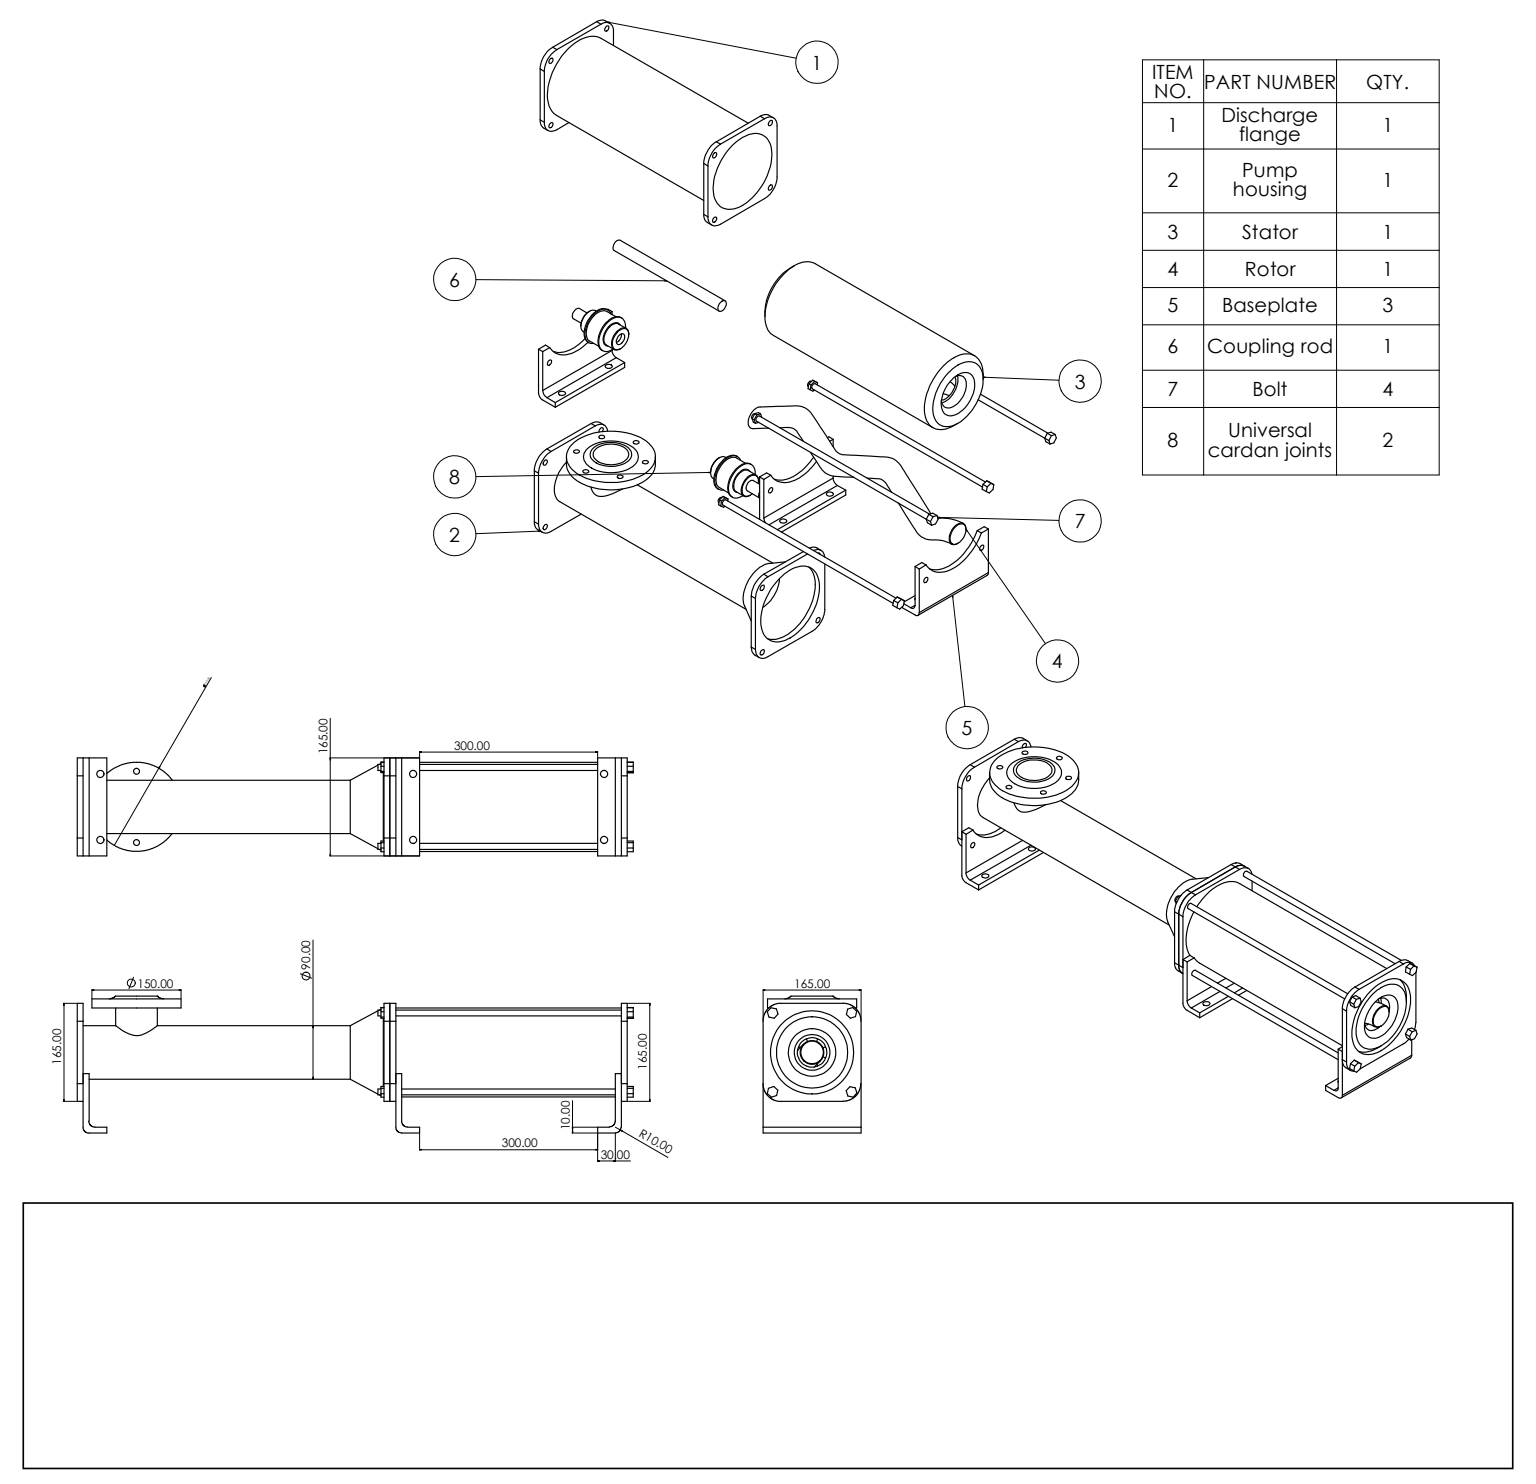
ISO-10303-21;
HEADER;
FILE_DESCRIPTION (('STEP AP214'),
    '1' );
FILE_NAME ('MAS-348',
    '2026-10-27T19:20:31',
    ( '' ),
    ( '' ),
    'SwSTEP 2.0',
    'SolidWorks 2025',
    '' );
FILE_SCHEMA (( 'AUTOMOTIVE_DESIGN' ));
ENDSEC;

DATA;
#1 = CARTESIAN_POINT ( 'NONE',  ( 14.38125909742182529, -39.99999999999944578, -55.17850393971050238 ) ) ;
#2 = CARTESIAN_POINT ( 'NONE',  ( -198.0356074513804572, -9.007331120208026888E-14, 15.37879056873070560 ) ) ;
#3 = CARTESIAN_POINT ( 'NONE',  ( 4.995406935893293543, -15.24977328854832592, 0.000000000000000000 ) ) ;
#4 = CARTESIAN_POINT ( 'NONE',  ( 163.1118516004056573, -9.006482792069636645, 9.006482792069567367 ) ) ;
#5 = CARTESIAN_POINT ( 'NONE',  ( -259.2033419157646676, 9.517827891722584255, -0.000000000000000000 ) ) ;
#6 = CARTESIAN_POINT ( 'NONE',  ( 0.2972598230770027716, -38.42060263243656237, -18.14793986248737667 ) ) ;
#7 = DIRECTION ( 'NONE',  ( 0.000000000000000000, 0.000000000000000000, -1.000000000000000000 ) ) ;
#8 =( GEOMETRIC_REPRESENTATION_CONTEXT ( 3 ) GLOBAL_UNCERTAINTY_ASSIGNED_CONTEXT ( ( #20296 ) ) GLOBAL_UNIT_ASSIGNED_CONTEXT ( ( #22388, #16248, #14122 ) ) REPRESENTATION_CONTEXT ( 'NONE', 'WORKASPACE' ) );
#9 = CARTESIAN_POINT ( 'NONE',  ( -200.0000000000000000, -52.49999999999992895, -52.49999999999999289 ) ) ;
#10 = CARTESIAN_POINT ( 'NONE',  ( 0.2972598230769957217, 1.502051041545559470E-13, -14.33493731733933352 ) ) ;
#11 = CARTESIAN_POINT ( 'NONE',  ( 130.8568914410475372, 8.154165912415230659E-16, 5.949712681206690945 ) ) ;
#12 = CARTESIAN_POINT ( 'NONE',  ( 184.8905102610680444, 13.49065550809807945, 13.49065550809809544 ) ) ;
#13 = CARTESIAN_POINT ( 'NONE',  ( 146.6084372240433709, -3.800685668859084210, 52.76785682606516303 ) ) ;
#14 = CARTESIAN_POINT ( 'NONE',  ( -190.0144721488653943, -13.91469502169275962, -47.57279682962041534 ) ) ;
#15 = CARTESIAN_POINT ( 'NONE',  ( -198.0356074513804572, -39.15871834505905724, -17.40982414986491733 ) ) ;
#16 = ORIENTED_EDGE ( 'NONE', *, *, #6629, .F. ) ;
#17 = CARTESIAN_POINT ( 'NONE',  ( 146.6084372240433993, -24.48358557860353457, 24.48358557860296258 ) ) ;
#18 = LINE ( 'NONE', #3258, #24208 ) ;
#19 = CARTESIAN_POINT ( 'NONE',  ( -192.9588430854689989, -14.46834944099973086, 0.000000000000000000 ) ) ;
#20 = CARTESIAN_POINT ( 'NONE',  ( -678.9461782662772293, 90.00000000000000000, 30.00000000000158096 ) ) ;
#21 = CARTESIAN_POINT ( 'NONE',  ( -100.7734535825088500, -44.31723036834885932, -12.25131212657538171 ) ) ;
#22 = DIRECTION ( 'NONE',  ( 0.000000000000000000, 0.000000000000000000, 1.000000000000000000 ) ) ;
#23 = CARTESIAN_POINT ( 'NONE',  ( -82.23866954411506924, 1.261533135296079022, 20.16514221458300682 ) ) ;
#24 = ORIENTED_EDGE ( 'NONE', *, *, #545, .T. ) ;
#25 = CARTESIAN_POINT ( 'NONE',  ( 199.9999999999999432, 19.00168160052138333, -0.2996653188340382967 ) ) ;
#26 = CARTESIAN_POINT ( 'NONE',  ( 22.89172254855152389, -23.44749030158411074, 43.00256445985486664 ) ) ;
#27 = CARTESIAN_POINT ( 'NONE',  ( -4.004886986946876171, 13.82996668233325721, 47.00296421444863171 ) ) ;
#28 = ORIENTED_EDGE ( 'NONE', *, *, #15718, .T. ) ;
#29 = ORIENTED_EDGE ( 'NONE', *, *, #2591, .T. ) ;
#30 = CARTESIAN_POINT ( 'NONE',  ( -208.1127848780265026, 15.00245453012665564, 0.000000000000000000 ) ) ;
#31 = CARTESIAN_POINT ( 'NONE',  ( 199.0062801237116332, 7.031410157601610145, -18.72090521856086198 ) ) ;
#32 = CARTESIAN_POINT ( 'NONE',  ( -190.0000000000000000, 52.50000000000007816, 52.49999999999999289 ) ) ;
#33 = CARTESIAN_POINT ( 'NONE',  ( -30.26275506840324070, 1.198031551616013601, 1.198031551616023371 ) ) ;
#34 = DIRECTION ( 'NONE',  ( 0.000000000000000000, 0.000000000000000000, 1.000000000000000000 ) ) ;
#35 = CARTESIAN_POINT ( 'NONE',  ( 199.9999999999999432, -1.727494763561684666E-13, 20.00000000000010303 ) ) ;
#36 = CARTESIAN_POINT ( 'NONE',  ( 200.0000000000002274, -16.15590588650048787, 10.03807108387658786 ) ) ;
#37 = CARTESIAN_POINT ( 'NONE',  ( 170.0000000000000000, 1.183443619805854272E-13, -24.95097643317000546 ) ) ;
#38 = DIRECTION ( 'NONE',  ( -1.836970198721030427E-16, 1.000000000000000000, -1.682156097916904327E-16 ) ) ;
#39 = CARTESIAN_POINT ( 'NONE',  ( 199.0246859915949642, -4.071254240408448410, 19.58630271169732140 ) ) ;
#40 = DIRECTION ( 'NONE',  ( 0.000000000000000000, -0.000000000000000000, 1.000000000000000000 ) ) ;
#41 = CARTESIAN_POINT ( 'NONE',  ( 12.96694272553733107, -24.77464205076947223, -44.79869582454342236 ) ) ;
#42 = CARTESIAN_POINT ( 'NONE',  ( -213.1075012329536946, -37.98287015391210275, -37.98287015391272092 ) ) ;
#43 = EDGE_CURVE ( 'NONE', #19077, #10069, #15238, .T. ) ;
#44 = CARTESIAN_POINT ( 'NONE',  ( -200.0000000000000000, 18.14877749763656212, 46.38610861938588670 ) ) ;
#45 = CARTESIAN_POINT ( 'NONE',  ( 146.6084372240433709, -32.08495691632041513, -24.48358557860343154 ) ) ;
#46 = CARTESIAN_POINT ( 'NONE',  ( -77.61444910505676376, 3.470426107442325048, 21.81614215779332966 ) ) ;
#47 = CARTESIAN_POINT ( 'NONE',  ( -213.1075012329537230, -9.698598906450422774, -9.698598906450550672 ) ) ;
#48 = CARTESIAN_POINT ( 'NONE',  ( -208.1127848780264742, -55.00245453012676222, -2.449293598294708485E-15 ) ) ;
#49 = EDGE_CURVE ( 'NONE', #17928, #4130, #15424, .T. ) ;
#50 = FACE_OUTER_BOUND ( 'NONE', #10007, .T. ) ;
#51 = CIRCLE ( 'NONE', #14477, 30.00000000000003908 ) ;
#52 = CARTESIAN_POINT ( 'NONE',  ( -192.9588430854689705, -54.46834944099975928, -2.449293598294708485E-15 ) ) ;
#53 = AXIS2_PLACEMENT_3D ( 'NONE', #25264, #21266, #19008 ) ;
#54 = CARTESIAN_POINT ( 'NONE',  ( -114.6180193230984372, 19.15387080987368762, 10.88873798880637622 ) ) ;
#55 = CARTESIAN_POINT ( 'NONE',  ( -30.26275506840325136, 40.00000000000003553, -1.694272468445841007 ) ) ;
#56 = EDGE_CURVE ( 'NONE', #12829, #11587, #7928, .T. ) ;
#57 = CARTESIAN_POINT ( 'NONE',  ( -30.26275506840325136, 29.48230279907798135, -27.08623969584585112 ) ) ;
#58 = EDGE_CURVE ( 'NONE', #18547, #5841, #11121, .T. ) ;
#59 = CARTESIAN_POINT ( 'NONE',  ( -198.0356074513804572, 15.37879056873066830, -40.00000000000002132 ) ) ;
#60 = VERTEX_POINT ( 'NONE', #18074 ) ;
#61 = VERTEX_POINT ( 'NONE', #13950 ) ;
#62 = CARTESIAN_POINT ( 'NONE',  ( 146.6084372240433709, -34.62501878078303008, 40.00000000000002132 ) ) ;
#63 = CARTESIAN_POINT ( 'NONE',  ( -86.86493150571118349, -7.943527260495776510, -19.77569912839190280 ) ) ;
#64 = CARTESIAN_POINT ( 'NONE',  ( -259.2033419157646676, -40.00000000000017764, 30.48217210827725054 ) ) ;
#65 = CIRCLE ( 'NONE', #6032, 14.99999999999999822 ) ;
#66 = CARTESIAN_POINT ( 'NONE',  ( -259.2033419157646676, 21.55415060305860209, -21.55415060305812602 ) ) ;
#67 = CARTESIAN_POINT ( 'NONE',  ( -280.0000000000000568, -20.00000000000006750, 40.00000000000002132 ) ) ;
#68 = CARTESIAN_POINT ( 'NONE',  ( -210.0000000000000284, -52.49999999999991473, 82.49999999999998579 ) ) ;
#69 = DIRECTION ( 'NONE',  ( 1.018913292508929218E-14, 1.000000000000000000, 8.144542348679703993E-15 ) ) ;
#70 = CARTESIAN_POINT ( 'NONE',  ( 200.0000000000001421, 16.62132632430557777, -9.210632111445709924 ) ) ;
#71 = CARTESIAN_POINT ( 'NONE',  ( 199.9999999999999432, -18.84870794256249482, 2.485603278128234450 ) ) ;
#72 = CARTESIAN_POINT ( 'NONE',  ( 91.82158438592158234, 44.40256751092319121, 12.16597498400105515 ) ) ;
#73 = CARTESIAN_POINT ( 'NONE',  ( -91.56559293963836410, -12.25131212657524138, 44.31723036834888774 ) ) ;
#74 = DIRECTION ( 'NONE',  ( -1.000000000000000000, 0.000000000000000000, 0.000000000000000000 ) ) ;
#75 = CARTESIAN_POINT ( 'NONE',  ( 14.38125909742181108, 1.616281842095393922E-13, -15.17850393972633682 ) ) ;
#76 = CARTESIAN_POINT ( 'NONE',  ( -198.0356074513804572, -67.44298959253333692, -10.87444709761016348 ) ) ;
#77 = CARTESIAN_POINT ( 'NONE',  ( -87.08883615166502068, 12.58652615577663170, -17.39726528837345398 ) ) ;
#78 = CARTESIAN_POINT ( 'NONE',  ( -213.1075012329537230, -18.58567234101155208, 37.98287015391234434 ) ) ;
#79 = CARTESIAN_POINT ( 'NONE',  ( -100.7734535825088500, -12.25131212657462498, -44.31723036834905827 ) ) ;
#80 = CARTESIAN_POINT ( 'NONE',  ( 199.0199757207951734, 7.646550829590152532, 18.48267855362066214 ) ) ;
#82 = CARTESIAN_POINT ( 'NONE',  ( -208.1127848780265026, -2.327190355601776466E-13, 55.00245453012672670 ) ) ;
#81 = CARTESIAN_POINT ( 'NONE',  ( -100.7734535825088358, 12.25131212657497848, -12.25131212657469604 ) ) ;
#83 = CARTESIAN_POINT ( 'NONE',  ( 19.06497207195980792, 66.60410523465830579, -10.03556273973354251 ) ) ;
#84 = AXIS2_PLACEMENT_3D ( 'NONE', #861, #18677, #15078 ) ;
#85 = CARTESIAN_POINT ( 'NONE',  ( 23.42154907652883011, 42.84253412640345715, -23.32998349128526883 ) ) ;
#86 = CARTESIAN_POINT ( 'NONE',  ( 192.4448373802100889, 19.99999999996064304, 2.449293598294708485E-15 ) ) ;
#87 = VERTEX_POINT ( 'NONE', #1727 ) ;
#88 = CARTESIAN_POINT ( 'NONE',  ( 192.4448373802100889, -14.14213562375876698, -14.14213562375885047 ) ) ;
#89 = CARTESIAN_POINT ( 'NONE',  ( -62.79433447042063676, -25.93934121795946268, 9.335111860881914581 ) ) ;
#90 = CARTESIAN_POINT ( 'NONE',  ( -280.0000000000000568, 19.99999999999995737, 40.00000000000002132 ) ) ;
#91 = ORIENTED_EDGE ( 'NONE', *, *, #1926, .F. ) ;
#92 = CARTESIAN_POINT ( 'NONE',  ( 12.01361959687201519, 24.84115733209565136, -44.88892880200794622 ) ) ;
#93 = CARTESIAN_POINT ( 'NONE',  ( 199.9999999999998863, -17.04947422730185025, -8.406841951002201441 ) ) ;
#94 = CARTESIAN_POINT ( 'NONE',  ( 20.91285618074969221, -23.84652503050088512, 43.54130497316993598 ) ) ;
#95 = CARTESIAN_POINT ( 'NONE',  ( -2.164901439630326330, 23.84421257770968339, -43.53794903252429549 ) ) ;
#96 = CARTESIAN_POINT ( 'NONE',  ( 199.0132273568269170, -10.00203194272371476, -17.32088655864767190 ) ) ;
#97 = VECTOR ( 'NONE', #21456, 1000.000000000000000 ) ;
#98 = CARTESIAN_POINT ( 'NONE',  ( 151.7948205124836250, -3.202120068677277203E-13, 33.23291073765553705 ) ) ;
#99 = CARTESIAN_POINT ( 'NONE',  ( 154.0339099654741801, -28.18615453125293513, 11.67508747798861002 ) ) ;
#100 = CARTESIAN_POINT ( 'NONE',  ( -166.3490736466491740, -19.13702016930768579, 36.43932733844285821 ) ) ;
#101 = CARTESIAN_POINT ( 'NONE',  ( 163.1118516004056573, 9.006482792069759213, -9.006482792069505194 ) ) ;
#102 = DIRECTION ( 'NONE',  ( -1.000000000000000000, -1.836970198721030181E-16, 0.000000000000000000 ) ) ;
#104 = CARTESIAN_POINT ( 'NONE',  ( 91.82158438592158234, -12.16597498397778843, 12.16597498397750954 ) ) ;
#103 = CARTESIAN_POINT ( 'NONE',  ( -188.4265466358324090, 13.83489705870430519, -47.03621809928684172 ) ) ;
#105 = CARTESIAN_POINT ( 'NONE',  ( -56.48582580120559271, -6.472252184284276844, 6.472252184284108978 ) ) ;
#106 = CARTESIAN_POINT ( 'NONE',  ( 91.82158438592159655, -22.79471317813468545, -40.00000000000002132 ) ) ;
#107 = CARTESIAN_POINT ( 'NONE',  ( -208.1127848780264742, 55.00245453010919050, -40.00000000000002132 ) ) ;
#108 = CARTESIAN_POINT ( 'NONE',  ( -105.3755690713226585, -40.00000000000027711, 21.75974354311608749 ) ) ;
#109 = CARTESIAN_POINT ( 'NONE',  ( 0.2972598230770011618, 10.13633138497462305, 66.70487387989858519 ) ) ;
#110 = CARTESIAN_POINT ( 'NONE',  ( -96.94475454975007267, 20.58449551010169998, -9.001119816636389714 ) ) ;
#111 = CARTESIAN_POINT ( 'NONE',  ( 130.8568914410475372, -4.207082182992785135, -4.207082182992884611 ) ) ;
#112 = ORIENTED_EDGE ( 'NONE', *, *, #21174, .F. ) ;
#113 = CARTESIAN_POINT ( 'NONE',  ( 0.2972598230769938343, 10.13633138497472252, 10.13633138497475628 ) ) ;
#114 = CARTESIAN_POINT ( 'NONE',  ( -97.73806390046776471, 8.581719943994480460, 20.71810467721184423 ) ) ;
#115 = CONTEXT_DEPENDENT_SHAPE_REPRESENTATION ( #703, #24194 ) ;
#116 = ORIENTED_EDGE ( 'NONE', *, *, #25089, .T. ) ;
#117 = EDGE_CURVE ( 'NONE', #6149, #16510, #26225, .T. ) ;
#118 = ORIENTED_EDGE ( 'NONE', *, *, #8682, .F. ) ;
#119 = B_SPLINE_CURVE_WITH_KNOTS ( 'NONE', 3,
 ( #4293, #2821, #10524, #19041, #16643, #4682, #8526, #24772, #8927, #6525, #20776, #20510, #2282, #14636, #22773, #8662, #10391, #6395, #24904, #14511, #14774, #22904, #12785, #20912, #2691, #18907, #15039, #23170, #13054, #25298, #21172, #4948, #17164, #2945 ),
 .UNSPECIFIED., .F., .F.,
 ( 4, 2, 2, 2, 2, 2, 2, 2, 2, 2, 2, 2, 2, 2, 2, 2, 4 ),
 ( -5.298243351204090312E-05, 0.01887868273877536807, 0.02834451532491907844, 0.03071097347145498174, 0.03307743161799089199, 0.03544388976452679529, 0.03781034791106269860, 0.04254326420413442889, 0.04727618049720615223, 0.04964263864374202084, 0.05200909679027788945, 0.05674201308334969607, 0.05910847122988561325, 0.06029170030315351980, 0.06147492937642144023, 0.06620784566949308725, 0.07567367825563638128 ),
 .UNSPECIFIED. ) ;
#120 = CARTESIAN_POINT ( 'NONE',  ( 57.59792236341147031, -26.56190807104670171, -30.00663442387710234 ) ) ;
#121 = CARTESIAN_POINT ( 'NONE',  ( 22.75882399337409367, -43.17886244245828919, -17.88527043150862283 ) ) ;
#122 = VERTEX_POINT ( 'NONE', #3583 ) ;
#123 = CARTESIAN_POINT ( 'NONE',  ( 151.7948205124836250, -33.23291073765550863, 0.000000000000000000 ) ) ;
#124 = CARTESIAN_POINT ( 'NONE',  ( -77.90255099906771363, -8.644468104261237684, -20.04994828523970440 ) ) ;
#125 = ORIENTED_EDGE ( 'NONE', *, *, #9291, .T. ) ;
#126 = SHAPE_REPRESENTATION ( 'Rotor', ( #21058 ), #20184 ) ;
#127 = CARTESIAN_POINT ( 'NONE',  ( 199.9999999999999432, 17.49244587396685091, 7.427265670988617785 ) ) ;
#128 = CARTESIAN_POINT ( 'NONE',  ( -83.21262154144230294, -33.12752917117752105, 13.72187187063023472 ) ) ;
#129 = CARTESIAN_POINT ( 'NONE',  ( -86.96347745069644475, 12.89780903124410472, -43.67073346367977393 ) ) ;
#130 = CARTESIAN_POINT ( 'NONE',  ( -187.8779108535587739, -43.02987313851080131, -17.82355704116172745 ) ) ;
#131 = CARTESIAN_POINT ( 'NONE',  ( 0.2972598230770030492, -40.00000000000007816, 14.33493731733919496 ) ) ;
#132 = CARTESIAN_POINT ( 'NONE',  ( 4.995406935893288214, 15.24977328854832770, 0.000000000000000000 ) ) ;
#133 = CARTESIAN_POINT ( 'NONE',  ( -259.2033419157646676, 21.55415060305860209, -21.55415060305812602 ) ) ;
#134 = CARTESIAN_POINT ( 'NONE',  ( 199.0221265002223845, 3.088699012602908578, 19.76381171561452632 ) ) ;
#135 = CARTESIAN_POINT ( 'NONE',  ( 200.0000000000000000, -39.99999999999991473, -20.00000000000024514 ) ) ;
#136 = CARTESIAN_POINT ( 'NONE',  ( 192.4448373802100889, -3.692737725850373501E-14, 19.99999999996060751 ) ) ;
#137 = CARTESIAN_POINT ( 'NONE',  ( -100.7734535825088500, 40.00000000000008527, -22.67402823373177512 ) ) ;
#138 = CARTESIAN_POINT ( 'NONE',  ( -30.26275506840324425, -1.694272468446265334, -40.00000000000002132 ) ) ;
#139 = CARTESIAN_POINT ( 'NONE',  ( 200.0000000000000000, -42.42640687119269671, -14.14213562373124766 ) ) ;
#140 = CARTESIAN_POINT ( 'NONE',  ( 192.4448373802100889, 20.00000000003945644, 0.000000000000000000 ) ) ;
#141 = ADVANCED_FACE ( 'NONE', ( #24347 ), #25952, .T. ) ;
#142 = CARTESIAN_POINT ( 'NONE',  ( -56.48582580120558561, -21.81201906317785699, 21.81201906317761896 ) ) ;
#143 = DIRECTION ( 'NONE',  ( 0.000000000000000000, 1.000000000000000000, 0.000000000000000000 ) ) ;
#144 = DIRECTION ( 'NONE',  ( 0.000000000000000000, 0.000000000000000000, 1.000000000000000000 ) ) ;
#145 = CARTESIAN_POINT ( 'NONE',  ( 57.59792236341147031, 40.00000000000042633, -37.56421063658144277 ) ) ;
#146 = CARTESIAN_POINT ( 'NONE',  ( 184.8905102610680444, -40.00000000000005684, 19.07866798485543569 ) ) ;
#147 = CARTESIAN_POINT ( 'NONE',  ( -259.2033419157646676, 21.55415060305839958, -35.01439189186541512 ) ) ;
#148 = CARTESIAN_POINT ( 'NONE',  ( -114.7173660547197045, 17.99555204289530863, 12.80183536318784299 ) ) ;
#149 = CARTESIAN_POINT ( 'NONE',  ( -193.3669098795559194, -18.32287322058442314, -44.23532903077867218 ) ) ;
#150 = CARTESIAN_POINT ( 'NONE',  ( 91.82158438592159655, -44.40256751092324095, -12.16597498400075139 ) ) ;
#151 = VERTEX_POINT ( 'NONE', #13812 ) ;
#152 = CARTESIAN_POINT ( 'NONE',  ( -192.9588430854690273, -18.05360324515400094, -38.51493924976961836 ) ) ;
#153 = DIRECTION ( 'NONE',  ( 1.000000000000000000, -0.000000000000000000, -0.000000000000000000 ) ) ;
#154 = CARTESIAN_POINT ( 'NONE',  ( -30.26275506840324425, -1.694272468446265334, -40.00000000000002132 ) ) ;
#155 = CARTESIAN_POINT ( 'NONE',  ( 190.0000000000000000, -66.50000000000001421, -66.50000000000005684 ) ) ;
#156 = CARTESIAN_POINT ( 'NONE',  ( -259.2033419157646676, -6.730120644403663199, 6.730120644403451813 ) ) ;
#157 = ORIENTED_EDGE ( 'NONE', *, *, #1849, .F. ) ;
#158 = ORIENTED_EDGE ( 'NONE', *, *, #24110, .F. ) ;
#159 = CARTESIAN_POINT ( 'NONE',  ( 199.9999999999999716, 8.674762155946922348, 16.91470172953081885 ) ) ;
#160 = LINE ( 'NONE', #12392, #2622 ) ;
#161 = CARTESIAN_POINT ( 'NONE',  ( -7.769366557097702852, 22.72119856430158791, 41.90323276218021675 ) ) ;
#162 = VERTEX_POINT ( 'NONE', #11961 ) ;
#163 = ORIENTED_EDGE ( 'NONE', *, *, #20627, .T. ) ;
#164 = CARTESIAN_POINT ( 'NONE',  ( -198.0356074513804572, 10.87444709759714989, 10.87444709759722450 ) ) ;
#165 = CARTESIAN_POINT ( 'NONE',  ( 199.0071786209885261, 3.739031945787267386, -19.64359944086908527 ) ) ;
#166 = CARTESIAN_POINT ( 'NONE',  ( -77.58504658647395047, -13.57342497464155429, -17.50304285594473086 ) ) ;
#167 = CARTESIAN_POINT ( 'NONE',  ( 14.38125909742180752, 10.73282306404720465, 10.73282306404724018 ) ) ;
#168 = CARTESIAN_POINT ( 'NONE',  ( 0.2972598230770030492, 5.716321584140269555E-13, -54.33493731733936016 ) ) ;
#169 = DIRECTION ( 'NONE',  ( 0.000000000000000000, -1.000000000000000000, 0.000000000000000000 ) ) ;
#170 = CARTESIAN_POINT ( 'NONE',  ( -654.9559990268497813, 38.50095308322672594, 10.88967829900012418 ) ) ;
#171 = CARTESIAN_POINT ( 'NONE',  ( -200.0000000000000000, -66.50000000000001421, -66.50000000000005684 ) ) ;
#172 = CARTESIAN_POINT ( 'NONE',  ( 199.0185982156405089, 10.13449990482401297, 17.24443922940779927 ) ) ;
#173 = CARTESIAN_POINT ( 'NONE',  ( -183.6284948306234810, 17.34366805700532410, 41.87131864452296526 ) ) ;
#174 = CARTESIAN_POINT ( 'NONE',  ( 23.37583784646126617, -23.33923448557677105, -42.85659535397680031 ) ) ;
#175 = CARTESIAN_POINT ( 'NONE',  ( 57.59792236341148453, -26.56190807104663421, -26.56190807104710672 ) ) ;
#176 = CARTESIAN_POINT ( 'NONE',  ( -94.58366989427224780, 20.58370269626824012, -9.000605044545586964 ) ) ;
#177 = CARTESIAN_POINT ( 'NONE',  ( -280.0000000000000000, -14.14213562373108779, 14.14213562373088529 ) ) ;
#178 = CYLINDRICAL_SURFACE ( 'NONE', #9570, 69.99999999999998579 ) ;
#179 = CARTESIAN_POINT ( 'NONE',  ( 19.06497207195982924, -54.19242893257843008, -2.449293598294708485E-15 ) ) ;
#180 = FACE_OUTER_BOUND ( 'NONE', #16206, .T. ) ;
#181 = CARTESIAN_POINT ( 'NONE',  ( -208.1127848780264742, -55.00245453012676222, -2.449293598294708485E-15 ) ) ;
#182 = CARTESIAN_POINT ( 'NONE',  ( -114.6133217222730991, 10.93740326486608083, 19.07173553325018389 ) ) ;
#183 = CARTESIAN_POINT ( 'NONE',  ( -105.3755690713226585, 40.00000000000019185, -18.24025645688310249 ) ) ;
#184 = CARTESIAN_POINT ( 'NONE',  ( -259.2033419157646676, -6.730120644403570829, -6.730120644403545960 ) ) ;
#185 = CARTESIAN_POINT ( 'NONE',  ( -91.56559293963834989, -22.67402823373193499, -40.00000000000002132 ) ) ;
#186 = ORIENTED_EDGE ( 'NONE', *, *, #13817, .T. ) ;
#187 = EDGE_LOOP ( 'NONE', ( #24603, #23674, #1863, #22741 ) ) ;
#188 = ORIENTED_EDGE ( 'NONE', *, *, #14494, .T. ) ;
#189 = CARTESIAN_POINT ( 'NONE',  ( -280.0000000000000568, 19.99999999999995737, 40.00000000000002132 ) ) ;
#190 = EDGE_CURVE ( 'NONE', #22454, #4199, #20086, .T. ) ;
#191 = CARTESIAN_POINT ( 'NONE',  ( -56.48582580120559982, 50.09629031063956717, 6.472252184284792875 ) ) ;
#192 = CARTESIAN_POINT ( 'NONE',  ( -110.0685463886591293, -19.46857821975389058, -5.325649136242457615 ) ) ;
#193 = ADVANCED_FACE ( 'NONE', ( #5707 ), #22219, .T. ) ;
#194 = DIRECTION ( 'NONE',  ( 0.000000000000000000, -0.9767746502210199466, 0.2142691827715878239 ) ) ;
#195 = PRODUCT ( 'Universal cardan joints', 'Universal cardan joints', '', ( #26348 ) ) ;
#196 = CARTESIAN_POINT ( 'NONE',  ( 210.0000000000000284, 61.50000000000009948, -66.50000000000005684 ) ) ;
#197 = CARTESIAN_POINT ( 'NONE',  ( 200.0000000000001705, 18.83917254958691601, 2.502331228272203223 ) ) ;
#198 = ADVANCED_FACE ( 'NONE', ( #23801 ), #14342, .T. ) ;
#199 = ADVANCED_FACE ( 'NONE', ( #14088 ), #12427, .T. ) ;
#200 = CARTESIAN_POINT ( 'NONE',  ( 199.9999999999999716, -19.00887936793599664, -0.3109487220520843476 ) ) ;
#201 = CARTESIAN_POINT ( 'NONE',  ( 136.1360204305621551, 31.79587985999232558, 24.77266263493161702 ) ) ;
#202 = CARTESIAN_POINT ( 'NONE',  ( 184.8905102610680444, -41.77492675556007384, 14.79361573936348684 ) ) ;
#203 = DIRECTION ( 'NONE',  ( -0.2259624730582342200, 0.000000000000000000, -0.9741360073261878805 ) ) ;
#204 = CARTESIAN_POINT ( 'NONE',  ( 19.06497207195979726, 40.00000000000017053, -14.19242893257798599 ) ) ;
#205 = CARTESIAN_POINT ( 'NONE',  ( 146.6084372240433993, -3.800685668858596156, -3.800685668858692967 ) ) ;
#206 = CARTESIAN_POINT ( 'NONE',  ( 163.1118516004056573, -19.27778845538787422, 19.27778845538743724 ) ) ;
#207 = CARTESIAN_POINT ( 'NONE',  ( -198.0356074513804572, -17.40982414986482141, 39.15871834505909987 ) ) ;
#208 = CARTESIAN_POINT ( 'NONE',  ( 163.1118516004056573, -9.006482792073960297, -47.56205970284963769 ) ) ;
#209 = CARTESIAN_POINT ( 'NONE',  ( 199.0242990326260042, -2.747623036511753991, 19.85784534697798875 ) ) ;
#211 = CARTESIAN_POINT ( 'NONE',  ( -100.7734535825088500, 39.99999999999994316, 17.32597176626825686 ) ) ;
#210 = CARTESIAN_POINT ( 'NONE',  ( 0.2972598230769959993, 38.42060263243713081, -38.42060263243619289 ) ) ;
#212 = CARTESIAN_POINT ( 'NONE',  ( 146.6084372240433709, 3.800685668858042821, 52.76785682606522698 ) ) ;
#213 = CARTESIAN_POINT ( 'NONE',  ( 19.94008347562116512, 43.76810615267693549, -24.01421467034480273 ) ) ;
#214 = CARTESIAN_POINT ( 'NONE',  ( -135.8532207217289738, -9.153146818113595984, -40.00000000000002132 ) ) ;
#215 = CARTESIAN_POINT ( 'NONE',  ( 8.517493242715996615, -24.85395068094629067, -44.90626920808422540 ) ) ;
#216 = CARTESIAN_POINT ( 'NONE',  ( -4.082462733454099713, -46.97557262069199879, 13.82507958736570153 ) ) ;
#217 = CARTESIAN_POINT ( 'NONE',  ( 130.8568914410475088, 5.949712681206712261, 40.00000000000002132 ) ) ;
#218 = VERTEX_POINT ( 'NONE', #16347 ) ;
#219 = CARTESIAN_POINT ( 'NONE',  ( 7.307793593482434957, 24.85783611765758039, -44.91153572052478893 ) ) ;
#220 = CARTESIAN_POINT ( 'NONE',  ( -259.2033419157646676, -35.01439189186554302, 21.55415060305832498 ) ) ;
#221 = CARTESIAN_POINT ( 'NONE',  ( -16.87994666136603072, -20.93785811888612258, 39.19724034055838757 ) ) ;
#222 =( GEOMETRIC_REPRESENTATION_CONTEXT ( 3 ) GLOBAL_UNCERTAINTY_ASSIGNED_CONTEXT ( ( #25788 ) ) GLOBAL_UNIT_ASSIGNED_CONTEXT ( ( #19170, #953, #19420 ) ) REPRESENTATION_CONTEXT ( 'NONE', 'WORKASPACE' ) );
#223 = CARTESIAN_POINT ( 'NONE',  ( -3.696864809820620934, 13.84627154338459931, -47.11278487914880486 ) ) ;
#224 = CARTESIAN_POINT ( 'NONE',  ( 199.0143331921596257, -11.79252763263196613, -16.15335214697885391 ) ) ;
#225 = EDGE_CURVE ( 'NONE', #2033, #22654, #7079, .T. ) ;
#226 = CARTESIAN_POINT ( 'NONE',  ( -56.48582580120559271, -1.062504017861011783E-13, 9.153146818113587102 ) ) ;
#227 = CARTESIAN_POINT ( 'NONE',  ( 167.0466155511621480, -23.44215416552593467, 9.710058186601612462 ) ) ;
#228 = CARTESIAN_POINT ( 'NONE',  ( -188.6890294954723117, -13.84869711777589885, 47.12920239600079242 ) ) ;
#229 = CARTESIAN_POINT ( 'NONE',  ( 14.38125909742181463, 10.73282306403652875, -67.30136555895941797 ) ) ;
#230 = CARTESIAN_POINT ( 'NONE',  ( -100.7734535825088500, 22.67402823373189591, -0.000000000000000000 ) ) ;
#231 = AXIS2_PLACEMENT_3D ( 'NONE', #20688, #10567, #468 ) ;
#232 = CIRCLE ( 'NONE', #10863, 5.000000000000004441 ) ;
#234 = CARTESIAN_POINT ( 'NONE',  ( -135.8532207217289738, -6.472252184284280396, 6.472252184284099208 ) ) ;
#233 = CARTESIAN_POINT ( 'NONE',  ( -194.7884774423580154, 18.40784251727735565, -44.44046305924767637 ) ) ;
#235 = CARTESIAN_POINT ( 'NONE',  ( -135.8532207217289738, 50.09629031063956006, 6.472252184284782217 ) ) ;
#236 = CARTESIAN_POINT ( 'NONE',  ( -100.7734535825088500, -17.32597176626813251, 40.00000000000002132 ) ) ;
#237 = CARTESIAN_POINT ( 'NONE',  ( 146.6084372240433993, 5.374981219216999229, 2.449293598294708485E-15 ) ) ;
#238 = CARTESIAN_POINT ( 'NONE',  ( 4.995406935893290878, 1.606505379428369110E-13, -15.24977328854832592 ) ) ;
#239 = CARTESIAN_POINT ( 'NONE',  ( 136.1360204305621551, -24.77266263493126885, 31.79587985999256006 ) ) ;
#240 = CARTESIAN_POINT ( 'NONE',  ( -94.58414068580489698, 20.73981583682122576, -8.590713000717968839 ) ) ;
#241 = CARTESIAN_POINT ( 'NONE',  ( 184.8905102610680444, 43.07788698682591644, -13.49065550809769221 ) ) ;
#242 = CARTESIAN_POINT ( 'NONE',  ( -213.1075012329537230, -9.698598906450557777, 9.698598906450415669 ) ) ;
#243 = ORIENTED_EDGE ( 'NONE', *, *, #21209, .F. ) ;
#244 = AXIS2_PLACEMENT_3D ( 'NONE', #3180, #21532, #25538 ) ;
#245 = CARTESIAN_POINT ( 'NONE',  ( 151.7948205124836534, -51.78348778862535795, 4.785054706298367044 ) ) ;
#246 = AXIS2_PLACEMENT_3D ( 'NONE', #22417, #6170, #12157 ) ;
#247 = AXIS2_PLACEMENT_3D ( 'NONE', #22404, #17983, #169 ) ;
#248 = CARTESIAN_POINT ( 'NONE',  ( -200.0000000000001421, -14.17215463606902404, -49.28189405767602693 ) ) ;
#249 = CARTESIAN_POINT ( 'NONE',  ( -91.56559293963834989, 6.234561990864368500E-14, -22.67402823373191723 ) ) ;
#250 = CARTESIAN_POINT ( 'NONE',  ( 91.82158438592159655, 12.16597498400028776, 44.40256751092339016 ) ) ;
#251 = CARTESIAN_POINT ( 'NONE',  ( -3.379936260374155399, -43.32059152999958940, -17.94397654175126888 ) ) ;
#252 = EDGE_LOOP ( 'NONE', ( #14876, #22901, #13781, #8671 ) ) ;
#253 = DIRECTION ( 'NONE',  ( 0.000000000000000000, 1.000000000000000000, 0.000000000000000000 ) ) ;
#254 = DIRECTION ( 'NONE',  ( 0.000000000000000000, 0.000000000000000000, 1.000000000000000000 ) ) ;
#255 = ORIENTED_EDGE ( 'NONE', *, *, #15646, .F. ) ;
#256 = CARTESIAN_POINT ( 'NONE',  ( 199.9999999999998295, 18.60987205011830881, -3.837998380785754726 ) ) ;
#257 = CIRCLE ( 'NONE', #21922, 30.00000000000000355 ) ;
#258 = PLANE ( 'NONE',  #2201 ) ;
#259 = CARTESIAN_POINT ( 'NONE',  ( 184.8905102610680444, -14.79361573936379415, -14.79361573936387941 ) ) ;
#260 = CARTESIAN_POINT ( 'NONE',  ( -188.3066136396997479, -46.99300418776440580, -13.82848859481202553 ) ) ;
#261 = CARTESIAN_POINT ( 'NONE',  ( -208.1127848780265026, -2.327190355601776466E-13, 55.00245453012672670 ) ) ;
#262 = CARTESIAN_POINT ( 'NONE',  ( 163.1118516004056573, 12.73709011382477918, 40.00000000000002132 ) ) ;
#263 = CARTESIAN_POINT ( 'NONE',  ( -208.1127848780265026, 10.60833733269551615, -10.60833733269529766 ) ) ;
#264 = CARTESIAN_POINT ( 'NONE',  ( 199.0256575778758474, -7.963596585350240176, 18.35421432800287533 ) ) ;
#265 = CIRCLE ( 'NONE', #15136, 44.99999999999997158 ) ;
#266 = CARTESIAN_POINT ( 'NONE',  ( -192.9588430854690273, -40.00000000000024158, 54.46834944101708231 ) ) ;
#267 = CARTESIAN_POINT ( 'NONE',  ( 170.2234770963711128, 40.00000000000000000, 15.44714144992830462 ) ) ;
#268 = CARTESIAN_POINT ( 'NONE',  ( -208.1127848780265026, -9.061048840815752106E-14, 15.00245453012669472 ) ) ;
#269 = DIRECTION ( 'NONE',  ( 0.000000000000000000, -1.000000000000000000, 0.000000000000000000 ) ) ;
#270 = CARTESIAN_POINT ( 'NONE',  ( 14.38125909742182884, -55.17850393972636169, -2.449293598294708485E-15 ) ) ;
#271 = CARTESIAN_POINT ( 'NONE',  ( -238.4067589809705794, -0.6820004458488042598, 57.25054294077229855 ) ) ;
#272 = CARTESIAN_POINT ( 'NONE',  ( -280.0000000000000000, -2.609240458947769655E-13, 20.00000000000001421 ) ) ;
#273 = CARTESIAN_POINT ( 'NONE',  ( 1.564252679174732208, -48.56509332159251358, 14.06374044400967271 ) ) ;
#274 = CARTESIAN_POINT ( 'NONE',  ( 136.1360204305621266, 7.947488714877270288E-14, -4.966164525587064560 ) ) ;
#275 = CARTESIAN_POINT ( 'NONE',  ( -100.7734535825088500, -40.00000000000009948, 17.32597176626796909 ) ) ;
#276 = CARTESIAN_POINT ( 'NONE',  ( -259.2033419157646676, -6.730120644403570829, -6.730120644403545960 ) ) ;
#277 = AXIS2_PLACEMENT_3D ( 'NONE', #11873, #9385, #1278 ) ;
#278 = CARTESIAN_POINT ( 'NONE',  ( -188.2995950289364941, -46.99046209955426434, -13.82811170417247126 ) ) ;
#279 = CARTESIAN_POINT ( 'NONE',  ( -97.72675010090328840, -8.987772175319422630, -20.56394680065913505 ) ) ;
#280 = CARTESIAN_POINT ( 'NONE',  ( 200.0000000000000000, -42.42640687119269671, -14.14213562373124766 ) ) ;
#281 = ORIENTED_EDGE ( 'NONE', *, *, #13368, .T. ) ;
#282 = CARTESIAN_POINT ( 'NONE',  ( 151.7948205124836534, -23.49921654115981084, -33.06932595376387951 ) ) ;
#283 = CARTESIAN_POINT ( 'NONE',  ( -200.0000000000000000, 52.49999999999987210, -82.49999999999998579 ) ) ;
#284 = CARTESIAN_POINT ( 'NONE',  ( -91.56559293963834989, -17.32597176626812185, -40.00000000000002132 ) ) ;
#285 = CARTESIAN_POINT ( 'NONE',  ( -114.4364955367336449, 20.04994829326807348, -8.644468109231272734 ) ) ;
#286 = CARTESIAN_POINT ( 'NONE',  ( -259.2033419157646676, -9.517827891722680178, 0.000000000000000000 ) ) ;
#287 = VERTEX_POINT ( 'NONE', #6242 ) ;
#288 = ORIENTED_EDGE ( 'NONE', *, *, #2639, .F. ) ;
#289 = CARTESIAN_POINT ( 'NONE',  ( 199.9999999999999716, 17.03617407744741641, 8.421988063785285306 ) ) ;
#290 = CARTESIAN_POINT ( 'NONE',  ( -97.73860346102746632, 8.987542150733535351, -20.56359266934956764 ) ) ;
#291 = ADVANCED_FACE ( 'NONE', ( #12485 ), #392, .F. ) ;
#292 = CARTESIAN_POINT ( 'NONE',  ( 23.36462152322931374, 23.34178792078241216, 42.86003749000698804 ) ) ;
#293 = ORIENTED_EDGE ( 'NONE', *, *, #21671, .T. ) ;
#294 = AXIS2_PLACEMENT_3D ( 'NONE', #8252, #14768, #20771 ) ;
#295 = CIRCLE ( 'NONE', #24520, 34.99999999999999289 ) ;
#296 = ORIENTED_EDGE ( 'NONE', *, *, #19861, .T. ) ;
#297 = CARTESIAN_POINT ( 'NONE',  ( -91.56559293963834989, -16.03295912088706388, -16.03295912088710651 ) ) ;
#298 = CARTESIAN_POINT ( 'NONE',  ( 199.0116000645839449, -7.055149577161559549, -18.71482085160166875 ) ) ;
#299 = DIRECTION ( 'NONE',  ( -1.000000000000000000, -0.000000000000000000, -0.000000000000000000 ) ) ;
#300 = ADVANCED_FACE ( 'NONE', ( #8363, #8229, #20751, #2125, #20481, #18473 ), #22483, .F. ) ;
#301 = CARTESIAN_POINT ( 'NONE',  ( 35.93702930694564657, 42.26928858314015258, -12.87541766278293665 ) ) ;
#302 = CARTESIAN_POINT ( 'NONE',  ( -280.0000000000000568, 14.14213562373097943, -42.42640687119285303 ) ) ;
#303 = CARTESIAN_POINT ( 'NONE',  ( 190.0000000000000000, 2.476104986517924766E-14, 4.683861624749757595E-30 ) ) ;
#304 = ADVANCED_FACE ( 'NONE', ( #10498 ), #8499, .T. ) ;
#305 = CARTESIAN_POINT ( 'NONE',  ( -94.58414068588150769, -8.590713000723692261, -20.73981583676798124 ) ) ;
#306 = EDGE_CURVE ( 'NONE', #14634, #3360, #8864, .T. ) ;
#307 = CARTESIAN_POINT ( 'NONE',  ( -280.0000000000000568, 40.00000000000017764, -19.99999999999959144 ) ) ;
#308 = CARTESIAN_POINT ( 'NONE',  ( 4.995406935893283773, 40.00000000000017764, -15.24977328854790848 ) ) ;
#309 = CARTESIAN_POINT ( 'NONE',  ( -655.7547062770219100, 39.08587256449166603, 8.516853268417087008 ) ) ;
#310 = DIRECTION ( 'NONE',  ( 0.000000000000000000, -0.6739498806388346530, -0.7387770694782699321 ) ) ;
#311 = CARTESIAN_POINT ( 'NONE',  ( 199.0082178062215803, 19.99654772287713911, -0.6402344634765599896 ) ) ;
#312 = CARTESIAN_POINT ( 'NONE',  ( -188.2652133075334291, 23.44262061655307505, 42.99509596150254964 ) ) ;
#313 = CARTESIAN_POINT ( 'NONE',  ( 163.1118516004056573, -9.006482792074626431, 47.56205970284951690 ) ) ;
#314 = CIRCLE ( 'NONE', #24034, 5.000000000000011546 ) ;
#315 = CARTESIAN_POINT ( 'NONE',  ( -199.9999999999998579, 24.82633483071252201, 44.86878812508700776 ) ) ;
#316 = CARTESIAN_POINT ( 'NONE',  ( 19.06497207195980792, 18.24870850772737185, 38.31983398719634692 ) ) ;
#317 = DIRECTION ( 'NONE',  ( 1.000000000000000000, -1.836970198721030181E-16, -0.000000000000000000 ) ) ;
#318 = CARTESIAN_POINT ( 'NONE',  ( -86.96347745069643054, 15.38646221621821297, -41.18208027870583265 ) ) ;
#319 = CARTESIAN_POINT ( 'NONE',  ( -661.6513161486427634, 44.74118846189777088, 4.856359999860261567 ) ) ;
#320 = CARTESIAN_POINT ( 'NONE',  ( 57.59792236341147031, 2.435789363418170872, 40.00000000000002132 ) ) ;
#321 = CARTESIAN_POINT ( 'NONE',  ( 151.7948205124836250, 23.49921654116361225, -23.49921654116333514 ) ) ;
#322 = CIRCLE ( 'NONE', #24542, 5.000000000000004441 ) ;
#323 = CARTESIAN_POINT ( 'NONE',  ( 163.1118516004056573, 27.26290988616876021, 40.00000000000002132 ) ) ;
#324 = DIRECTION ( 'NONE',  ( 1.000000000000000000, 1.836970198721030181E-16, 0.000000000000000000 ) ) ;
#325 = CARTESIAN_POINT ( 'NONE',  ( -86.96347745069645896, 39.99999999999977973, 21.75974354311691883 ) ) ;
#326 = CARTESIAN_POINT ( 'NONE',  ( 19.06497207195980792, 10.03556273973433299, 10.03556273973436319 ) ) ;
#327 = CARTESIAN_POINT ( 'NONE',  ( 146.5090579137181237, -12.40347562390472191, 29.94463907179402185 ) ) ;
#328 = EDGE_LOOP ( 'NONE', ( #16904, #25782, #2991, #623 ) ) ;
#329 = ORIENTED_EDGE ( 'NONE', *, *, #13669, .T. ) ;
#330 = CARTESIAN_POINT ( 'NONE',  ( 136.1360204305621551, -35.03383547441293899, 40.00000000000002132 ) ) ;
#331 = SURFACE_SIDE_STYLE ('',( #4065 ) ) ;
#332 = CARTESIAN_POINT ( 'NONE',  ( -105.3755690713226585, 41.18208027870575449, 15.38646221621837107 ) ) ;
#333 = CARTESIAN_POINT ( 'NONE',  ( 83.01683444495014896, 24.01517293246239859, -9.947410331382577908 ) ) ;
#334 = B_SPLINE_CURVE_WITH_KNOTS ( 'NONE', 3,
 ( #4512, #20114, #6492, #14604, #8355, #6621, #19974, #12614, #1625, #16476, #1755, #1891, #10626, #24601 ),
 .UNSPECIFIED., .F., .F.,
 ( 4, 2, 2, 2, 2, 2, 4 ),
 ( 0.0003132551814620533593, 0.004485169056169878432, 0.006571125993523792459, 0.008657082930877708221, 0.01282899680558553628, 0.01491495374293945290, 0.01700091068029336780 ),
 .UNSPECIFIED. ) ;
#335 = CARTESIAN_POINT ( 'NONE',  ( -175.9234121933940003, -12.95566993500714581, -42.70618342224702957 ) ) ;
#336 = CARTESIAN_POINT ( 'NONE',  ( -175.9235632145383477, 21.03681926525754164, 39.35891845724489002 ) ) ;
#337 = CARTESIAN_POINT ( 'NONE',  ( 199.9999999999997442, 8.817246258963736594, -16.83121203733840332 ) ) ;
#338 = CARTESIAN_POINT ( 'NONE',  ( 200.0000000000000284, -8.412522034014145333, -17.05141207210294851 ) ) ;
#339 = CARTESIAN_POINT ( 'NONE',  ( -192.9588430854690273, 10.23066800229588758, -66.79921049721882298 ) ) ;
#340 = CARTESIAN_POINT ( 'NONE',  ( 57.59792236341147031, -26.56190807104712448, 30.00663442387673285 ) ) ;
#341 = CARTESIAN_POINT ( 'NONE',  ( 180.0000000000000000, -61.50000000000001421, 66.50000000000005684 ) ) ;
#342 = CARTESIAN_POINT ( 'NONE',  ( -213.1075012329537230, 40.00000000000055422, -53.71589010953623244 ) ) ;
#343 = CARTESIAN_POINT ( 'NONE',  ( 130.8568914410475088, -32.49135343045495006, 24.07718906446878648 ) ) ;
#344 = CARTESIAN_POINT ( 'NONE',  ( 130.8568914410475372, 34.05028731879791337, 0.000000000000000000 ) ) ;
#345 = CARTESIAN_POINT ( 'NONE',  ( -77.90255099907052738, 8.064892378688679031, 20.29001641119211641 ) ) ;
#346 = CARTESIAN_POINT ( 'NONE',  ( -198.0356074513804572, -67.44298959250878056, 10.87444709758448447 ) ) ;
#347 = CARTESIAN_POINT ( 'NONE',  ( -198.0356074513804572, -15.37879056873074290, 0.000000000000000000 ) ) ;
#348 = EDGE_CURVE ( 'NONE', #21839, #25714, #6340, .T. ) ;
#350 = CARTESIAN_POINT ( 'NONE',  ( -259.2033419157646676, 39.99999999999987210, 30.48217210827754542 ) ) ;
#349 = CARTESIAN_POINT ( 'NONE',  ( 184.8905102610680444, 41.77492675555983936, 14.79361573936436081 ) ) ;
#351 = CARTESIAN_POINT ( 'NONE',  ( 0.2972598230769886718, 38.42060263243643448, 18.14793986248763957 ) ) ;
#352 = CARTESIAN_POINT ( 'NONE',  ( 27.00968939604439711, 41.97305875715863976, -17.38581019152421447 ) ) ;
#353 = CARTESIAN_POINT ( 'NONE',  ( 146.6084372240433709, 5.374981219217002781, -40.00000000000002132 ) ) ;
#354 = CARTESIAN_POINT ( 'NONE',  ( -162.0762913951020892, 1.198031840385716418, 1.198031840385750169 ) ) ;
#355 = CARTESIAN_POINT ( 'NONE',  ( -100.7734535825088358, -22.67402823373193499, 0.000000000000000000 ) ) ;
#356 = ADVANCED_FACE ( 'NONE', ( #16743 ), #4299, .T. ) ;
#357 = CARTESIAN_POINT ( 'NONE',  ( -77.90255099906768521, -20.04994828523980743, 8.644468104261049390 ) ) ;
#358 = CARTESIAN_POINT ( 'NONE',  ( -30.26275506840324070, 41.69427246844628598, 2.449293598294708485E-15 ) ) ;
#359 = ADVANCED_FACE ( 'NONE', ( #19844 ), #15148, .T. ) ;
#360 = ORIENTED_EDGE ( 'NONE', *, *, #13600, .F. ) ;
#361 = DIRECTION ( 'NONE',  ( 0.000000000000000000, 0.000000000000000000, 1.000000000000000000 ) ) ;
#362 = CARTESIAN_POINT ( 'NONE',  ( -77.80451652700847376, 19.69389078277757577, 9.718324738897942794 ) ) ;
#363 = CARTESIAN_POINT ( 'NONE',  ( -4.660840668353244176, -23.32816686155642572, 42.82207049670917343 ) ) ;
#364 = CARTESIAN_POINT ( 'NONE',  ( -3.786831587087438500, 23.50387725152274143, -43.07879808621805040 ) ) ;
#365 = CARTESIAN_POINT ( 'NONE',  ( 199.0262399469797572, -16.26902294624164469, 11.64593733880351500 ) ) ;
#366 = CARTESIAN_POINT ( 'NONE',  ( -188.2995950289364089, 46.99046209955525200, -13.82811170417133617 ) ) ;
#367 = CARTESIAN_POINT ( 'NONE',  ( -53.37686176745582145, -27.95807077219591008, -13.65870576116551405 ) ) ;
#369 = CARTESIAN_POINT ( 'NONE',  ( -197.6433718613984638, -18.53520099271227650, 44.74793361791267188 ) ) ;
#368 = CIRCLE ( 'NONE', #25453, 69.99999999999994316 ) ;
#370 = CARTESIAN_POINT ( 'NONE',  ( 0.2972598230769990524, -18.14793986248671231, -38.42060263243687501 ) ) ;
#371 = CARTESIAN_POINT ( 'NONE',  ( -105.3755690713226869, 21.75974354311648540, -0.000000000000000000 ) ) ;
#373 = CARTESIAN_POINT ( 'NONE',  ( -198.0356074513804572, 10.87444709759730088, -10.87444709759707173 ) ) ;
#372 = CARTESIAN_POINT ( 'NONE',  ( -188.3509229510973171, 17.87648076835260724, -43.15764231845668775 ) ) ;
#374 = CARTESIAN_POINT ( 'NONE',  ( 163.1118516004056573, -19.27778845538787422, 19.27778845538743724 ) ) ;
#375 = CARTESIAN_POINT ( 'NONE',  ( 146.6084372240433993, -5.374981219216945938, -2.449293598294708485E-15 ) ) ;
#376 = CARTESIAN_POINT ( 'NONE',  ( 136.1360204305621266, 4.966164525587089429, 2.449293598294708485E-15 ) ) ;
#377 = CARTESIAN_POINT ( 'NONE',  ( -91.56559293963834989, -2.543181659092656077E-13, 22.67402823373191723 ) ) ;
#378 = CARTESIAN_POINT ( 'NONE',  ( 4.995406935893290878, 39.06748935135185263, 39.06748935135198764 ) ) ;
#379 = EDGE_CURVE ( 'NONE', #9180, #11184, #24378, .T. ) ;
#380 = CARTESIAN_POINT ( 'NONE',  ( -88.38011430142853442, 20.03522014474807733, -8.298859908977320288 ) ) ;
#381 = CARTESIAN_POINT ( 'NONE',  ( -30.26275506840322649, -29.48230279907769358, -29.48230279907820162 ) ) ;
#382 = CARTESIAN_POINT ( 'NONE',  ( 151.7948205124836250, 23.49921654116361225, -23.49921654116333514 ) ) ;
#383 = ORIENTED_EDGE ( 'NONE', *, *, #7506, .F. ) ;
#384 = CARTESIAN_POINT ( 'NONE',  ( 136.1360204305621551, -53.05693388239313890, 3.511608612530593199 ) ) ;
#385 = CARTESIAN_POINT ( 'NONE',  ( -102.4294859495257981, 8.407280617713011495, 20.29697089052800862 ) ) ;
#386 = CARTESIAN_POINT ( 'NONE',  ( 19.06497207195981858, -10.03556273973469715, 66.60410523465813526 ) ) ;
#387 = CARTESIAN_POINT ( 'NONE',  ( 6.984886629841083661, -44.84679502273381502, -24.81009932001601825 ) ) ;
#388 = EDGE_CURVE ( 'NONE', #22654, #12121, #26200, .T. ) ;
#389 = EDGE_CURVE ( 'NONE', #22079, #14258, #2389, .T. ) ;
#390 = ORIENTED_EDGE ( 'NONE', *, *, #13074, .F. ) ;
#391 = CARTESIAN_POINT ( 'NONE',  ( 0.4226707250630000745, -48.37218667320258447, -14.03458789212649016 ) ) ;
#392 = CYLINDRICAL_SURFACE ( 'NONE', #8339, 5.000000000000007994 ) ;
#393 = VECTOR ( 'NONE', #2972, 1000.000000000000000 ) ;
#394 = ORIENTED_EDGE ( 'NONE', *, *, #6967, .F. ) ;
#395 = B_SPLINE_CURVE_WITH_KNOTS ( 'NONE', 3,
 ( #13531, #13284, #23906, #9540, #17397, #9292 ),
 .UNSPECIFIED., .F., .F.,
 ( 4, 2, 4 ),
 ( 0.0003134720024621259586, 0.004478974658733396105, 0.008644477315004665818 ),
 .UNSPECIFIED. ) ;
#396 = CARTESIAN_POINT ( 'NONE',  ( 199.9999999999997726, 10.29466221862743680, -15.97248499526360987 ) ) ;
#397 = CARTESIAN_POINT ( 'NONE',  ( -114.4364955367323091, -20.29001642039124675, -8.064892380834873364 ) ) ;
#398 = AXIS2_PLACEMENT_3D ( 'NONE', #8466, #22714, #5020 ) ;
#399 = CARTESIAN_POINT ( 'NONE',  ( -189.1288815661592650, -43.24061771116329567, -23.62384257861769754 ) ) ;
#400 = CARTESIAN_POINT ( 'NONE',  ( -192.9588430854689989, -2.280704836619014309E-13, 54.46834944099972375 ) ) ;
#401 = B_SPLINE_CURVE_WITH_KNOTS ( 'NONE', 3,
 ( #4947, #19166, #10663, #18773, #12921, #12650, #4553, #6791, #22903, #10796, #25038, #22772 ),
 .UNSPECIFIED., .F., .F.,
 ( 4, 2, 2, 2, 2, 4 ),
 ( 5.605063087764202676E-17, 0.005971652981263785541, 0.008957479471895606754, 0.01045039271721155509, 0.01119684933986949023, 0.01194330596252742363 ),
 .UNSPECIFIED. ) ;
#402 = CARTESIAN_POINT ( 'NONE',  ( -238.4067589809705794, 40.96449427998256709, 2.449293598294708485E-15 ) ) ;
#403 = CARTESIAN_POINT ( 'NONE',  ( 136.1360204305621551, -53.05693388239309627, -3.511608612531332163 ) ) ;
#404 = DIRECTION ( 'NONE',  ( 0.000000000000000000, 1.000000000000000000, 0.000000000000000000 ) ) ;
#405 = CARTESIAN_POINT ( 'NONE',  ( -105.3755690713226585, -40.00000000000010658, 18.24025645688337249 ) ) ;
#406 = CARTESIAN_POINT ( 'NONE',  ( 19.06497207195979726, 39.99999999999997158, 14.19242893257854554 ) ) ;
#407 = DIRECTION ( 'NONE',  ( 0.000000000000000000, 0.000000000000000000, 1.000000000000000000 ) ) ;
#408 = LINE ( 'NONE', #4009, #2409 ) ;
#409 = CARTESIAN_POINT ( 'NONE',  ( -100.7734535825088500, -17.32597176626812185, -40.00000000000002132 ) ) ;
#410 = CARTESIAN_POINT ( 'NONE',  ( 184.8905102610680444, -13.49065550809810965, 13.49065550809799596 ) ) ;
#411 = CARTESIAN_POINT ( 'NONE',  ( 19.06497207195981147, 1.521599808664285085E-13, -14.19242893257840521 ) ) ;
#412 = CARTESIAN_POINT ( 'NONE',  ( -114.4364955367327070, -8.644468109209471507, 20.04994829327649342 ) ) ;
#413 = CARTESIAN_POINT ( 'NONE',  ( 170.2234770963711128, 40.00000000000021316, -15.44714144992773797 ) ) ;
#414 = CARTESIAN_POINT ( 'NONE',  ( -162.0762913951020892, 39.99999999999985079, 41.69427287692695216 ) ) ;
#415 = FACE_OUTER_BOUND ( 'NONE', #9966, .T. ) ;
#416 = CARTESIAN_POINT ( 'NONE',  ( -114.7826396787322665, 2.171560191748074081E-13, -22.13135001986799111 ) ) ;
#417 = CARTESIAN_POINT ( 'NONE',  ( -93.02511667906946968, -8.946512270084925333, -20.50052124204830761 ) ) ;
#418 = CARTESIAN_POINT ( 'NONE',  ( 146.6084372240433709, -32.08495691632041513, -24.48358557860343154 ) ) ;
#419 = ORIENTED_EDGE ( 'NONE', *, *, #4206, .T. ) ;
#420 = CARTESIAN_POINT ( 'NONE',  ( -726.9846540392142060, -66.50000000000001421, -66.50000000000005684 ) ) ;
#421 = CARTESIAN_POINT ( 'NONE',  ( -370.0000000000001137, -4.857225732735059864E-14, 0.000000000000000000 ) ) ;
#422 = CARTESIAN_POINT ( 'NONE',  ( -162.0762913951020607, -41.69427287682838568, -2.449293598294708485E-15 ) ) ;
#423 = AXIS2_PLACEMENT_3D ( 'NONE', #16508, #2685, #22769 ) ;
#424 = CARTESIAN_POINT ( 'NONE',  ( -138.9613198122422375, -27.95779845120239671, 13.65853124629192017 ) ) ;
#425 = FACE_OUTER_BOUND ( 'NONE', #10801, .T. ) ;
#426 =( NAMED_UNIT ( * ) SI_UNIT ( $, .STERADIAN. ) SOLID_ANGLE_UNIT ( ) );
#427 = ORIENTED_EDGE ( 'NONE', *, *, #15865, .F. ) ;
#428 = EDGE_LOOP ( 'NONE', ( #390, #21002 ) ) ;
#429 = SPHERICAL_SURFACE ( 'NONE', #21501, 15.00000000000000000 ) ;
#430 = CARTESIAN_POINT ( 'NONE',  ( -97.73806390048314086, 8.581719943918708182, -20.71810467719452120 ) ) ;
#431 = CARTESIAN_POINT ( 'NONE',  ( 19.94008347562546390, 13.96811062196290010, 47.92933869853475670 ) ) ;
#432 = EDGE_LOOP ( 'NONE', ( #11863, #1832, #6303, #14953 ) ) ;
#433 = VERTEX_POINT ( 'NONE', #24106 ) ;
#434 = CARTESIAN_POINT ( 'NONE',  ( -135.8532207217289738, -6.472252184284287502, 50.09629031063965243 ) ) ;
#435 = CARTESIAN_POINT ( 'NONE',  ( 199.0205186365099905, -18.88915341724846542, -6.581556047429298673 ) ) ;
#436 = CARTESIAN_POINT ( 'NONE',  ( -110.0947178155009141, 2.529241932053376551, 20.04333087343293940 ) ) ;
#437 = CARTESIAN_POINT ( 'NONE',  ( -109.1264249741459338, -33.12752917269534692, -13.72187187123280161 ) ) ;
#438 = CARTESIAN_POINT ( 'NONE',  ( 91.82158438592158234, -12.16597498397761967, -12.16597498397768007 ) ) ;
#439 = CIRCLE ( 'NONE', #14817, 44.99999999999997158 ) ;
#440 = CARTESIAN_POINT ( 'NONE',  ( -295.0000000000000568, -4.857225732735059864E-14, 0.000000000000000000 ) ) ;
#441 = FACE_BOUND ( 'NONE', #16176, .T. ) ;
#442=STYLED_ITEM('',(#26409),#26080);
#443 = CARTESIAN_POINT ( 'NONE',  ( 200.0000000000000000, 40.00000000000026290, -19.99999999999950617 ) ) ;
#444 = CARTESIAN_POINT ( 'NONE',  ( 163.1118516004056573, -2.556006622855449647E-13, 27.26290988616872824 ) ) ;
#445 = CARTESIAN_POINT ( 'NONE',  ( -650.6286843459992042, 35.47998694306583189, 18.48952057123083037 ) ) ;
#446 = DIRECTION ( 'NONE',  ( 0.000000000000000000, 0.000000000000000000, -1.000000000000000000 ) ) ;
#447 = CARTESIAN_POINT ( 'NONE',  ( 199.0122446118616892, 18.20979473430505280, 8.267810710173087330 ) ) ;
#448 = CARTESIAN_POINT ( 'NONE',  ( -188.3610564113327825, 23.46269903113395827, 43.02325945309083011 ) ) ;
#449 = CARTESIAN_POINT ( 'NONE',  ( -105.3755690713226585, -12.89780903124444578, 43.67073346367968156 ) ) ;
#450 =( BOUNDED_CURVE ( )  B_SPLINE_CURVE ( 3, ( #3461, #19679, #15943, #11828 ),
 .UNSPECIFIED., .F., .F. ) 
 B_SPLINE_CURVE_WITH_KNOTS ( ( 4, 4 ),
 ( 0.004183487405659383311, 0.01388163287021833628 ),
 .UNSPECIFIED. ) 
 CURVE ( )  GEOMETRIC_REPRESENTATION_ITEM ( )  RATIONAL_B_SPLINE_CURVE ( ( 0.6809743333591558034, 0.7608653435686151267, 0.8672072324488965256, 1.000000000000000000 ) ) 
 REPRESENTATION_ITEM ( '' )  );
#451 = DIRECTION ( 'NONE',  ( 0.000000000000000000, 0.000000000000000000, -1.000000000000000000 ) ) ;
#452 = CARTESIAN_POINT ( 'NONE',  ( 14.38125909742182529, -39.01709431150933938, 39.01709431150894147 ) ) ;
#453 = CARTESIAN_POINT ( 'NONE',  ( 150.0000000000000284, -135.7889608577475258, -82.49999999999998579 ) ) ;
#454 = CARTESIAN_POINT ( 'NONE',  ( 192.4448373802101173, 14.14213562375922884, -42.42640687116488607 ) ) ;
#455 = CARTESIAN_POINT ( 'NONE',  ( -649.9764076924376468, 36.43131350046466821, 26.47907437413556053 ) ) ;
#456 = CARTESIAN_POINT ( 'NONE',  ( 163.1118516004056573, 27.26290988616875310, 0.000000000000000000 ) ) ;
#457 = CARTESIAN_POINT ( 'NONE',  ( -192.9588430854690273, 66.79921049724377724, -10.23066800231904239 ) ) ;
#458 = CARTESIAN_POINT ( 'NONE',  ( -100.7734535825088500, 22.67402823373189591, -0.000000000000000000 ) ) ;
#459 = LINE ( 'NONE', #6827, #7636 ) ;
#460 = CARTESIAN_POINT ( 'NONE',  ( -91.56559293963834989, -39.99999999999985789, -17.32597176626853042 ) ) ;
#461 = CARTESIAN_POINT ( 'NONE',  ( 199.0150639398586634, -12.88796719789325707, -15.29887847299889003 ) ) ;
#462 = DIRECTION ( 'NONE',  ( -1.000000000000000000, 0.000000000000000000, 0.000000000000000000 ) ) ;
#463 = ORIENTED_EDGE ( 'NONE', *, *, #25346, .F. ) ;
#464 = AXIS2_PLACEMENT_3D ( 'NONE', #3688, #20320, #23901 ) ;
#466 = ORIENTED_EDGE ( 'NONE', *, *, #16953, .T. ) ;
#465 = EDGE_CURVE ( 'NONE', #21399, #16736, #13986, .T. ) ;
#467 = CARTESIAN_POINT ( 'NONE',  ( -86.96347745069644475, -21.75974354311651737, 0.000000000000000000 ) ) ;
#468 = DIRECTION ( 'NONE',  ( 0.000000000000000000, 0.000000000000000000, 1.000000000000000000 ) ) ;
#469 = CARTESIAN_POINT ( 'NONE',  ( 0.2972598230769907257, 66.70487387989869887, -10.13633138497392494 ) ) ;
#470 = CARTESIAN_POINT ( 'NONE',  ( -114.4364955367305896, -20.29001642037712827, 8.064892380866057309 ) ) ;
#471 = CARTESIAN_POINT ( 'NONE',  ( -215.0000000000000284, 69.29737539576900929, -75.30386416458597409 ) ) ;
#472 = DIRECTION ( 'NONE',  ( 0.000000000000000000, 0.000000000000000000, 1.000000000000000000 ) ) ;
#473 = CARTESIAN_POINT ( 'NONE',  ( 199.9999999999999147, 7.974356211459238786, -17.24664066343551028 ) ) ;
#474 = CARTESIAN_POINT ( 'NONE',  ( 170.0000000000000000, -6.285860131565354614, 24.25569233607177111 ) ) ;
#475 = CIRCLE ( 'NONE', #21717, 14.99999999999999822 ) ;
#476 = CARTESIAN_POINT ( 'NONE',  ( 136.1360204305621551, -53.05693388239309627, -3.511608612531332163 ) ) ;
#477 = CARTESIAN_POINT ( 'NONE',  ( -56.48582580120559271, 6.472252184284121412, 6.472252184284244869 ) ) ;
#478 = DIRECTION ( 'NONE',  ( 0.000000000000000000, 0.000000000000000000, -1.000000000000000000 ) ) ;
#479 = CARTESIAN_POINT ( 'NONE',  ( 151.7948205124836534, 40.00000000000012079, -6.767089262348609857 ) ) ;
#480 = CARTESIAN_POINT ( 'NONE',  ( 184.8905102610680444, -13.49065550809840630, 43.07788698682565354 ) ) ;
#481 = CARTESIAN_POINT ( 'NONE',  ( -83.21262154144251610, -13.72187187061536484, 33.12752917118401541 ) ) ;
#482 = CARTESIAN_POINT ( 'NONE',  ( -30.26275506840324070, 1.198031551616013601, 1.198031551616023371 ) ) ;
#483 = CARTESIAN_POINT ( 'NONE',  ( -213.1075012329537230, -9.698598906438496314, 66.26714140136188291 ) ) ;
#484 = DIRECTION ( 'NONE',  ( -1.000000000000000000, -1.836970198721030181E-16, -0.000000000000000000 ) ) ;
#486 = CARTESIAN_POINT ( 'NONE',  ( 184.8905102610680444, -40.00000000000005684, 19.07866798485543569 ) ) ;
#485 = CARTESIAN_POINT ( 'NONE',  ( 14.38125909742181463, 10.73282306403652875, -67.30136555895941797 ) ) ;
#487 = CARTESIAN_POINT ( 'NONE',  ( 91.82158438592158234, 16.11829626348378142, 40.45024623143977749 ) ) ;
#488 = CARTESIAN_POINT ( 'NONE',  ( 23.38399212876566580, 42.85408588822684806, -23.33762193384624695 ) ) ;
#489 = CARTESIAN_POINT ( 'NONE',  ( -91.56559293963834989, 17.32597176626809699, -40.00000000000002132 ) ) ;
#490 = CARTESIAN_POINT ( 'NONE',  ( -280.0000000000000568, -42.42640687119295251, 14.14213562373088351 ) ) ;
#491 = CARTESIAN_POINT ( 'NONE',  ( -56.48582580120559982, 30.84685318188643421, 40.00000000000002132 ) ) ;
#492 = CARTESIAN_POINT ( 'NONE',  ( -5.787027468455986146, -42.67020100828555940, 17.67457596681778043 ) ) ;
#493 = AXIS2_PLACEMENT_3D ( 'NONE', #19176, #9563, #1212 ) ;
#494 = CARTESIAN_POINT ( 'NONE',  ( -238.4067589809705794, 40.96449427990177128, 40.00000000000002132 ) ) ;
#495 = VERTEX_POINT ( 'NONE', #11725 ) ;
#496 = CARTESIAN_POINT ( 'NONE',  ( -198.0012279766650067, -49.19397028317939657, -14.15883993157146215 ) ) ;
#497 = AXIS2_PLACEMENT_3D ( 'NONE', #8550, #23068, #15061 ) ;
#498 = CARTESIAN_POINT ( 'NONE',  ( -77.55640685876515761, 16.67541351910017866, 14.62304181636398148 ) ) ;
#499 = CARTESIAN_POINT ( 'NONE',  ( -4.076660308449182146, -23.44206949513782945, 42.99426297939349695 ) ) ;
#500 = CARTESIAN_POINT ( 'NONE',  ( -4.660840668352557614, 13.78427145221092154, -46.77528141313259624 ) ) ;
#501 = CARTESIAN_POINT ( 'NONE',  ( 200.0000000000000853, -10.31015863810315025, 15.97237410830284254 ) ) ;
#502 = CARTESIAN_POINT ( 'NONE',  ( -238.4067589809705794, 28.96627169325285678, 27.60227080167094726 ) ) ;
#503 = CARTESIAN_POINT ( 'NONE',  ( -82.30220482034343377, -18.74474319042090542, 7.441767004327110691 ) ) ;
#504 = CARTESIAN_POINT ( 'NONE',  ( -726.9846540392142060, 52.49999999999986500, 82.49999999999998579 ) ) ;
#505 = CARTESIAN_POINT ( 'NONE',  ( -188.4702232936788278, -23.48628015402999836, 43.05505437950382941 ) ) ;
#506 = CARTESIAN_POINT ( 'NONE',  ( 192.4448373802100889, 14.14213562375873678, 14.14213562375894817 ) ) ;
#507 = CARTESIAN_POINT ( 'NONE',  ( -100.7734535825088500, -44.31723036834885932, -12.25131212657538171 ) ) ;
#508 = CARTESIAN_POINT ( 'NONE',  ( -198.0356074513804572, -10.87444709759714634, -10.87444709759729911 ) ) ;
#509 = VECTOR ( 'NONE', #21184, 1000.000000000000000 ) ;
#511 = CARTESIAN_POINT ( 'NONE',  ( 4.995406935893290878, 39.06748935135239265, -39.06748935135144762 ) ) ;
#510 = CARTESIAN_POINT ( 'NONE',  ( 19.06497207195981147, -10.03556273973425483, -10.03556273973443247 ) ) ;
#512 = CARTESIAN_POINT ( 'NONE',  ( -86.96347745069644475, 12.89780903124349898, 43.67073346367994446 ) ) ;
#513 = CARTESIAN_POINT ( 'NONE',  ( -100.7734535825088358, -17.32597176626813251, -2.449293598294708485E-15 ) ) ;
#514 = CARTESIAN_POINT ( 'NONE',  ( 91.82158438592158234, 22.79471317813471742, 40.00000000000002132 ) ) ;
#515 = CARTESIAN_POINT ( 'NONE',  ( -56.48582580120558561, -40.00000000000012790, 9.153146818113166105 ) ) ;
#516 = CARTESIAN_POINT ( 'NONE',  ( -91.56559293963834989, 12.25131212657490209, -44.31723036834897300 ) ) ;
#517 = DIRECTION ( 'NONE',  ( 0.000000000000000000, 0.000000000000000000, 1.000000000000000000 ) ) ;
#518 = CARTESIAN_POINT ( 'NONE',  ( 14.38125909742181996, -10.73282306405815234, -67.30136555898266693 ) ) ;
#519 = CARTESIAN_POINT ( 'NONE',  ( -56.48582580120559271, 6.472252184284211118, -6.472252184284153387 ) ) ;
#520 = ORIENTED_EDGE ( 'NONE', *, *, #25095, .F. ) ;
#521 = CARTESIAN_POINT ( 'NONE',  ( 192.4448373802101173, -14.14213562375886291, 42.42640687116498555 ) ) ;
#522 = CARTESIAN_POINT ( 'NONE',  ( 169.9999999999999432, 22.62041470344884075, 9.369682556672378482 ) ) ;
#523 = CARTESIAN_POINT ( 'NONE',  ( -100.7734535825088500, 16.03295912088683295, 40.53558337403684675 ) ) ;
#524 = CARTESIAN_POINT ( 'NONE',  ( 7.112934525950139530, -44.84100494512853885, -18.57375239871706185 ) ) ;
#525 = VERTEX_POINT ( 'NONE', #9736 ) ;
#526 = DIRECTION ( 'NONE',  ( 0.000000000000000000, 0.000000000000000000, 1.000000000000000000 ) ) ;
#527 = CARTESIAN_POINT ( 'NONE',  ( -90.07798792367799479, -15.74993999324178162, -15.74993999324182248 ) ) ;
#528 = ORIENTED_EDGE ( 'NONE', *, *, #7839, .T. ) ;
#529 = CARTESIAN_POINT ( 'NONE',  ( 199.9999999999997442, 17.78964944107278967, -6.681507572083275726 ) ) ;
#530 = CIRCLE ( 'NONE', #25177, 14.99999999999999822 ) ;
#531 = DIRECTION ( 'NONE',  ( 1.000000000000000000, 1.836970198721030181E-16, -0.000000000000000000 ) ) ;
#532 = EDGE_CURVE ( 'NONE', #15801, #13855, #7476, .T. ) ;
#533 = CARTESIAN_POINT ( 'NONE',  ( 192.4448373802101173, 19.99999999996063949, 40.00000000000002132 ) ) ;
#534 = CARTESIAN_POINT ( 'NONE',  ( -162.0762913951021176, -27.08623940707584055, -29.48230308784799547 ) ) ;
#535 = CARTESIAN_POINT ( 'NONE',  ( 199.0191753821509622, 9.128090787448098098, 17.79799345705162139 ) ) ;
#536 = EDGE_CURVE ( 'NONE', #22653, #12962, #21308, .T. ) ;
#537 = CARTESIAN_POINT ( 'NONE',  ( -162.0762913951020607, -57.76657433537922515, -1.198031840455874963 ) ) ;
#538 = CARTESIAN_POINT ( 'NONE',  ( 184.8905102610680444, -40.00000000000005684, 19.07866798485543569 ) ) ;
#539 = CARTESIAN_POINT ( 'NONE',  ( 0.2972598230769883387, 39.99999999999997158, 14.33493731733947563 ) ) ;
#540 = CARTESIAN_POINT ( 'NONE',  ( -215.0000000000000284, 61.50000000000001421, -66.50000000000005684 ) ) ;
#541 = CARTESIAN_POINT ( 'NONE',  ( 14.38125909742181285, -15.17850393972633505, 0.000000000000000000 ) ) ;
#542 = CARTESIAN_POINT ( 'NONE',  ( -597.4202930725263059, 39.67406997103029198, 5.193980993137010671 ) ) ;
#543 = EDGE_CURVE ( 'NONE', #14909, #16811, #17780, .T. ) ;
#544 = CARTESIAN_POINT ( 'NONE',  ( -100.7734535825088358, -17.32597176626813251, -2.449293598294708485E-15 ) ) ;
#545 = EDGE_CURVE ( 'NONE', #9566, #22711, #18550, .T. ) ;
#546 = CARTESIAN_POINT ( 'NONE',  ( -208.1127848780264742, -38.89260858015758515, 38.89260858015713751 ) ) ;
#547 = CARTESIAN_POINT ( 'NONE',  ( -114.4364955367327354, 8.064892380842190178, 20.29001642038852182 ) ) ;
#548 = CARTESIAN_POINT ( 'NONE',  ( -105.2109270643250909, 16.13380223203129304, -14.21138704485549731 ) ) ;
#549 = CARTESIAN_POINT ( 'NONE',  ( -56.48582580120558561, 3.151766524733697544E-13, -30.84685318188644132 ) ) ;
#550 = CARTESIAN_POINT ( 'NONE',  ( 192.4448373802100889, -3.692737725850373501E-14, 19.99999999996060751 ) ) ;
#551 = CARTESIAN_POINT ( 'NONE',  ( 200.0000000000000000, 14.14213562373100608, -42.42640687119291698 ) ) ;
#552 = CARTESIAN_POINT ( 'NONE',  ( -362.0709805440841365, 9.999999999999960920, 0.000000000000000000 ) ) ;
#553 = CARTESIAN_POINT ( 'NONE',  ( -210.0000000000000284, 72.72568232011437317, -59.67546976104961942 ) ) ;
#554 = CARTESIAN_POINT ( 'NONE',  ( 91.82158438592156813, -16.11829626348402655, -40.45024623143966380 ) ) ;
#555 = VERTEX_POINT ( 'NONE', #21999 ) ;
#556 = DIRECTION ( 'NONE',  ( -1.000000000000000000, -1.836970198721030427E-16, 0.000000000000000000 ) ) ;
#557 = DIRECTION ( 'NONE',  ( 0.000000000000000000, 0.000000000000000000, 1.000000000000000000 ) ) ;
#558 = CARTESIAN_POINT ( 'NONE',  ( 136.1360204305621551, -4.966164525587036138, -40.00000000000002132 ) ) ;
#559 = CARTESIAN_POINT ( 'NONE',  ( -87.11144460191506766, -21.34775735502242000, -2.726834743463422583 ) ) ;
#560 = CARTESIAN_POINT ( 'NONE',  ( -192.9588430854689989, 10.23066800230756712, -10.23066800230735396 ) ) ;
#561 = ORIENTED_EDGE ( 'NONE', *, *, #7645, .F. ) ;
#562 =( BOUNDED_SURFACE ( )  B_SPLINE_SURFACE ( 3, 3, ( 
 ( #2606, #10719, #25098, #14964, #10577, #12567, #4870, #12974, #18828, #18692, #24826, #608, #21097, #477, #6579, #2877, #10985, #19095, #25223, #21357, #5129, #15468, #11229, #7110, #25867, #3126, #9623, #19347, #17216, #13603 ),
 ( #19602, #9489, #1388, #7611, #11353, #15726, #21861, #23597, #25355, #13235, #11607, #5376, #7356, #11742, #23851, #17347, #19730, #17470, #25612, #9360, #23476, #13480, #9106, #21602, #9240, #3375, #1256, #11474, #17593, #3637 ),
 ( #15221, #21732, #1136, #23352, #25733, #5248, #3508, #7484, #15596, #19862, #5502, #23721, #1517, #17726, #5629, #25483, #13735, #7232, #15352, #13352, #21474, #3249, #19469, #20137, #9888, #2051, #13871, #14143, #16407, #3918 ),
 ( #6164, #5899, #24128, #42, #8018, #22275, #18261, #16001, #10290, #7880, #1915, #5763, #6291, #12409, #4049, #17856, #6037, #12150, #12281, #175, #22004, #24535, #4319, #20272, #8155, #26137, #14008, #26279, #10158, #3775 ),
 ( #1784, #16269, #14409, #24398, #17990, #22410, #14274, #11878, #10020, #26007, #4186, #19998, #16133, #20408, #12017, #2182, #22539, #23984, #1647, #18398, #24264, #15855, #8281, #9755, #18129, #7743, #22137, #4712, #19064, #22802 ),
 ( #25199, #12816, #18663, #6422, #10822, #2305, #20806, #23194, #24800, #449, #10414, #8956, #16799, #14800, #8821, #20939, #8553, #4579, #2717, #24936, #2577, #18935, #847, #18532, #17065, #313, #25067, #24665, #8415, #717 ),
 ( #18803, #16932, #6946, #6818, #6686, #22932, #12948, #23071, #10551, #14935, #2439, #583, #15064, #16537, #14540, #22670, #12676, #16669, #4842, #4442, #21064, #4975, #10691, #20534, #6552, #12536, #2850, #14662, #20670, #10958 ) ),
 .UNSPECIFIED., .T., .F., .F. ) 
 B_SPLINE_SURFACE_WITH_KNOTS ( ( 4, 3, 4 ),
 ( 4, 2, 2, 2, 2, 2, 2, 2, 2, 2, 2, 2, 2, 2, 4 ),
 ( 0.000000000000000000, 0.5000000000000000000, 1.000000000000000000 ),
 ( 0.000000000000000000, 0.1357259735107005372, 0.1651108541090157700, 0.1944957347073310028, 0.3598804999793158710, 0.3867117631979620773, 0.4135430264166082281, 0.5789277916885930964, 0.6062785021374117456, 0.6336292125862302838, 0.8508620842112317728, 0.8814014469398914198, 0.9119408096685510667, 0.9559704048342755334, 1.000000000000000000 ),
 .UNSPECIFIED. ) 
 GEOMETRIC_REPRESENTATION_ITEM ( )  RATIONAL_B_SPLINE_SURFACE ( (
 ( 1.000000000000000000, 1.000000000000000000, 1.000000000000000000, 1.000000000000000000, 1.000000000000000000, 1.000000000000000000, 1.000000000000000000, 1.000000000000000000, 1.000000000000000000, 1.000000000000000000, 1.000000000000000000, 1.000000000000000000, 1.000000000000000000, 1.000000000000000000, 1.000000000000000000, 1.000000000000000000, 1.000000000000000000, 1.000000000000000000, 1.000000000000000000, 1.000000000000000000, 1.000000000000000000, 1.000000000000000000, 1.000000000000000000, 1.000000000000000000, 1.000000000000000000, 1.000000000000000000, 1.000000000000000000, 1.000000000000000000, 1.000000000000000000, 1.000000000000000000),
 ( 0.3333333333333333703, 0.3333333333333333703, 0.3333333333333333703, 0.3333333333333333703, 0.3333333333333333703, 0.3333333333333333703, 0.3333333333333333703, 0.3333333333333333703, 0.3333333333333333703, 0.3333333333333333703, 0.3333333333333333703, 0.3333333333333333703, 0.3333333333333333703, 0.3333333333333333703, 0.3333333333333333703, 0.3333333333333333703, 0.3333333333333333703, 0.3333333333333333703, 0.3333333333333333703, 0.3333333333333333703, 0.3333333333333333703, 0.3333333333333333703, 0.3333333333333333703, 0.3333333333333333703, 0.3333333333333333703, 0.3333333333333333703, 0.3333333333333333703, 0.3333333333333333703, 0.3333333333333333703, 0.3333333333333333703),
 ( 0.3333333333333333703, 0.3333333333333333703, 0.3333333333333333703, 0.3333333333333333703, 0.3333333333333333703, 0.3333333333333333703, 0.3333333333333333703, 0.3333333333333333703, 0.3333333333333333703, 0.3333333333333333703, 0.3333333333333333703, 0.3333333333333333703, 0.3333333333333333703, 0.3333333333333333703, 0.3333333333333333703, 0.3333333333333333703, 0.3333333333333333703, 0.3333333333333333703, 0.3333333333333333703, 0.3333333333333333703, 0.3333333333333333703, 0.3333333333333333703, 0.3333333333333333703, 0.3333333333333333703, 0.3333333333333333703, 0.3333333333333333703, 0.3333333333333333703, 0.3333333333333333703, 0.3333333333333333703, 0.3333333333333333703),
 ( 1.000000000000000000, 1.000000000000000000, 1.000000000000000000, 1.000000000000000000, 1.000000000000000000, 1.000000000000000000, 1.000000000000000000, 1.000000000000000000, 1.000000000000000000, 1.000000000000000000, 1.000000000000000000, 1.000000000000000000, 1.000000000000000000, 1.000000000000000000, 1.000000000000000000, 1.000000000000000000, 1.000000000000000000, 1.000000000000000000, 1.000000000000000000, 1.000000000000000000, 1.000000000000000000, 1.000000000000000000, 1.000000000000000000, 1.000000000000000000, 1.000000000000000000, 1.000000000000000000, 1.000000000000000000, 1.000000000000000000, 1.000000000000000000, 1.000000000000000000),
 ( 0.3333333333333333703, 0.3333333333333333703, 0.3333333333333333703, 0.3333333333333333703, 0.3333333333333333703, 0.3333333333333333703, 0.3333333333333333703, 0.3333333333333333703, 0.3333333333333333703, 0.3333333333333333703, 0.3333333333333333703, 0.3333333333333333703, 0.3333333333333333703, 0.3333333333333333703, 0.3333333333333333703, 0.3333333333333333703, 0.3333333333333333703, 0.3333333333333333703, 0.3333333333333333703, 0.3333333333333333703, 0.3333333333333333703, 0.3333333333333333703, 0.3333333333333333703, 0.3333333333333333703, 0.3333333333333333703, 0.3333333333333333703, 0.3333333333333333703, 0.3333333333333333703, 0.3333333333333333703, 0.3333333333333333703),
 ( 0.3333333333333333703, 0.3333333333333333703, 0.3333333333333333703, 0.3333333333333333703, 0.3333333333333333703, 0.3333333333333333703, 0.3333333333333333703, 0.3333333333333333703, 0.3333333333333333703, 0.3333333333333333703, 0.3333333333333333703, 0.3333333333333333703, 0.3333333333333333703, 0.3333333333333333703, 0.3333333333333333703, 0.3333333333333333703, 0.3333333333333333703, 0.3333333333333333703, 0.3333333333333333703, 0.3333333333333333703, 0.3333333333333333703, 0.3333333333333333703, 0.3333333333333333703, 0.3333333333333333703, 0.3333333333333333703, 0.3333333333333333703, 0.3333333333333333703, 0.3333333333333333703, 0.3333333333333333703, 0.3333333333333333703),
 ( 1.000000000000000000, 1.000000000000000000, 1.000000000000000000, 1.000000000000000000, 1.000000000000000000, 1.000000000000000000, 1.000000000000000000, 1.000000000000000000, 1.000000000000000000, 1.000000000000000000, 1.000000000000000000, 1.000000000000000000, 1.000000000000000000, 1.000000000000000000, 1.000000000000000000, 1.000000000000000000, 1.000000000000000000, 1.000000000000000000, 1.000000000000000000, 1.000000000000000000, 1.000000000000000000, 1.000000000000000000, 1.000000000000000000, 1.000000000000000000, 1.000000000000000000, 1.000000000000000000, 1.000000000000000000, 1.000000000000000000, 1.000000000000000000, 1.000000000000000000) ) ) 
 REPRESENTATION_ITEM ( '' )  SURFACE ( )  );
#563 = ORIENTED_EDGE ( 'NONE', *, *, #7909, .T. ) ;
#564 = CARTESIAN_POINT ( 'NONE',  ( 199.9999999999999147, -2.490047575889294595, 18.88689753006142880 ) ) ;
#565 = CARTESIAN_POINT ( 'NONE',  ( -103.9663809733945499, 8.026122151960143114, -20.15238534321454367 ) ) ;
#566 = CARTESIAN_POINT ( 'NONE',  ( 23.26364522859735828, 23.36474233297307990, 42.89098160628132916 ) ) ;
#567 = VERTEX_POINT ( 'NONE', #26132 ) ;
#568 = ORIENTED_EDGE ( 'NONE', *, *, #18157, .T. ) ;
#569 = CARTESIAN_POINT ( 'NONE',  ( 136.1360204305621551, -53.05693388239313890, 3.511608612530593199 ) ) ;
#570 = CARTESIAN_POINT ( 'NONE',  ( 199.0236444319429268, -19.98745889671670284, 0.8241971460415670192 ) ) ;
#571 = CARTESIAN_POINT ( 'NONE',  ( -110.1018001840315321, 0.6219992248577108640, 20.19553435165690658 ) ) ;
#572 = CARTESIAN_POINT ( 'NONE',  ( 192.4448373802100889, -14.14213562375876698, -14.14213562375885047 ) ) ;
#573 = DIRECTION ( 'NONE',  ( -1.000000000000000000, 0.000000000000000000, -0.000000000000000000 ) ) ;
#574 = CARTESIAN_POINT ( 'NONE',  ( -208.1127848780264742, 39.99999999999992895, 15.00245453012683683 ) ) ;
#575 = PLANE ( 'NONE',  #7887 ) ;
#576 = FACE_OUTER_BOUND ( 'NONE', #10089, .T. ) ;
#577 = CARTESIAN_POINT ( 'NONE',  ( -198.0356074513804572, 40.00000000000056843, -55.37879056871282302 ) ) ;
#578 = CARTESIAN_POINT ( 'NONE',  ( -259.2033419157646676, 39.99999999999987921, 9.517827891723049660 ) ) ;
#579 = CARTESIAN_POINT ( 'NONE',  ( -656.5498746188114865, 39.67471111131991535, -5.189028119869940170 ) ) ;
#580 = LINE ( 'NONE', #4839, #17878 ) ;
#581 = CARTESIAN_POINT ( 'NONE',  ( 199.0103760074104002, 19.48024492545154018, 4.564568505664855280 ) ) ;
#582 = CARTESIAN_POINT ( 'NONE',  ( -188.9266304146001971, 17.94050393342739014, 43.31220791188948738 ) ) ;
#583 = CARTESIAN_POINT ( 'NONE',  ( -91.56559293963836410, 16.03295912088692177, 16.03295912088721664 ) ) ;
#584 = CARTESIAN_POINT ( 'NONE',  ( -265.6482238768269326, 0.000000000000000000, 0.000000000000000000 ) ) ;
#585 = CARTESIAN_POINT ( 'NONE',  ( -56.48582580120558561, 6.472252184283903809, 50.09629031063968796 ) ) ;
#586 = DIRECTION ( 'NONE',  ( 1.000000000000000000, 1.836970198721030427E-16, 0.000000000000000000 ) ) ;
#587 = CARTESIAN_POINT ( 'NONE',  ( -105.3755690713226727, -12.89780903124395550, -12.89780903124416511 ) ) ;
#588 = CARTESIAN_POINT ( 'NONE',  ( -199.9999999999998010, 49.28189405767604114, -14.17215463606931181 ) ) ;
#589 = CARTESIAN_POINT ( 'NONE',  ( 91.82158438592158234, 17.20528682183301683, 0.000000000000000000 ) ) ;
#590 = CARTESIAN_POINT ( 'NONE',  ( 136.1360204305621266, -24.77266263493151044, 24.77266263493093135 ) ) ;
#591 = CARTESIAN_POINT ( 'NONE',  ( -259.2033419157646676, 9.517827891722584255, -0.000000000000000000 ) ) ;
#592 = CARTESIAN_POINT ( 'NONE',  ( -611.2898122108906591, 32.33625437144371517, -31.30306668446011642 ) ) ;
#593 = ORIENTED_EDGE ( 'NONE', *, *, #11245, .T. ) ;
#594 = CARTESIAN_POINT ( 'NONE',  ( -162.0762913951020892, -39.99999999999961631, -41.69427287692722928 ) ) ;
#595 = CARTESIAN_POINT ( 'NONE',  ( 199.0058896134214024, 8.852588301136247395, -17.93157114668636964 ) ) ;
#596 = CARTESIAN_POINT ( 'NONE',  ( 137.0939645874030361, -12.56330697291285681, 30.33050608226178468 ) ) ;
#597 = ORIENTED_EDGE ( 'NONE', *, *, #20606, .T. ) ;
#598 = ORIENTED_EDGE ( 'NONE', *, *, #21416, .F. ) ;
#599 = CARTESIAN_POINT ( 'NONE',  ( -280.0000000000000000, 19.99999999999996092, 2.449293598294708485E-15 ) ) ;
#600 = CARTESIAN_POINT ( 'NONE',  ( -190.0000000000000000, -66.50000000000001421, -66.50000000000005684 ) ) ;
#601 = CARTESIAN_POINT ( 'NONE',  ( -114.7824662269243561, -22.13040512707748064, -1.403530270405573210 ) ) ;
#602 = CARTESIAN_POINT ( 'NONE',  ( 107.5473083967388277, -16.96446921415041587, -16.96446921415049403 ) ) ;
#603 =( BOUNDED_CURVE ( )  B_SPLINE_CURVE ( 3, ( #11156, #15517, #13403, #11526 ),
 .UNSPECIFIED., .F., .F. ) 
 B_SPLINE_CURVE_WITH_KNOTS ( ( 4, 4 ),
 ( 0.01577215542394082640, 0.02369175774463767523 ),
 .UNSPECIFIED. ) 
 CURVE ( )  GEOMETRIC_REPRESENTATION_ITEM ( )  RATIONAL_B_SPLINE_CURVE ( ( 0.5197830649482693133, 0.5065943549827455206, 0.4999999999999891198, 0.5000000000000001110 ) ) 
 REPRESENTATION_ITEM ( '' )  );
#604 = LINE ( 'NONE', #14430, #23210 ) ;
#605 = CARTESIAN_POINT ( 'NONE',  ( 200.0000000000000000, 15.45062812681867825, -11.05917137904152625 ) ) ;
#606 = CARTESIAN_POINT ( 'NONE',  ( -105.4741150117382062, 7.943527260750565588, -19.77569912955109288 ) ) ;
#607 = CARTESIAN_POINT ( 'NONE',  ( -105.3755690713226585, -43.67073346367964604, -12.89780903124457545 ) ) ;
#608 = CARTESIAN_POINT ( 'NONE',  ( -91.56559293963836410, 16.03295912088692177, 16.03295912088721664 ) ) ;
#609 = DIRECTION ( 'NONE',  ( 0.000000000000000000, 0.000000000000000000, -1.000000000000000000 ) ) ;
#610 = CARTESIAN_POINT ( 'NONE',  ( -192.9588430854690273, 40.00000000000055422, -54.46834944101679810 ) ) ;
#611 = CARTESIAN_POINT ( 'NONE',  ( -88.39148973765144035, -8.027153355909462107, 20.15708830332390988 ) ) ;
#612 = ADVANCED_FACE ( 'NONE', ( #6031 ), #23234, .T. ) ;
#613 = CARTESIAN_POINT ( 'NONE',  ( -238.4067589809705794, -0.9644942799826262680, 0.000000000000000000 ) ) ;
#614 = CARTESIAN_POINT ( 'NONE',  ( 163.1118516004056573, -19.27778845538761132, -19.27778845538770724 ) ) ;
#615 = CARTESIAN_POINT ( 'NONE',  ( 146.6084372240433709, -32.08495691632041513, -24.48358557860343154 ) ) ;
#616 = CARTESIAN_POINT ( 'NONE',  ( 199.0138869583062728, 16.66122972709626637, 11.08110611611319740 ) ) ;
#618 = CARTESIAN_POINT ( 'NONE',  ( -208.1127848780265026, -9.061048840815752106E-14, 15.00245453012669472 ) ) ;
#617 = CARTESIAN_POINT ( 'NONE',  ( -280.0000000000000568, -42.42640687119276066, -14.14213562373147148 ) ) ;
#619 = CARTESIAN_POINT ( 'NONE',  ( 36.66494225463969059, 39.17447069122760439, -16.22659705898878002 ) ) ;
#620 = CARTESIAN_POINT ( 'NONE',  ( 91.82158438592158234, -17.20528682183298486, -40.00000000000002132 ) ) ;
#621 = CARTESIAN_POINT ( 'NONE',  ( 192.4448373802101173, -42.42640687122073473, 14.14213562370301780 ) ) ;
#622 = CARTESIAN_POINT ( 'NONE',  ( 130.8568914410475372, -34.05028731879786363, 0.000000000000000000 ) ) ;
#623 = ORIENTED_EDGE ( 'NONE', *, *, #25019, .T. ) ;
#624 = CARTESIAN_POINT ( 'NONE',  ( 6.615221834168117709, -44.82734842560460464, 24.79576599681886151 ) ) ;
#625 = CARTESIAN_POINT ( 'NONE',  ( -30.26275506840324425, 41.69427246844627177, 40.00000000000002132 ) ) ;
#626 = EDGE_CURVE ( 'NONE', #8935, #25083, #18123, .T. ) ;
#627 = ORIENTED_EDGE ( 'NONE', *, *, #1350, .F. ) ;
#628 = CARTESIAN_POINT ( 'NONE',  ( -199.9999999999998579, 24.82633483071252201, 44.86878812508700776 ) ) ;
#629 = CARTESIAN_POINT ( 'NONE',  ( 199.9999999999999432, -14.14213562373096345, -14.14213562373104871 ) ) ;
#630 = CARTESIAN_POINT ( 'NONE',  ( -39.81953879995582213, -16.38089232936994222, 32.18669035977284665 ) ) ;
#631 = EDGE_CURVE ( 'NONE', #993, #19515, #17493, .T. ) ;
#632 = CARTESIAN_POINT ( 'NONE',  ( -4.151555265633182223, 23.42746911247800057, -42.97219445042047425 ) ) ;
#633 = CARTESIAN_POINT ( 'NONE',  ( 199.0262887415137527, -15.87643591937917442, 12.17243215972436055 ) ) ;
#634 = CARTESIAN_POINT ( 'NONE',  ( -259.2033419157646676, 21.55415060305790931, 35.01439189186571355 ) ) ;
#635 = CARTESIAN_POINT ( 'NONE',  ( -77.59415595804631494, -21.92621357339736221, 2.768978254285019425 ) ) ;
#636 = SURFACE_SIDE_STYLE ('',( #25248 ) ) ;
#637 = CARTESIAN_POINT ( 'NONE',  ( -190.7346372394937077, -13.94676542150760312, 47.78727444208784192 ) ) ;
#638 = CARTESIAN_POINT ( 'NONE',  ( -280.0000000000000000, 14.14213562373078581, 14.14213562373108424 ) ) ;
#639 = ADVANCED_FACE ( 'NONE', ( #7380 ), #10777, .T. ) ;
#640 = CARTESIAN_POINT ( 'NONE',  ( 4.995406935893287326, 17.50105314357170627, 39.06748935135200895 ) ) ;
#641 = CARTESIAN_POINT ( 'NONE',  ( -280.0000000000000000, -14.14213562373118549, 14.14213562373078936 ) ) ;
#642 = CARTESIAN_POINT ( 'NONE',  ( -91.56559293963836410, 16.03295912088692177, 16.03295912088721664 ) ) ;
#644 = CARTESIAN_POINT ( 'NONE',  ( -100.7734535825088358, 12.25131212657497848, -12.25131212657469604 ) ) ;
#643 = CARTESIAN_POINT ( 'NONE',  ( -238.4067589809705794, 27.60227080167080160, -28.96627169325299533 ) ) ;
#645 = CARTESIAN_POINT ( 'NONE',  ( -259.2033419157646676, 49.83842185052017015, 6.730120644404137487 ) ) ;
#646 = CARTESIAN_POINT ( 'NONE',  ( 136.1360204305621266, 35.03383547441298163, 40.00000000000002132 ) ) ;
#647 = CARTESIAN_POINT ( 'NONE',  ( -213.1075012329537230, 13.71589010951907817, -40.00000000000002132 ) ) ;
#648 = CARTESIAN_POINT ( 'NONE',  ( -238.4067589809705794, 28.96627169325324758, -27.60227080167054581 ) ) ;
#649 = CARTESIAN_POINT ( 'NONE',  ( -102.4294859495854411, 20.29697089060380222, -8.407280617849153259 ) ) ;
#650 = CARTESIAN_POINT ( 'NONE',  ( -213.1075012329536946, -37.98287015391210275, -37.98287015391272092 ) ) ;
#651 = CARTESIAN_POINT ( 'NONE',  ( -151.7004365444681468, 32.50163950438717109, -13.46261988206755333 ) ) ;
#652 = ORIENTED_EDGE ( 'NONE', *, *, #9331, .F. ) ;
#653 = CARTESIAN_POINT ( 'NONE',  ( -213.1075012329537230, 66.26714140136188291, 9.698598906438215650 ) ) ;
#654 = CARTESIAN_POINT ( 'NONE',  ( -86.86493150570990451, 7.943527260495432785, 19.77569912839167898 ) ) ;
#655 = CARTESIAN_POINT ( 'NONE',  ( -135.8532207217289738, -21.81201906317788186, 21.81201906317762962 ) ) ;
#656 = CARTESIAN_POINT ( 'NONE',  ( 16.03312633933773768, -44.50221493480259483, -18.43342098165166121 ) ) ;
#657 = ORIENTED_EDGE ( 'NONE', *, *, #3627, .F. ) ;
#658 = CARTESIAN_POINT ( 'NONE',  ( -678.9461782662772293, 75.00000000000000000, 35.00000000000159162 ) ) ;
#659 = CARTESIAN_POINT ( 'NONE',  ( 190.0000000000000000, 52.50000000000007816, -52.49999999999999289 ) ) ;
#660 = CARTESIAN_POINT ( 'NONE',  ( 199.9999999999999432, 6.681520191215184035, -17.78964488229654251 ) ) ;
#661 = CARTESIAN_POINT ( 'NONE',  ( -114.5523123854244716, -20.89198064830845425, 6.807555700458482129 ) ) ;
#662 = CARTESIAN_POINT ( 'NONE',  ( 91.82158438592158234, 22.79471317813472098, 2.449293598294708485E-15 ) ) ;
#663 = CARTESIAN_POINT ( 'NONE',  ( -105.4894168351564048, 19.67999904371083275, 8.151722511394638104 ) ) ;
#664 = CARTESIAN_POINT ( 'NONE',  ( 199.0161420530203600, 13.89456085230456850, 14.38651294782529888 ) ) ;
#665 = PRESENTATION_LAYER_ASSIGNMENT (  '', '', ( #24456 ) ) ;
#666 = CARTESIAN_POINT ( 'NONE',  ( 130.8568914410475088, -4.207082182990058428, 52.36146031193416661 ) ) ;
#667 = CARTESIAN_POINT ( 'NONE',  ( 91.82158438592158234, -6.516925787240506436E-14, 22.79471317813470321 ) ) ;
#668 = CARTESIAN_POINT ( 'NONE',  ( 57.59792236341146321, 40.00000000000004263, -2.435789363418021214 ) ) ;
#669 = CARTESIAN_POINT ( 'NONE',  ( -362.0709805440841365, -10.00000000000005684, 1.224646799147354440E-15 ) ) ;
#670 = CARTESIAN_POINT ( 'NONE',  ( -30.26275506840322649, -41.69427246844630019, -2.449293598294708485E-15 ) ) ;
#672 = CARTESIAN_POINT ( 'NONE',  ( 19.06497207195981147, -10.03556273973439517, 10.03556273973429214 ) ) ;
#671 = CARTESIAN_POINT ( 'NONE',  ( 23.42154907652910012, -13.79745687233715046, -46.79103593565392316 ) ) ;
#673 = CARTESIAN_POINT ( 'NONE',  ( 200.0000000000000000, -19.99999999999988631, -40.00000000000002132 ) ) ;
#674 = CARTESIAN_POINT ( 'NONE',  ( 163.1118516004056573, 19.27778845539212327, 37.29075403953164169 ) ) ;
#675 = CARTESIAN_POINT ( 'NONE',  ( 156.1979191798867248, -11.34289806466571271, -27.38417834433185760 ) ) ;
#676 = CARTESIAN_POINT ( 'NONE',  ( -716.9846540392142060, 66.50000000000009948, 61.50000000000005684 ) ) ;
#677 = CARTESIAN_POINT ( 'NONE',  ( -91.56559293963834989, 1.671088883502053755E-13, -17.32597176626811120 ) ) ;
#678 = CARTESIAN_POINT ( 'NONE',  ( 14.38125909742180930, 39.99999999999982947, 55.17850393971022527 ) ) ;
#679 = CARTESIAN_POINT ( 'NONE',  ( 130.8568914410475088, 4.207082182989741348, -52.36146031193420924 ) ) ;
#680 = PLANE ( 'NONE',  #24960 ) ;
#681 = CARTESIAN_POINT ( 'NONE',  ( -86.86493150571116928, -8.366608963953867217, -19.60045294882765887 ) ) ;
#682 = CARTESIAN_POINT ( 'NONE',  ( 14.38125909742182529, -39.01709431150933938, 39.01709431150894147 ) ) ;
#683 = ORIENTED_EDGE ( 'NONE', *, *, #9481, .F. ) ;
#684 = CARTESIAN_POINT ( 'NONE',  ( -192.9588430854689989, -10.23066800230742501, -10.23066800230756712 ) ) ;
#685 = FACE_OUTER_BOUND ( 'NONE', #11342, .T. ) ;
#686 = CARTESIAN_POINT ( 'NONE',  ( 163.1118516004056573, -12.73709011382471878, -40.00000000000002132 ) ) ;
#687 = EDGE_CURVE ( 'NONE', #14320, #23489, #997, .T. ) ;
#688 = CARTESIAN_POINT ( 'NONE',  ( -114.6679276626366430, 11.81543316366880525, -18.60595090114481920 ) ) ;
#689 = CARTESIAN_POINT ( 'NONE',  ( 151.7948205124836250, -23.49921654116371883, 23.49921654116317526 ) ) ;
#690 =( NAMED_UNIT ( * ) SI_UNIT ( $, .STERADIAN. ) SOLID_ANGLE_UNIT ( ) );
#691 = ORIENTED_EDGE ( 'NONE', *, *, #23589, .F. ) ;
#692 = AXIS2_PLACEMENT_3D ( 'NONE', #22776, #2285, #14907 ) ;
#693 = EDGE_LOOP ( 'NONE', ( #13184, #9222, #23705, #13464 ) ) ;
#694 = AXIS2_PLACEMENT_3D ( 'NONE', #21020, #25155, #15023 ) ;
#695 = CARTESIAN_POINT ( 'NONE',  ( 199.9999999999999147, 3.087032903897462432, 18.75855398088509318 ) ) ;
#696 = DIRECTION ( 'NONE',  ( 1.000000000000000000, 0.000000000000000000, 0.000000000000000000 ) ) ;
#697 = EDGE_CURVE ( 'NONE', #5841, #23332, #14292, .T. ) ;
#698 = ORIENTED_EDGE ( 'NONE', *, *, #18324, .T. ) ;
#699 = ORIENTED_EDGE ( 'NONE', *, *, #4311, .T. ) ;
#700 = CARTESIAN_POINT ( 'NONE',  ( -280.0000000000000568, -42.42640687119295251, 14.14213562373088351 ) ) ;
#701 = CARTESIAN_POINT ( 'NONE',  ( 199.0171635947087907, -15.67013318013508716, -12.42972081464992407 ) ) ;
#702 = LINE ( 'NONE', #834, #8135 ) ;
#703 =( REPRESENTATION_RELATIONSHIP ('NONE','NONE', #23888, #9131 ) REPRESENTATION_RELATIONSHIP_WITH_TRANSFORMATION ( #1591 )SHAPE_REPRESENTATION_RELATIONSHIP( ) );
#704 = EDGE_CURVE ( 'NONE', #13948, #1209, #14934, .T. ) ;
#705 = AXIS2_PLACEMENT_3D ( 'NONE', #5212, #19434, #1220 ) ;
#706 = CARTESIAN_POINT ( 'NONE',  ( -105.3755690713226585, -15.38646221621796251, 41.18208027870593924 ) ) ;
#707 = CARTESIAN_POINT ( 'NONE',  ( 14.38125909742180752, 10.73282306404720465, 10.73282306404724018 ) ) ;
#708 = CARTESIAN_POINT ( 'NONE',  ( 146.6084372240433709, 40.00000000000017053, -34.62501878078291639 ) ) ;
#709 = CARTESIAN_POINT ( 'NONE',  ( -114.4364955367328491, -20.29001642038857156, 8.064892380842218600 ) ) ;
#710 = DIRECTION ( 'NONE',  ( 0.000000000000000000, 0.000000000000000000, -1.000000000000000000 ) ) ;
#711 = CARTESIAN_POINT ( 'NONE',  ( 14.38125909742181818, 5.830552384690105017E-13, -55.17850393972636880 ) ) ;
#712 = CARTESIAN_POINT ( 'NONE',  ( 0.2972598230769957217, 1.502051041545559470E-13, -14.33493731733933352 ) ) ;
#713 = DIRECTION ( 'NONE',  ( 0.000000000000000000, 0.000000000000000000, 1.000000000000000000 ) ) ;
#714 = CARTESIAN_POINT ( 'NONE',  ( -87.13361725327075646, -16.16779225783700724, -14.22820416757983253 ) ) ;
#715 = CARTESIAN_POINT ( 'NONE',  ( 199.0068072339493597, 19.36029496603142874, -5.002335373038918398 ) ) ;
#716 = CARTESIAN_POINT ( 'NONE',  ( -190.0144222803280627, 13.91469272132741963, 47.57278142030602908 ) ) ;
#717 = CARTESIAN_POINT ( 'NONE',  ( 200.0000000000000000, -14.14213562373122457, 42.42640687119282461 ) ) ;
#718 = CARTESIAN_POINT ( 'NONE',  ( -93.02511667907126025, 8.946512270084744145, 20.50052124204852078 ) ) ;
#719 = CARTESIAN_POINT ( 'NONE',  ( 200.0000000000000000, 14.14213562373083022, 42.42640687119289566 ) ) ;
#720 = CARTESIAN_POINT ( 'NONE',  ( -77.55743582226475041, 22.12574471220127137, 0.8414656003864237066 ) ) ;
#721 = CARTESIAN_POINT ( 'NONE',  ( 163.1118516004056573, 19.27778845539265618, -37.29075403953135037 ) ) ;
#722 = CARTESIAN_POINT ( 'NONE',  ( -661.7419054499291633, 44.81143869219462772, -4.158744080377950070 ) ) ;
#723 = CARTESIAN_POINT ( 'NONE',  ( -135.8532207217289738, 9.153146818113546246, -0.000000000000000000 ) ) ;
#724 = VECTOR ( 'NONE', #14723, 1000.000000000000000 ) ;
#725 = CARTESIAN_POINT ( 'NONE',  ( -100.7734535825088500, 12.25131212657428748, 44.31723036834913643 ) ) ;
#726 = CARTESIAN_POINT ( 'NONE',  ( 57.59792236341147031, 2.435789363418170872, 40.00000000000002132 ) ) ;
#727 = VECTOR ( 'NONE', #18095, 1000.000000000000000 ) ;
#728 = CARTESIAN_POINT ( 'NONE',  ( -592.0657137250348114, 44.93697794005576185, -2.456499637838828853 ) ) ;
#729 = ORIENTED_EDGE ( 'NONE', *, *, #3071, .F. ) ;
#730 = CARTESIAN_POINT ( 'NONE',  ( 0.2972598230770103767, -39.99999999999945288, -54.33493731733979359 ) ) ;
#731 = CARTESIAN_POINT ( 'NONE',  ( 199.0058341074146142, 9.150281110520873895, -17.78147227136547670 ) ) ;
#732 = DIRECTION ( 'NONE',  ( 1.000000000000000000, 1.836970198721030181E-16, 0.000000000000000000 ) ) ;
#733 = ORIENTED_EDGE ( 'NONE', *, *, #5255, .F. ) ;
#734 = ORIENTED_EDGE ( 'NONE', *, *, #20024, .F. ) ;
#735 = ORIENTED_EDGE ( 'NONE', *, *, #6535, .T. ) ;
#736 = CARTESIAN_POINT ( 'NONE',  ( 130.8568914410475088, 5.949712681206712261, 40.00000000000002132 ) ) ;
#737 = EDGE_CURVE ( 'NONE', #992, #2989, #22534, .T. ) ;
#738 = CARTESIAN_POINT ( 'NONE',  ( -100.0968563617347797, -20.72609133250457703, -8.149320301440017289 ) ) ;
#739 = CARTESIAN_POINT ( 'NONE',  ( -105.4741150117382489, -19.77569912955116749, -7.943527260750408381 ) ) ;
#740 = CIRCLE ( 'NONE', #4985, 5.000000000000095035 ) ;
#741 = CARTESIAN_POINT ( 'NONE',  ( 146.6084372240433993, -24.48358557860319706, -24.48358557860330720 ) ) ;
#742 = CARTESIAN_POINT ( 'NONE',  ( -30.26275506840324070, -1.147469862568086380E-14, 1.694272468446259783 ) ) ;
#743 = CARTESIAN_POINT ( 'NONE',  ( 199.9999999999999432, 6.681520191215184035, -17.78964488229654251 ) ) ;
#744 = CARTESIAN_POINT ( 'NONE',  ( 199.9999999999999147, -5.229706238425958276, -18.27161031230872368 ) ) ;
#745 = CARTESIAN_POINT ( 'NONE',  ( 0.2972598230770011618, 10.13633138497555919, -66.70487387989845729 ) ) ;
#746 = CARTESIAN_POINT ( 'NONE',  ( 146.6084372240433709, -3.800685668859084210, 52.76785682606516303 ) ) ;
#747 = DIRECTION ( 'NONE',  ( 1.000000000000000000, 1.836970198721030181E-16, 0.000000000000000000 ) ) ;
#748 = CARTESIAN_POINT ( 'NONE',  ( -162.0762913951021176, 40.00000000000001421, -1.694272876827905394 ) ) ;
#749 = DIRECTION ( 'NONE',  ( -1.000000000000000000, -1.836970198721030181E-16, 0.000000000000000000 ) ) ;
#750 = CARTESIAN_POINT ( 'NONE',  ( -135.8532207217289738, 9.153146818113546246, -0.000000000000000000 ) ) ;
#751 = CARTESIAN_POINT ( 'NONE',  ( -280.0000000000000568, 14.14213562373067745, 42.42640687119295251 ) ) ;
#752 = CARTESIAN_POINT ( 'NONE',  ( 199.0072939989582324, 19.72179417679889823, -3.362695692811099590 ) ) ;
#754 = CARTESIAN_POINT ( 'NONE',  ( -87.13361725327074225, -15.19799821270821560, -15.19799821270861884 ) ) ;
#753 = CARTESIAN_POINT ( 'NONE',  ( -56.48582580120559271, -6.472252184284276844, 6.472252184284108978 ) ) ;
#755 = CARTESIAN_POINT ( 'NONE',  ( -192.9588430854689989, 14.46834944099965981, 0.000000000000000000 ) ) ;
#756 = CARTESIAN_POINT ( 'NONE',  ( 151.7948205124836250, -23.49921654116339553, -23.49921654116350211 ) ) ;
#757 = CARTESIAN_POINT ( 'NONE',  ( 163.1118516004056573, -27.26290988616869626, 0.000000000000000000 ) ) ;
#758 = ORIENTED_EDGE ( 'NONE', *, *, #3424, .F. ) ;
#759 = CARTESIAN_POINT ( 'NONE',  ( 17.65190074001006693, -48.50354960737486465, 14.05440436229930867 ) ) ;
#760 = CARTESIAN_POINT ( 'NONE',  ( -192.9588430854690273, 14.46834944099966336, -40.00000000000002132 ) ) ;
#761 = ORIENTED_EDGE ( 'NONE', *, *, #11193, .T. ) ;
#762 = CARTESIAN_POINT ( 'NONE',  ( -105.2334157265390502, 16.99665894158216872, -13.14152336620543338 ) ) ;
#763 = CARTESIAN_POINT ( 'NONE',  ( -56.48582580120559982, -34.75652343174615311, 21.81201906317766870 ) ) ;
#764 = CARTESIAN_POINT ( 'NONE',  ( -70.30307074955213409, -8.711708290686113187, 23.14841683089695934 ) ) ;
#765 = CARTESIAN_POINT ( 'NONE',  ( -82.26600655510863191, 19.56860215688234561, -4.953608811515387345 ) ) ;
#766 = CARTESIAN_POINT ( 'NONE',  ( -5.859158571312478081, 23.09435402965887363, -42.46836465824239326 ) ) ;
#767 = CARTESIAN_POINT ( 'NONE',  ( 199.0263606093525652, -14.93202714917829965, 13.31409215216611663 ) ) ;
#768 = CARTESIAN_POINT ( 'NONE',  ( 130.8568914410475088, 4.207082182989012153, 52.36146031193425188 ) ) ;
#769 = CARTESIAN_POINT ( 'NONE',  ( -87.13361725327075646, -21.49321519333432207, -1.155557966632341512E-30 ) ) ;
#770 = DIRECTION ( 'NONE',  ( 0.000000000000000000, 1.000000000000000000, 0.000000000000000000 ) ) ;
#771 = CARTESIAN_POINT ( 'NONE',  ( -188.4265466358341428, -13.83489705870445263, 47.03621809928723252 ) ) ;
#772 = CARTESIAN_POINT ( 'NONE',  ( 184.8905102610680444, 14.79361573936375507, 14.79361573936398067 ) ) ;
#773 = CARTESIAN_POINT ( 'NONE',  ( -105.3755690713226727, 15.38646221621793231, -15.38646221621779020 ) ) ;
#774 = CARTESIAN_POINT ( 'NONE',  ( -280.0000000000000568, -42.42640687119276066, -14.14213562373147148 ) ) ;
#775 = CARTESIAN_POINT ( 'NONE',  ( -86.86493150571114086, -7.943527260496002107, 19.77569912839178912 ) ) ;
#777 = CARTESIAN_POINT ( 'NONE',  ( 146.6084372240433709, 32.08495691632030145, 24.48358557860365181 ) ) ;
#776 = LINE ( 'NONE', #12604, #24053 ) ;
#778 = CARTESIAN_POINT ( 'NONE',  ( 130.8568914410475372, 4.207082182992923691, -4.207082182992794017 ) ) ;
#779 = CARTESIAN_POINT ( 'NONE',  ( 170.2234770963711128, 24.55285855007190676, 40.00000000000002132 ) ) ;
#780 = CARTESIAN_POINT ( 'NONE',  ( 192.4448373802101173, 19.99999999996065014, -40.00000000000002132 ) ) ;
#781 = CARTESIAN_POINT ( 'NONE',  ( 91.82158438592158234, 16.11829626348434630, -40.45024623143955012 ) ) ;
#782 = PRODUCT_RELATED_PRODUCT_CATEGORY ( 'part', '', ( #10401 ) ) ;
#783 = CARTESIAN_POINT ( 'NONE',  ( -314.0000000000000568, -4.857225732735059864E-14, 0.000000000000000000 ) ) ;
#784 = CARTESIAN_POINT ( 'NONE',  ( 0.2972598230770027716, -38.42060263243681817, 18.14793986248684377 ) ) ;
#785 = CARTESIAN_POINT ( 'NONE',  ( -184.9729924864344355, 42.02333070177955676, -22.80024897327513500 ) ) ;
#786 = ORIENTED_EDGE ( 'NONE', *, *, #16697, .F. ) ;
#787 = CARTESIAN_POINT ( 'NONE',  ( 19.06497207195981858, 10.03556273973424062, 66.60410523465820631 ) ) ;
#788 = CARTESIAN_POINT ( 'NONE',  ( -86.95457011089800403, -19.12034330075778854, -9.640471311020448297 ) ) ;
#789 = ITEM_DEFINED_TRANSFORMATION ( 'NONE', 'NONE', #7845,  #21058 ) ;
#790 = CARTESIAN_POINT ( 'NONE',  ( 199.9999999999999432, -14.14213562373093680, 14.14213562373082311 ) ) ;
#791 = CARTESIAN_POINT ( 'NONE',  ( 9.345847406375622057, -49.32890504404500831, -14.17927947630055741 ) ) ;
#792 = EDGE_LOOP ( 'NONE', ( #18200, #12963, #12220, #17200 ) ) ;
#793 = DIRECTION ( 'NONE',  ( -0.01051738777840850216, -0.9307051272558640731, 0.3656191333258757004 ) ) ;
#794 = CARTESIAN_POINT ( 'NONE',  ( -110.0738206587849390, -10.29063887146194034, -17.41030175792333168 ) ) ;
#795 = EDGE_CURVE ( 'NONE', #24980, #854, #10474, .T. ) ;
#796 = CARTESIAN_POINT ( 'NONE',  ( 200.0000000000003126, 10.03286793820859835, -16.13825081434616493 ) ) ;
#797 = CARTESIAN_POINT ( 'NONE',  ( -114.6679276626352788, -21.51116696530653627, -4.801621139945174477 ) ) ;
#798 = CARTESIAN_POINT ( 'NONE',  ( -86.96347745069644475, 18.24025645688350750, -40.00000000000002132 ) ) ;
#799 = CARTESIAN_POINT ( 'NONE',  ( 146.6084372240433709, -52.76785682606510619, -3.800685668859292043 ) ) ;
#800 = CARTESIAN_POINT ( 'NONE',  ( 199.0185982156405089, 10.13449990482401297, 17.24443922940779927 ) ) ;
#801 = CARTESIAN_POINT ( 'NONE',  ( 57.59792236341147031, -26.56190807104712448, 30.00663442387673285 ) ) ;
#802 = CARTESIAN_POINT ( 'NONE',  ( -208.1127848780265026, -2.327190355601776466E-13, 55.00245453012672670 ) ) ;
#803 = CARTESIAN_POINT ( 'NONE',  ( -30.26275506840324425, 39.99999999999987210, 41.69427246844643520 ) ) ;
#804 = CARTESIAN_POINT ( 'NONE',  ( 184.8905102610680444, 1.070102760522089011E-13, -20.92133201514444352 ) ) ;
#805 = CARTESIAN_POINT ( 'NONE',  ( -280.0000000000000568, -20.00000000000006395, -40.00000000000002132 ) ) ;
#807 = CARTESIAN_POINT ( 'NONE',  ( -617.0807177054949761, 28.23630110923742365, 28.33531756806318214 ) ) ;
#806 = CARTESIAN_POINT ( 'NONE',  ( 25.62979979008735043, -22.88075396656093830, -42.16299361905900867 ) ) ;
#808 = CARTESIAN_POINT ( 'NONE',  ( -213.1075012329537230, -53.71589010953668719, -40.00000000000002132 ) ) ;
#809 = CARTESIAN_POINT ( 'NONE',  ( 14.38125909742180752, 17.55144818341448953, 39.01709431150923280 ) ) ;
#810 = CARTESIAN_POINT ( 'NONE',  ( 167.0466155511619490, -9.710058186601607133, -23.44215416552599152 ) ) ;
#811 = LINE ( 'NONE', #8516, #13626 ) ;
#812 = CARTESIAN_POINT ( 'NONE',  ( 4.995406935893306866, -39.99999999999944578, -55.24977328856505920 ) ) ;
#813 = FACE_OUTER_BOUND ( 'NONE', #11620, .T. ) ;
#814 = CARTESIAN_POINT ( 'NONE',  ( 155.1202959361052365, -27.79909075771130844, -11.51476041348459667 ) ) ;
#815 = CARTESIAN_POINT ( 'NONE',  ( -280.0000000000000000, -14.14213562373118549, 14.14213562373078936 ) ) ;
#816 = CARTESIAN_POINT ( 'NONE',  ( -86.96347745069643054, 15.38646221621763210, 41.18208027870604582 ) ) ;
#817 = VERTEX_POINT ( 'NONE', #14658 ) ;
#819 = CARTESIAN_POINT ( 'NONE',  ( -7.769366557093614567, 45.69637362129925862, -13.56374645825293257 ) ) ;
#818 = CARTESIAN_POINT ( 'NONE',  ( -77.79405973474302982, -6.791823288762519617, -20.85724814835166896 ) ) ;
#820 = FACE_OUTER_BOUND ( 'NONE', #17080, .T. ) ;
#821 = CARTESIAN_POINT ( 'NONE',  ( 130.8568914410475088, -5.949712681206671405, 40.00000000000002132 ) ) ;
#822 = AXIS2_PLACEMENT_3D ( 'NONE', #9624, #3638, #5764 ) ;
#823 = CARTESIAN_POINT ( 'NONE',  ( -678.9461782662789346, 90.00000000000000000, -24.99999999999826628 ) ) ;
#824 = CARTESIAN_POINT ( 'NONE',  ( -188.3392535381696007, 47.00481007172025727, -13.83023904993444120 ) ) ;
#825 =( NAMED_UNIT ( * ) SI_UNIT ( $, .STERADIAN. ) SOLID_ANGLE_UNIT ( ) );
#826 = ORIENTED_EDGE ( 'NONE', *, *, #944, .T. ) ;
#827 = ORIENTED_EDGE ( 'NONE', *, *, #8764, .F. ) ;
#828 = CARTESIAN_POINT ( 'NONE',  ( 85.88525995973293448, -8.769880560541459147, 23.37195345519199563 ) ) ;
#829 = CARTESIAN_POINT ( 'NONE',  ( 98.29820294267858571, 2.581272653895909208, 20.00000000000376588 ) ) ;
#830 = EDGE_LOOP ( 'NONE', ( #20781, #4653, #520, #427 ) ) ;
#831 = EDGE_LOOP ( 'NONE', ( #23466, #9560, #14259, #11065 ) ) ;
#832 = CARTESIAN_POINT ( 'NONE',  ( 146.6084372240433993, -24.48358557860319706, -24.48358557860330720 ) ) ;
#833 = CARTESIAN_POINT ( 'NONE',  ( 199.0220583073800640, -19.74674823417053915, -3.257374120286249397 ) ) ;
#834 = CARTESIAN_POINT ( 'NONE',  ( -678.9461782662772293, 75.00000000000000000, 25.00000000000157385 ) ) ;
#835 = CARTESIAN_POINT ( 'NONE',  ( 91.82158438592158234, -40.45024623143958564, 16.11829626348418998 ) ) ;
#836 = CARTESIAN_POINT ( 'NONE',  ( -135.8532207217289738, -6.472252184284190690, -6.472252184284188914 ) ) ;
#837 = CARTESIAN_POINT ( 'NONE',  ( 91.82158438592156813, 39.99999999999995737, 22.79471317813484887 ) ) ;
#838 = CARTESIAN_POINT ( 'NONE',  ( -199.9999999999999716, -22.84381638316559204, 44.98788141756676140 ) ) ;
#839 = CARTESIAN_POINT ( 'NONE',  ( -199.9999999999999432, 10.02640517461945890, 53.44529986889378392 ) ) ;
#840 = CARTESIAN_POINT ( 'NONE',  ( -30.26275506840324070, -40.00000000000001421, -1.694272468446678559 ) ) ;
#841 = CARTESIAN_POINT ( 'NONE',  ( -30.26275506840323359, 4.336144384597734078E-13, -41.69427246844629309 ) ) ;
#842 = CARTESIAN_POINT ( 'NONE',  ( -110.0368417077420560, -18.51665893310633848, 7.992411109433169791 ) ) ;
#843 = CARTESIAN_POINT ( 'NONE',  ( -87.13361725327075646, 15.19799821270843765, 15.19799821270837015 ) ) ;
#844 = CARTESIAN_POINT ( 'NONE',  ( 199.0053210531128229, 14.60061869579413063, -13.67646033072836786 ) ) ;
#845 = VECTOR ( 'NONE', #18191, 1000.000000000000000 ) ;
#846 = CARTESIAN_POINT ( 'NONE',  ( -86.96347745069644475, 15.38646221621793586, -15.38646221621778842 ) ) ;
#847 = CARTESIAN_POINT ( 'NONE',  ( 136.1360204305621266, -3.511608612531119000, 53.05693388239312469 ) ) ;
#848 = LINE ( 'NONE', #8957, #8452 ) ;
#849 = CARTESIAN_POINT ( 'NONE',  ( 146.6084372240433993, -3.800685668858652999, 3.800685668858636568 ) ) ;
#850 = CARTESIAN_POINT ( 'NONE',  ( -280.0000000000000568, 14.14213562373127431, -42.42640687119274645 ) ) ;
#851 = CARTESIAN_POINT ( 'NONE',  ( -642.7070543445415751, 32.34947999245193273, 31.28956669078001340 ) ) ;
#852 = CARTESIAN_POINT ( 'NONE',  ( -198.0356074513804572, -15.37879056873074290, 40.00000000000002132 ) ) ;
#853 = B_SPLINE_CURVE_WITH_KNOTS ( 'NONE', 3,
 ( #22849, #4624, #12724, #20848, #2626, #10738 ),
 .UNSPECIFIED., .F., .F.,
 ( 4, 2, 4 ),
 ( -0.0001050551439129801008, 0.04006586859759233427, 0.08023679233909764008 ),
 .UNSPECIFIED. ) ;
#854 = VERTEX_POINT ( 'NONE', #22798 ) ;
#855 = CARTESIAN_POINT ( 'NONE',  ( -56.48582580120559982, 50.09629031063956717, 6.472252184284792875 ) ) ;
#856 = CARTESIAN_POINT ( 'NONE',  ( 151.7948205124835681, 33.23291073765556547, 40.00000000000002132 ) ) ;
#857 = CARTESIAN_POINT ( 'NONE',  ( -592.4919920315402351, 44.60627086681392228, -6.055351194787411906 ) ) ;
#858 = VERTEX_POINT ( 'NONE', #4575 ) ;
#859 = CARTESIAN_POINT ( 'NONE',  ( 19.06497207195981858, 5.735870351258996432E-13, -54.19242893257843008 ) ) ;
#860 = CARTESIAN_POINT ( 'NONE',  ( 199.0089017020823121, -1.168865339877916965, -19.99575268797839911 ) ) ;
#861 = CARTESIAN_POINT ( 'NONE',  ( 200.0000000000000000, 66.50000000000009948, -66.50000000000005684 ) ) ;
#862 = VERTEX_POINT ( 'NONE', #20801 ) ;
#863 = ORIENTED_EDGE ( 'NONE', *, *, #704, .T. ) ;
#864 = ORIENTED_EDGE ( 'NONE', *, *, #26060, .T. ) ;
#865 = CARTESIAN_POINT ( 'NONE',  ( -213.1075012329537230, 53.71589010953660193, 40.00000000000002132 ) ) ;
#866 = CARTESIAN_POINT ( 'NONE',  ( -105.4732637872227770, -19.68494377761401992, -8.153770687239941140 ) ) ;
#867 = AXIS2_PLACEMENT_3D ( 'NONE', #5163, #9025, #21137 ) ;
#868 = DIRECTION ( 'NONE',  ( 0.000000000000000000, 0.7071067811865434649, 0.7071067811865516806 ) ) ;
#869 = EDGE_CURVE ( 'NONE', #20514, #9693, #9078, .T. ) ;
#870 = CARTESIAN_POINT ( 'NONE',  ( -114.4364955367327070, -8.644468109209471507, 20.04994829327649342 ) ) ;
#871 = CARTESIAN_POINT ( 'NONE',  ( -56.48582580120559271, 2.158176344243877536E-14, -9.153146818113587102 ) ) ;
#872 = CARTESIAN_POINT ( 'NONE',  ( 199.9999999999996021, 9.500464834803043601, -16.45734938164063621 ) ) ;
#873 = CARTESIAN_POINT ( 'NONE',  ( 199.9999999999999432, 2.163685940895884841, -18.88015187541845918 ) ) ;
#874 = CARTESIAN_POINT ( 'NONE',  ( -56.48582580120559982, -34.75652343174584047, -21.81201906317815187 ) ) ;
#875 = CARTESIAN_POINT ( 'NONE',  ( -280.0000000000000000, 14.14213562373078581, 14.14213562373108424 ) ) ;
#876 = LINE ( 'NONE', #6848, #22484 ) ;
#877 = CARTESIAN_POINT ( 'NONE',  ( 4.995406935893298872, 5.820775922023080204E-13, -55.24977328854835434 ) ) ;
#878 = CARTESIAN_POINT ( 'NONE',  ( 160.9163046357249129, -135.7889608577475542, -55.61140153332245006 ) ) ;
#879 = CARTESIAN_POINT ( 'NONE',  ( 210.0000000000000284, 69.29737539576909455, -75.30386416458597409 ) ) ;
#880 = EDGE_CURVE ( 'NONE', #12353, #2322, #17250, .T. ) ;
#881 = ADVANCED_FACE ( 'NONE', ( #17061 ), #19573, .T. ) ;
#882 = CARTESIAN_POINT ( 'NONE',  ( 4.995406935893310418, -67.35176059880237176, 10.78321810387813429 ) ) ;
#883 = CARTESIAN_POINT ( 'NONE',  ( 199.0119004238765967, 18.48644426806060181, 7.626980851762527713 ) ) ;
#884 = COLOUR_RGB ( '',0.7921568627450980005, 0.8196078431372548767, 0.9333333333333333481 ) ;
#886 = CARTESIAN_POINT ( 'NONE',  ( 130.8568914410475088, 40.00000000000015632, -34.05028731879774284 ) ) ;
#885 = CARTESIAN_POINT ( 'NONE',  ( -91.56559293963834989, -16.03295912088728414, 16.03295912088688269 ) ) ;
#887 = CARTESIAN_POINT ( 'NONE',  ( -56.48582580120559982, -9.153146818113595984, -40.00000000000002132 ) ) ;
#888 = CARTESIAN_POINT ( 'NONE',  ( -259.2033419157646676, -6.730120644403667640, 49.83842185052029805 ) ) ;
#889 = CARTESIAN_POINT ( 'NONE',  ( 192.4448373802100889, -20.00000000003938538, 0.000000000000000000 ) ) ;
#890 = ORIENTED_EDGE ( 'NONE', *, *, #2098, .F. ) ;
#891 = CARTESIAN_POINT ( 'NONE',  ( -1.087763065927232153, -43.78960619332504223, 24.03018639662561640 ) ) ;
#892 = CARTESIAN_POINT ( 'NONE',  ( 192.4448373802101173, 19.99999999996065014, -40.00000000000002132 ) ) ;
#893 = DIRECTION ( 'NONE',  ( -1.000000000000000000, -1.836970198721030181E-16, 0.000000000000000000 ) ) ;
#894 = CARTESIAN_POINT ( 'NONE',  ( -238.4067589809705794, 28.96627169325315165, 28.96627169325329731 ) ) ;
#895 = CARTESIAN_POINT ( 'NONE',  ( -213.1075012329537230, -40.00000000000011369, 13.71589010951897691 ) ) ;
#896 = CARTESIAN_POINT ( 'NONE',  ( -86.86493150571119770, 19.77569912839179622, -7.943527260495995002 ) ) ;
#897 = CARTESIAN_POINT ( 'NONE',  ( -1.818469002956039970, -13.93708913181221298, -47.72215409237463035 ) ) ;
#898 = CARTESIAN_POINT ( 'NONE',  ( 200.0000000000000000, -12.54535540268124372, 14.29661512548269187 ) ) ;
#899 = CARTESIAN_POINT ( 'NONE',  ( -238.4067589809705794, 57.25054294065799354, -0.6820004457334954973 ) ) ;
#900 = CARTESIAN_POINT ( 'NONE',  ( -82.23726319249652761, -20.19517362732918642, -9.977985540125272163E-16 ) ) ;
#901 = DIRECTION ( 'NONE',  ( 1.000000000000000000, -1.836970198721030181E-16, -0.000000000000000000 ) ) ;
#902 = CARTESIAN_POINT ( 'NONE',  ( 210.0000000000000284, 72.72568232011447265, -59.67546976104962653 ) ) ;
#903 = CARTESIAN_POINT ( 'NONE',  ( 136.1360204305621266, 24.77266263493104148, 24.77266263493145004 ) ) ;
#904 = CARTESIAN_POINT ( 'NONE',  ( 136.1360204305621551, 24.77266263493108411, 31.79587985999273769 ) ) ;
#905 = CARTESIAN_POINT ( 'NONE',  ( -82.30220482034344798, 7.992411108777224271, -18.51665893431685461 ) ) ;
#906 = CARTESIAN_POINT ( 'NONE',  ( -208.1127848780265026, -10.60833733269537227, -10.60833733269551793 ) ) ;
#908 = CARTESIAN_POINT ( 'NONE',  ( -100.7734535825088500, 40.53558337403654832, 16.03295912088756481 ) ) ;
#907 = CARTESIAN_POINT ( 'NONE',  ( -91.56559293963836410, 44.31723036834908669, -12.25131212657445801 ) ) ;
#909 = CARTESIAN_POINT ( 'NONE',  ( -208.1127848780265026, 38.89260858015777700, -38.89260858015687461 ) ) ;
#910 = CARTESIAN_POINT ( 'NONE',  ( 19.06497207195980792, 54.19242893257844429, -40.00000000000002132 ) ) ;
#911 = CARTESIAN_POINT ( 'NONE',  ( -105.3755690713226727, -15.38646221621786481, -15.38646221621789856 ) ) ;
#912 = CARTESIAN_POINT ( 'NONE',  ( -210.0000000000000284, 63.70262460423102624, -57.69613583541415380 ) ) ;
#913 = CARTESIAN_POINT ( 'NONE',  ( 19.06497207195982924, -66.60410523465809263, -10.03556273973493163 ) ) ;
#914 = AXIS2_PLACEMENT_3D ( 'NONE', #32, #18248, #10144 ) ;
#915 = CARTESIAN_POINT ( 'NONE',  ( -188.2956751479420063, 46.98904240251129494, -13.82790121914899117 ) ) ;
#916 = VERTEX_POINT ( 'NONE', #14930 ) ;
#917 = CARTESIAN_POINT ( 'NONE',  ( -238.4067589809705794, 28.96627169325315165, 28.96627169325329731 ) ) ;
#918 = AXIS2_PLACEMENT_3D ( 'NONE', #25838, #19695, #3477 ) ;
#919 = AXIS2_PLACEMENT_3D ( 'NONE', #13697, #7318, #23809 ) ;
#920 = CARTESIAN_POINT ( 'NONE',  ( -100.7734535825088500, 44.31723036834890905, 12.25131212657507795 ) ) ;
#921 = CARTESIAN_POINT ( 'NONE',  ( -16.87994666138489208, -42.52193590801358170, -12.91133298919152139 ) ) ;
#922 = ORIENTED_EDGE ( 'NONE', *, *, #11815, .T. ) ;
#923 = CARTESIAN_POINT ( 'NONE',  ( -188.8842190493880651, -43.30124183641380142, 17.93596163623971407 ) ) ;
#924 = B_SPLINE_CURVE_WITH_KNOTS ( 'NONE', 3,
 ( #606, #10717, #18826, #24964, #6711, #14825 ),
 .UNSPECIFIED., .F., .F.,
 ( 4, 2, 4 ),
 ( 0.0002283555316178395036, 0.004316741542439621673, 0.008405127553261403789 ),
 .UNSPECIFIED. ) ;
#925 = CARTESIAN_POINT ( 'NONE',  ( 199.9999999999999716, -3.557237102606629620, -18.66704445460036865 ) ) ;
#926 = CARTESIAN_POINT ( 'NONE',  ( 27.79909650602726856, -13.47302921521705699, 45.20561170653579097 ) ) ;
#927 = CARTESIAN_POINT ( 'NONE',  ( 192.4448373802101173, 19.99999999996065014, -40.00000000000002132 ) ) ;
#928 = CARTESIAN_POINT ( 'NONE',  ( 67.90397382965308282, 10.29861769495212798, -30.27708616508716233 ) ) ;
#929 = CARTESIAN_POINT ( 'NONE',  ( 199.0091071337781159, 19.93120984291649478, 1.649067560610785854 ) ) ;
#930 = AXIS2_PLACEMENT_3D ( 'NONE', #26089, #1997, #5984 ) ;
#931 = CARTESIAN_POINT ( 'NONE',  ( 136.1360204305621551, -31.79587985999279454, 24.77266263493094911 ) ) ;
#932 = CARTESIAN_POINT ( 'NONE',  ( 57.59792236341149163, -40.00000000000014211, 37.56421063658172699 ) ) ;
#933 = CARTESIAN_POINT ( 'NONE',  ( 0.2972598230769957217, -4.999556039334937811E-14, 14.33493731733933352 ) ) ;
#934 = CARTESIAN_POINT ( 'NONE',  ( -99.21568817060989431, 16.03295912088713848, -16.03295912088698927 ) ) ;
#935 = CARTESIAN_POINT ( 'NONE',  ( 146.6084372240433709, 34.62501878078307982, -40.00000000000002132 ) ) ;
#937 = CARTESIAN_POINT ( 'NONE',  ( -605.2485198462496783, 34.24030537962636345, 20.68249523888561470 ) ) ;
#936 = CARTESIAN_POINT ( 'NONE',  ( 23.49666234703804690, -23.31470603676250164, -42.81942870555072744 ) ) ;
#938 = CARTESIAN_POINT ( 'NONE',  ( 184.8905102610680444, 20.92133201514447194, 40.00000000000002132 ) ) ;
#939 = CARTESIAN_POINT ( 'NONE',  ( 4.995406935893287326, 17.50105314357170627, 39.06748935135200895 ) ) ;
#940 = CARTESIAN_POINT ( 'NONE',  ( -208.1127848780264742, 40.00000000000055422, -55.00245453014380814 ) ) ;
#941 = DIRECTION ( 'NONE',  ( -0.7071067811865302533, 0.000000000000000000, 0.7071067811865646702 ) ) ;
#942 = CARTESIAN_POINT ( 'NONE',  ( 91.82158438592159655, -39.99999999999976552, -22.79471317813512599 ) ) ;
#943 = CARTESIAN_POINT ( 'NONE',  ( 199.0250816517838359, -5.508431349499541163, 19.23181920140171997 ) ) ;
#944 = EDGE_CURVE ( 'NONE', #14912, #4726, #12582, .T. ) ;
#945 = CARTESIAN_POINT ( 'NONE',  ( 141.7942202792037563, -30.38864012024685479, -12.58738687988142857 ) ) ;
#946 = CARTESIAN_POINT ( 'NONE',  ( 151.7948205124836534, 4.785054706297857230, 51.78348778862544322 ) ) ;
#947 = CARTESIAN_POINT ( 'NONE',  ( 184.8905102610680444, -13.49065550809810965, 13.49065550809799596 ) ) ;
#948 = ORIENTED_EDGE ( 'NONE', *, *, #2831, .T. ) ;
#950 = CARTESIAN_POINT ( 'NONE',  ( -4.558244102846366275, 46.81081390833239197, -13.79151199599547439 ) ) ;
#949 = CARTESIAN_POINT ( 'NONE',  ( -87.04503123322959368, 18.12276621389070286, -11.46092073712416060 ) ) ;
#951 = CARTESIAN_POINT ( 'NONE',  ( -362.0709805440841365, -4.857225732735059864E-14, 0.000000000000000000 ) ) ;
#952 = CARTESIAN_POINT ( 'NONE',  ( -100.7734535825088500, 22.67402823373189946, 40.00000000000002132 ) ) ;
#953 =( NAMED_UNIT ( * ) PLANE_ANGLE_UNIT ( ) SI_UNIT ( $, .RADIAN. ) );
#954 = CARTESIAN_POINT ( 'NONE',  ( -114.7539998840377962, 2.778767434142399573, -21.97438023164994192 ) ) ;
#955 = CARTESIAN_POINT ( 'NONE',  ( 0.000000000000000000, 0.000000000000000000, 0.000000000000000000 ) ) ;
#956 = EDGE_LOOP ( 'NONE', ( #1715, #1989, #25855, #13026 ) ) ;
#957 = ORIENTED_EDGE ( 'NONE', *, *, #6304, .F. ) ;
#958 = CIRCLE ( 'NONE', #7716, 5.000000000000011546 ) ;
#959 = CARTESIAN_POINT ( 'NONE',  ( 35.93675087521947376, -12.87543817712692729, 42.26938917674299034 ) ) ;
#960 = CARTESIAN_POINT ( 'NONE',  ( 132.4338126186515581, 12.33615677966353452, -29.78211700502412285 ) ) ;
#961 = VERTEX_POINT ( 'NONE', #7078 ) ;
#962 = ORIENTED_EDGE ( 'NONE', *, *, #25597, .T. ) ;
#963 = CARTESIAN_POINT ( 'NONE',  ( 199.0254590212676078, -18.72437106667806717, 7.049340093992902290 ) ) ;
#964 = DIRECTION ( 'NONE',  ( -1.000000000000000000, -1.836970198721030427E-16, 0.000000000000000000 ) ) ;
#965 = EDGE_CURVE ( 'NONE', #24679, #18072, #13200, .T. ) ;
#966 = CARTESIAN_POINT ( 'NONE',  ( -91.56559293963834989, -44.31723036834903695, 12.25131212657476709 ) ) ;
#967 = CARTESIAN_POINT ( 'NONE',  ( 130.8568914410475372, -24.07718906447222551, -24.07718906447233209 ) ) ;
#968 = CARTESIAN_POINT ( 'NONE',  ( -208.1127848780264742, 39.99999999999979394, 55.00245453010936103 ) ) ;
#969 = CARTESIAN_POINT ( 'NONE',  ( -199.9999999999999432, -45.65206365911544850, 19.98641303047035223 ) ) ;
#970 = EDGE_CURVE ( 'NONE', #17072, #2955, #7897, .T. ) ;
#971 = DIRECTION ( 'NONE',  ( -1.836970198721030181E-16, 1.000000000000000000, 0.000000000000000000 ) ) ;
#972 = CARTESIAN_POINT ( 'NONE',  ( -238.4067589809705794, -39.99999999999963762, -40.96449428006383187 ) ) ;
#973 = CARTESIAN_POINT ( 'NONE',  ( -100.7734535825088500, 40.00000000000017764, -17.32597176626768487 ) ) ;
#974 = DIRECTION ( 'NONE',  ( 0.9352143323239811012, 0.1355013636757285422, 0.3271292299043733198 ) ) ;
#975 = CARTESIAN_POINT ( 'NONE',  ( -200.0000000000000284, 19.96680831879919538, -45.63305559644798137 ) ) ;
#976 = CARTESIAN_POINT ( 'NONE',  ( 192.4448373802100889, 14.14213562375893574, -14.14213562375874922 ) ) ;
#977 = CARTESIAN_POINT ( 'NONE',  ( -88.39148973765020401, 8.027153355909049992, 20.15708830332377133 ) ) ;
#978 = LINE ( 'NONE', #16933, #23009 ) ;
#979 = DIRECTION ( 'NONE',  ( 1.000000000000000000, -0.000000000000000000, -0.000000000000000000 ) ) ;
#980 = FACE_OUTER_BOUND ( 'NONE', #4167, .T. ) ;
#981 = CARTESIAN_POINT ( 'NONE',  ( -91.56559293963834989, -40.53558337403692491, 16.03295912088671571 ) ) ;
#982 = CARTESIAN_POINT ( 'NONE',  ( -184.9730489278823882, -22.80026000644736328, -42.02334742172997295 ) ) ;
#983 = DIRECTION ( 'NONE',  ( 1.000000000000000000, 1.836970198721030427E-16, -0.000000000000000000 ) ) ;
#984 = ORIENTED_EDGE ( 'NONE', *, *, #22744, .T. ) ;
#985 = CARTESIAN_POINT ( 'NONE',  ( 170.2234770963711128, 10.92277846919147066, 45.64576402573197811 ) ) ;
#986 = CARTESIAN_POINT ( 'NONE',  ( 23.37394308801977871, -23.33966569535098046, 42.85717664514577763 ) ) ;
#987 = CARTESIAN_POINT ( 'NONE',  ( -608.3670141342350917, 33.85940881687466231, 29.64264663930133992 ) ) ;
#988 = ORIENTED_EDGE ( 'NONE', *, *, #20698, .F. ) ;
#989 = CARTESIAN_POINT ( 'NONE',  ( 130.8568914410475088, -39.99999999999992895, -5.949712681207114606 ) ) ;
#990 = CARTESIAN_POINT ( 'NONE',  ( 199.0112255263369718, -6.317613805557628304, -18.97682060292212114 ) ) ;
#991 = CARTESIAN_POINT ( 'NONE',  ( -199.9999999999999432, 4.865628651907057289, -55.16984130226895644 ) ) ;
#992 = VERTEX_POINT ( 'NONE', #2965 ) ;
#993 = VERTEX_POINT ( 'NONE', #19060 ) ;
#994 = ORIENTED_EDGE ( 'NONE', *, *, #17258, .F. ) ;
#995 = CARTESIAN_POINT ( 'NONE',  ( -238.4067589809705794, 40.96449428006337001, -40.00000000000002132 ) ) ;
#996 = DIRECTION ( 'NONE',  ( 0.000000000000000000, 0.000000000000000000, -1.000000000000000000 ) ) ;
#997 = B_SPLINE_CURVE_WITH_KNOTS ( 'NONE', 3,
 ( #7874, #1158, #13256, #1778, #9883, #26275, #12144, #15374, #24123, #5894, #14002, #10153, #20132, #21379, #25380, #22132, #21504, #3150, #7132, #15244, #23376, #12012, #5151, #11252, #19371, #3275, #9262, #17369, #25506, #7256, #23497, #579, #24530, #10410, #22405, #22927, #2713, #20665, #8149, #4438, #8686, #2301, #309, #6681, #170, #8411, #2177, #6159, #2573, #4708, #16264, #6418, #445, #4315, #24393, #16795, #12812, #18527, #12672, #18658, #4181, #16533, #18393, #8548, #14796, #10547, #6286, #12276, #20934, #24661, #14268, #18798, #14535, #22666 ),
 .UNSPECIFIED., .F., .F.,
 ( 4, 2, 2, 2, 2, 2, 2, 2, 2, 2, 2, 2, 2, 2, 2, 2, 2, 2, 2, 2, 2, 2, 2, 2, 2, 2, 2, 2, 2, 2, 2, 2, 2, 2, 2, 2, 4 ),
 ( 0.09798846907125773054, 0.09951654375267081354, 0.1010446184340838827, 0.1041007677969100348, 0.1071569171597361869, 0.1102130665225623529, 0.1132692158853885050, 0.1163253652482146572, 0.1224376639738672112, 0.1239657386552804053, 0.1254938133366935993, 0.1285499626995199873, 0.1346622614251727357, 0.1361903361065859297, 0.1377184107879991515, 0.1407745601508255950, 0.1438307095136520108, 0.1453587841950652049, 0.1468868588764783989, 0.1529991576021312305, 0.1545272322835444245, 0.1560553069649576186, 0.1591114563277840066, 0.1606395310091972561, 0.1621676056906105057, 0.1652237550534370325, 0.1682799044162635593, 0.1698079790976768089, 0.1713360537790900584, 0.1774483525047432786, 0.1805045018675699997, 0.1820325765489833603, 0.1835606512303967208, 0.1896729499560510512, 0.1927290993188783552, 0.1942571740002920211, 0.1957852486817056592 ),
 .UNSPECIFIED. ) ;
#998 = CARTESIAN_POINT ( 'NONE',  ( -77.58523997990643295, -17.50224656896021003, 13.57278374160384260 ) ) ;
#999 = CARTESIAN_POINT ( 'NONE',  ( -208.1127848780265026, -9.061048840815752106E-14, 15.00245453012669472 ) ) ;
#1000 = CARTESIAN_POINT ( 'NONE',  ( 199.9999999999999147, -10.82539530975288855, -15.62049148088690131 ) ) ;
#1001 = DIRECTION ( 'NONE',  ( -1.000000000000000000, 0.000000000000000000, 0.000000000000000000 ) ) ;
#1002 = CARTESIAN_POINT ( 'NONE',  ( 170.2234770963711128, -17.36149277827010096, 17.36149277826970660 ) ) ;
#1003 = CARTESIAN_POINT ( 'NONE',  ( -626.9846540392142060, 90.00000000000000000, 0.000000000000000000 ) ) ;
#1004 = LINE ( 'NONE', #19348, #9721 ) ;
#1005 = CARTESIAN_POINT ( 'NONE',  ( -238.4067589809705794, 3.877349844572403567E-13, -40.96449427998260973 ) ) ;
#1006 = CARTESIAN_POINT ( 'NONE',  ( -99.29480781227053399, -8.165122821357890359, 20.80016781325164388 ) ) ;
#1007 = CARTESIAN_POINT ( 'NONE',  ( 146.6084372240433709, 34.62501878078307982, -40.00000000000002132 ) ) ;
#1008 = CARTESIAN_POINT ( 'NONE',  ( -162.0762913951020892, -29.48230308784785692, 29.48230308784751230 ) ) ;
#1009 = CARTESIAN_POINT ( 'NONE',  ( 0.2972598230769983307, -14.33493731733933352, 0.000000000000000000 ) ) ;
#1011 = CARTESIAN_POINT ( 'NONE',  ( 14.38125909742180220, 39.99999999999997158, 15.17850393972647716 ) ) ;
#1010 = CARTESIAN_POINT ( 'NONE',  ( -213.1075012329537230, 9.698598906450543566, -9.698598906450348167 ) ) ;
#1012 = CARTESIAN_POINT ( 'NONE',  ( 163.1118516004056573, -27.26290988616869626, 0.000000000000000000 ) ) ;
#1013 = CARTESIAN_POINT ( 'NONE',  ( -208.1127848780264742, -17.67593391476659548, 38.89260858015730804 ) ) ;
#1014 = CARTESIAN_POINT ( 'NONE',  ( -280.0000000000000568, -20.00000000000006750, 40.00000000000002132 ) ) ;
#1015 = ORIENTED_EDGE ( 'NONE', *, *, #8422, .F. ) ;
#1016 = ADVANCED_FACE ( 'NONE', ( #17315 ), #3265, .T. ) ;
#1017 = CARTESIAN_POINT ( 'NONE',  ( 5.823571940253325252, -49.16771748718758062, 14.15488761397359418 ) ) ;
#1018 = CARTESIAN_POINT ( 'NONE',  ( -91.56559293963834989, 17.32597176626809699, -40.00000000000002132 ) ) ;
#1019 = DIRECTION ( 'NONE',  ( -1.000000000000000000, 1.836970198721030181E-16, 0.000000000000000000 ) ) ;
#1020 = EDGE_CURVE ( 'NONE', #4727, #14641, #4162, .T. ) ;
#1021 = CARTESIAN_POINT ( 'NONE',  ( -238.4067589809705794, 0.6820004457340470561, 57.25054294065803617 ) ) ;
#1022 = CARTESIAN_POINT ( 'NONE',  ( 192.4448373802100889, 1.051811698935164031E-13, -20.00000000003942091 ) ) ;
#1023 = CARTESIAN_POINT ( 'NONE',  ( -82.25099254137421667, 19.89874485163253581, 3.429530458953132133 ) ) ;
#1024 = EDGE_CURVE ( 'NONE', #19288, #5841, #13481, .T. ) ;
#1025 = EDGE_CURVE ( 'NONE', #20774, #23054, #12596, .T. ) ;
#1026 = CARTESIAN_POINT ( 'NONE',  ( -3.071327051952971399, -13.87830843099562728, -47.32824404903816173 ) ) ;
#1027 = CARTESIAN_POINT ( 'NONE',  ( 199.9999999999999716, 2.158921371974932057, 18.88613560767030464 ) ) ;
#1028 = CARTESIAN_POINT ( 'NONE',  ( 200.0000000000000000, 14.14213562373041455, 42.42640687119311593 ) ) ;
#1029 = CARTESIAN_POINT ( 'NONE',  ( -82.25678930352327711, -4.084640388374164210, -19.77202877180203089 ) ) ;
#1030 = CARTESIAN_POINT ( 'NONE',  ( 160.7895100360958622, -28.48799984206438296, 0.000000000000000000 ) ) ;
#1031 = CARTESIAN_POINT ( 'NONE',  ( 199.9999999999999432, -1.727494763561684666E-13, 20.00000000000010303 ) ) ;
#1032 = CARTESIAN_POINT ( 'NONE',  ( -198.0356074513804572, 17.40982414986446969, 39.15871834505921356 ) ) ;
#1033 = CARTESIAN_POINT ( 'NONE',  ( -82.24857225179439979, 11.87278284862390976, -16.34324723835692694 ) ) ;
#1034 = CARTESIAN_POINT ( 'NONE',  ( -105.3755690713226727, 15.38646221621771737, 15.38646221621800514 ) ) ;
#1036 = CARTESIAN_POINT ( 'NONE',  ( 163.1118516004056573, -47.56205970284945295, -9.006482792074823607 ) ) ;
#1035 = CARTESIAN_POINT ( 'NONE',  ( -198.9233928135151928, 14.16707757974149828, -49.24835219441582979 ) ) ;
#1037 = CARTESIAN_POINT ( 'NONE',  ( 19.06497207195981147, 38.31983398719673772, -38.31983398719579981 ) ) ;
#1038 = CARTESIAN_POINT ( 'NONE',  ( -86.96347745069644475, -21.75974354311652093, -40.00000000000002132 ) ) ;
#1039 = CARTESIAN_POINT ( 'NONE',  ( -192.9588430854689989, 10.23066800230742679, 10.23066800230749607 ) ) ;
#1040 = CARTESIAN_POINT ( 'NONE',  ( -198.0356074513804572, -9.007331120208026888E-14, 15.37879056873070560 ) ) ;
#1041 = CARTESIAN_POINT ( 'NONE',  ( -100.7734535825088500, -40.53558337403692491, 16.03295912088671571 ) ) ;
#1042 = CARTESIAN_POINT ( 'NONE',  ( -144.1957000271909806, 30.13184844835543075, -12.48102028634719396 ) ) ;
#1043 = ORIENTED_EDGE ( 'NONE', *, *, #3287, .F. ) ;
#1044 = CARTESIAN_POINT ( 'NONE',  ( 146.6084372240433993, 3.800685668858676980, 3.800685668858667210 ) ) ;
#1045 = ADVANCED_FACE ( 'NONE', ( #24084, #5858, #5998, #13964, #22099, #22760, #8115, #10649 ), #20625, .F. ) ;
#1046 = CARTESIAN_POINT ( 'NONE',  ( -4.039451493210490796, 46.99046209229823745, -13.82811171175438147 ) ) ;
#1047 = CARTESIAN_POINT ( 'NONE',  ( 17.24092899311760263, 18.36647614518702198, 44.34059580268282730 ) ) ;
#1048 = CARTESIAN_POINT ( 'NONE',  ( -62.69292774209023378, -24.97541154601726632, -11.76166271901563576 ) ) ;
#1049 = ORIENTED_EDGE ( 'NONE', *, *, #22501, .T. ) ;
#1050 = CARTESIAN_POINT ( 'NONE',  ( -173.7925187075031204, -38.69492115326026038, 20.60915802515858886 ) ) ;
#1051 = CARTESIAN_POINT ( 'NONE',  ( 200.0000000000000568, 2.475862818518347552, -18.83975305017670365 ) ) ;
#1052 = CARTESIAN_POINT ( 'NONE',  ( 23.84827734669584487, -23.24317830786080208, 42.71123329578262684 ) ) ;
#1053 = ADVANCED_FACE ( 'NONE', ( #2269 ), #2400, .T. ) ;
#1054 = CARTESIAN_POINT ( 'NONE',  ( 98.29820294267322822, 7.653668647304298744, -18.47759065023114999 ) ) ;
#1055 = CARTESIAN_POINT ( 'NONE',  ( 199.0190933210857906, 9.274233341078666371, 17.72222919763310856 ) ) ;
#1056 = CARTESIAN_POINT ( 'NONE',  ( -259.2033419157646676, -21.55415060305872998, 35.01439189186525880 ) ) ;
#1057 = CARTESIAN_POINT ( 'NONE',  ( 0.2972598230769883387, 39.99999999999997158, 14.33493731733947563 ) ) ;
#1058 = CARTESIAN_POINT ( 'NONE',  ( 130.8568914410475372, 1.429239637432775288E-13, -34.05028731879788495 ) ) ;
#1059 = LINE ( 'NONE', #1190, #21088 ) ;
#1060 = CARTESIAN_POINT ( 'NONE',  ( -259.2033419157646676, -30.48217210827744239, -2.449293598294708485E-15 ) ) ;
#1062 = CARTESIAN_POINT ( 'NONE',  ( -86.96347745069644475, 15.38646221621793586, -15.38646221621778842 ) ) ;
#1061 = CARTESIAN_POINT ( 'NONE',  ( 27.55177309528516361, -13.49150912998400287, -45.29548561696848452 ) ) ;
#1063 = CARTESIAN_POINT ( 'NONE',  ( -162.0762913951020607, -41.69427287692683848, 40.00000000000002132 ) ) ;
#1064 = CARTESIAN_POINT ( 'NONE',  ( 184.8905102610680444, 43.07788698682572459, 13.49065550809829439 ) ) ;
#1065 = CARTESIAN_POINT ( 'NONE',  ( -192.9588430854690273, 40.00000000000055422, -54.46834944101679810 ) ) ;
#1066 = DIRECTION ( 'NONE',  ( 1.000000000000000000, 1.836970198721030181E-16, 0.000000000000000000 ) ) ;
#1067 = CARTESIAN_POINT ( 'NONE',  ( -280.0000000000000568, -39.99999999999987210, -20.00000000000043343 ) ) ;
#1068 = CARTESIAN_POINT ( 'NONE',  ( 144.1614306663417722, -30.21666801910898315, -12.51615370324033272 ) ) ;
#1069 = CARTESIAN_POINT ( 'NONE',  ( 0.2972598230769938343, 10.13633138497486286, -10.13633138497461594 ) ) ;
#1070 = CARTESIAN_POINT ( 'NONE',  ( 146.6084372240433709, 24.48358557860311180, 32.08495691632071356 ) ) ;
#1071 = ORIENTED_EDGE ( 'NONE', *, *, #14110, .F. ) ;
#1073 = CARTESIAN_POINT ( 'NONE',  ( 12.96694272559474648, 44.79869582453754617, -24.77464205076245207 ) ) ;
#1072 = CARTESIAN_POINT ( 'NONE',  ( -86.86493150571116928, 19.60045294882758071, -8.366608963953975575 ) ) ;
#1074 = CARTESIAN_POINT ( 'NONE',  ( -198.0356074513804572, -15.37879056873074290, 40.00000000000002132 ) ) ;
#1075 = PRESENTATION_STYLE_ASSIGNMENT (( #9557 ) ) ;
#1076 = DIRECTION ( 'NONE',  ( -1.303213150798907793E-16, 1.000000000000000000, -1.682156097916904081E-16 ) ) ;
#1077 = DIRECTION ( 'NONE',  ( -1.000000000000000000, 0.000000000000000000, 0.000000000000000000 ) ) ;
#1078 = VERTEX_POINT ( 'NONE', #6512 ) ;
#1079 = ORIENTED_EDGE ( 'NONE', *, *, #14192, .F. ) ;
#1080 = CARTESIAN_POINT ( 'NONE',  ( -105.3755690713226727, 15.38646221621793231, -15.38646221621779020 ) ) ;
#1081 = DIRECTION ( 'NONE',  ( -1.836970198721030427E-16, 1.000000000000000000, -1.321694076934715579E-16 ) ) ;
#1082 = CARTESIAN_POINT ( 'NONE',  ( 165.3321726438082351, 1.230175059844345975E-13, -26.53500608755492252 ) ) ;
#1083 = ORIENTED_EDGE ( 'NONE', *, *, #23767, .F. ) ;
#1084 = CARTESIAN_POINT ( 'NONE',  ( 200.0000000000000568, 3.396018298074437780, 18.70303282425911462 ) ) ;
#1085 = CIRCLE ( 'NONE', #21901, 5.000000000000004441 ) ;
#1086 = VECTOR ( 'NONE', #8418, 1000.000000000000000 ) ;
#1087 = CARTESIAN_POINT ( 'NONE',  ( -716.9846540392142060, 66.50000000000009948, -61.50000000000004974 ) ) ;
#1088 = CARTESIAN_POINT ( 'NONE',  ( 136.1360204305621551, -53.05693388239313890, 3.511608612530593199 ) ) ;
#1089 = CARTESIAN_POINT ( 'NONE',  ( -626.9846540392142060, 75.00000000000000000, -54.99999999999995026 ) ) ;
#1090 = CARTESIAN_POINT ( 'NONE',  ( 146.6084372240433993, 1.478241399363601114E-13, -34.62501878078305850 ) ) ;
#1091 = DIRECTION ( 'NONE',  ( -1.000000000000000000, -1.836970198721030181E-16, -0.000000000000000000 ) ) ;
#1092 = CARTESIAN_POINT ( 'NONE',  ( 130.8568914410475088, -40.00000000000036238, 34.05028731879746573 ) ) ;
#1093 = CARTESIAN_POINT ( 'NONE',  ( 57.59792236341147742, 4.064940816252731242E-13, -37.56421063658186199 ) ) ;
#1094 = DIRECTION ( 'NONE',  ( 0.000000000000000000, 0.000000000000000000, 1.000000000000000000 ) ) ;
#1095 = CARTESIAN_POINT ( 'NONE',  ( -280.0000000000000568, -42.42640687119285303, -14.14213562373118371 ) ) ;
#1096 = CARTESIAN_POINT ( 'NONE',  ( -77.90255099906767100, 8.064892378658102601, -20.29001641120677846 ) ) ;
#1097 = CARTESIAN_POINT ( 'NONE',  ( -213.1075012329537230, -9.698598906450557777, 9.698598906450415669 ) ) ;
#1098 = CARTESIAN_POINT ( 'NONE',  ( 126.3230993689412571, 28.30579214049041070, 11.72464299830500067 ) ) ;
#1099 = CARTESIAN_POINT ( 'NONE',  ( 199.9999999999999716, 82.50000000000008527, 52.49999999999977973 ) ) ;
#1100 = CARTESIAN_POINT ( 'NONE',  ( 0.000000000000000000, 0.000000000000000000, 0.000000000000000000 ) ) ;
#1101 = CARTESIAN_POINT ( 'NONE',  ( -77.58512834293978244, -17.50146741023962349, 13.57440574222109397 ) ) ;
#1102 = CARTESIAN_POINT ( 'NONE',  ( 192.4448373802101173, -14.14213562375886291, 42.42640687116498555 ) ) ;
#1103 = AXIS2_PLACEMENT_3D ( 'NONE', #2737, #10842, #13228 ) ;
#1104 = AXIS2_PLACEMENT_3D ( 'NONE', #14806, #22938, #4718 ) ;
#1105 = CARTESIAN_POINT ( 'NONE',  ( -259.2033419157646676, -49.83842185052040463, 6.730120644403092101 ) ) ;
#1106 = CARTESIAN_POINT ( 'NONE',  ( -187.8779108535657372, -17.82355704115960648, -43.02987313851341611 ) ) ;
#1107 = CARTESIAN_POINT ( 'NONE',  ( -626.9846540392142060, 75.00000000000000000, -65.00000000000004263 ) ) ;
#1108 = EDGE_LOOP ( 'NONE', ( #7564, #21544, #5228, #9146 ) ) ;
#1109 = CARTESIAN_POINT ( 'NONE',  ( -30.26275506840324070, 1.198031551616724366, -57.76657404653984429 ) ) ;
#1110 = DIRECTION ( 'NONE',  ( 1.000000000000000000, 1.836970198721030181E-16, 0.000000000000000000 ) ) ;
#1111 = CARTESIAN_POINT ( 'NONE',  ( 169.9999999999674571, -17.64300463372919836, -17.64300463252165585 ) ) ;
#1112 = PRODUCT_DEFINITION ( 'UNKNOWN', '', #12139, #15344 ) ;
#1113 = ORIENTED_EDGE ( 'NONE', *, *, #21755, .F. ) ;
#1114 = CARTESIAN_POINT ( 'NONE',  ( -56.48582580120559271, -1.062504017861011783E-13, 9.153146818113587102 ) ) ;
#1115 = CARTESIAN_POINT ( 'NONE',  ( -3.555049149807529396, -23.55301256057176573, 43.14507846637736321 ) ) ;
#1116 = CYLINDRICAL_SURFACE ( 'NONE', #8150, 44.99999999999997158 ) ;
#1117 = CIRCLE ( 'NONE', #11762, 60.00000000000000000 ) ;
#1118 = EDGE_LOOP ( 'NONE', ( #10707, #11181, #17708, #25036 ) ) ;
#1119 = ORIENTED_EDGE ( 'NONE', *, *, #1862, .F. ) ;
#1120 = CARTESIAN_POINT ( 'NONE',  ( 170.2234770963711128, 15.44714144992819094, 2.449293598294708485E-15 ) ) ;
#1121 = PRODUCT_DEFINITION_CONTEXT ( 'detailed design', #16139, 'design' ) ;
#1122 = CARTESIAN_POINT ( 'NONE',  ( -265.0000000000000000, -4.867971026610730343E-14, -6.532754371361504014E-30 ) ) ;
#1123 = CIRCLE ( 'NONE', #20660, 39.99999999999997158 ) ;
#1124 = CARTESIAN_POINT ( 'NONE',  ( -56.48582580120559271, 6.472252184284211118, -6.472252184284153387 ) ) ;
#1125 = CARTESIAN_POINT ( 'NONE',  ( -86.96347745069645896, 40.00000000000008527, -21.75974354311636461 ) ) ;
#1126 = EDGE_CURVE ( 'NONE', #8002, #9153, #408, .T. ) ;
#1127 = DIRECTION ( 'NONE',  ( -1.000000000000000000, -1.836970198721030181E-16, -0.000000000000000000 ) ) ;
#1128 = ADVANCED_FACE ( 'NONE', ( #14498 ), #20591, .T. ) ;
#1129 = AXIS2_PLACEMENT_3D ( 'NONE', #12944, #974, #3215 ) ;
#1130 = CARTESIAN_POINT ( 'NONE',  ( -199.9999999999999432, 43.68705981750494516, 18.09577267661451927 ) ) ;
#1131 = CARTESIAN_POINT ( 'NONE',  ( -100.7734535825088358, 6.065416334915073333E-14, -22.67402823373191723 ) ) ;
#1132 = CARTESIAN_POINT ( 'NONE',  ( 199.9999999999994031, -18.37269623729978107, -4.912321869774860517 ) ) ;
#1133 = AXIS2_PLACEMENT_3D ( 'NONE', #3305, #1186, #21785 ) ;
#1134 = DIRECTION ( 'NONE',  ( 1.000000000000000000, -1.836970198721030181E-16, -0.000000000000000000 ) ) ;
#1135 = CARTESIAN_POINT ( 'NONE',  ( -24.88648382749666155, -19.35593139216429037, -36.77569126519823328 ) ) ;
#1136 = CARTESIAN_POINT ( 'NONE',  ( -238.4067589809705794, -0.6820004457337348613, -57.25054294065803617 ) ) ;
#1137 = CARTESIAN_POINT ( 'NONE',  ( -97.74230697482651919, 20.71358501227901883, 8.579847837454130044 ) ) ;
#1138 = CARTESIAN_POINT ( 'NONE',  ( -238.4067589809705794, -39.99999999999963762, -40.96449428006383187 ) ) ;
#1139 = LINE ( 'NONE', #17860, #8300 ) ;
#1140 = CARTESIAN_POINT ( 'NONE',  ( 146.6084372240433709, -5.374981219216942385, -40.00000000000002132 ) ) ;
#1141 = CARTESIAN_POINT ( 'NONE',  ( -30.26275506840325136, 27.08623969584573388, 29.48230279907808793 ) ) ;
#1142 = CARTESIAN_POINT ( 'NONE',  ( 151.7948205124835681, 33.23291073765556547, -40.00000000000002132 ) ) ;
#1144 = CARTESIAN_POINT ( 'NONE',  ( 170.2234770963711128, 40.00000000000014211, -24.55285855007172913 ) ) ;
#1143 = CARTESIAN_POINT ( 'NONE',  ( 98.29820294272737158, 10.21753654889138652, 17.41560179325824009 ) ) ;
#1145 = AXIS2_PLACEMENT_3D ( 'NONE', #16360, #16231, #22372 ) ;
#1146 = LINE ( 'NONE', #13362, #1967 ) ;
#1147 = CARTESIAN_POINT ( 'NONE',  ( -105.3755690713226727, 12.89780903124400879, 12.89780903124407452 ) ) ;
#1148 = CARTESIAN_POINT ( 'NONE',  ( 4.995406935893288214, 55.24977328854835434, 2.449293598294708485E-15 ) ) ;
#1149 = ORIENTED_EDGE ( 'NONE', *, *, #9291, .F. ) ;
#1150 = CARTESIAN_POINT ( 'NONE',  ( 23.17367289775286210, -42.91822977676378770, 23.38495170326197226 ) ) ;
#1151 = CARTESIAN_POINT ( 'NONE',  ( -105.4741150117365009, 19.60045294981777531, -8.366608964619008049 ) ) ;
#1152 = CIRCLE ( 'NONE', #8804, 29.99999999999999289 ) ;
#1153 = CARTESIAN_POINT ( 'NONE',  ( -192.9588430854689989, 38.51493924976929861, 38.51493924976947625 ) ) ;
#1154 = CARTESIAN_POINT ( 'NONE',  ( -259.2033419157646676, -1.438356298054549103E-14, -9.517827891722632216 ) ) ;
#1155 = CARTESIAN_POINT ( 'NONE',  ( -77.55800104386271698, 22.12266577817424817, 0.9110312510734462910 ) ) ;
#1156 = CARTESIAN_POINT ( 'NONE',  ( 20.59573805978978811, -13.93986955483911849, -47.74081960064690833 ) ) ;
#1157 = CARTESIAN_POINT ( 'NONE',  ( 200.0000000000003695, 4.006257452897062699, 18.58368358710308144 ) ) ;
#1158 = CARTESIAN_POINT ( 'NONE',  ( -627.5027443299393326, 26.45751311064577038, -30.00000000000005329 ) ) ;
#1159 = CARTESIAN_POINT ( 'NONE',  ( -82.23866184897889298, 1.260276691160380436, -20.16530832601847933 ) ) ;
#1160 = CARTESIAN_POINT ( 'NONE',  ( -192.9588430854690273, 38.51493924976913519, 18.05360324515490333 ) ) ;
#1161 = CARTESIAN_POINT ( 'NONE',  ( 192.4448373802101173, 14.14213562375922884, -42.42640687116488607 ) ) ;
#1162 = EDGE_CURVE ( 'NONE', #1634, #13223, #20018, .T. ) ;
#1163 = CARTESIAN_POINT ( 'NONE',  ( 91.82158438592156813, 40.45024623143950038, 16.11829626348447420 ) ) ;
#1164 = CARTESIAN_POINT ( 'NONE',  ( 160.9163046357249129, -135.7889608577475542, -61.61140153332246427 ) ) ;
#1165 = CARTESIAN_POINT ( 'NONE',  ( -280.0000000000000568, 14.14213562373127431, -42.42640687119274645 ) ) ;
#1167 = CARTESIAN_POINT ( 'NONE',  ( -91.56559293963834989, -16.03295912088659492, -40.53558337403696044 ) ) ;
#1166 = CARTESIAN_POINT ( 'NONE',  ( 0.2972598230770048811, -10.13633138497415942, -66.70487387989865624 ) ) ;
#1168 = CARTESIAN_POINT ( 'NONE',  ( 163.1118516004056573, 37.29075403953132906, 19.27778845539275565 ) ) ;
#1169 = CARTESIAN_POINT ( 'NONE',  ( 130.8568914410475088, -34.05028731879786363, -40.00000000000002132 ) ) ;
#1170 = CARTESIAN_POINT ( 'NONE',  ( 130.8568914410475372, 34.05028731879791337, 0.000000000000000000 ) ) ;
#1171 = VECTOR ( 'NONE', #14693, 1000.000000000000114 ) ;
#1172 = CARTESIAN_POINT ( 'NONE',  ( -189.9999999999999716, 82.50000000000008527, -52.49999999999977973 ) ) ;
#1173 = CARTESIAN_POINT ( 'NONE',  ( 0.2972598230770153171, -66.70487387989849992, -10.13633138497533004 ) ) ;
#1174 = CARTESIAN_POINT ( 'NONE',  ( -173.7925187078953115, 41.93431653924884017, -12.78856575083363722 ) ) ;
#1175 = ORIENTED_EDGE ( 'NONE', *, *, #25415, .F. ) ;
#1176 = CARTESIAN_POINT ( 'NONE',  ( 136.1360204305621551, 31.79587985999267374, -24.77266263493117293 ) ) ;
#1177 = LINE ( 'NONE', #21004, #23952 ) ;
#1178 = CARTESIAN_POINT ( 'NONE',  ( 23.17367289775146943, 23.38495170326214989, 42.91822977676415718 ) ) ;
#1179 = CARTESIAN_POINT ( 'NONE',  ( -87.08870976744167081, -21.20092391029482926, 3.405966936733633155 ) ) ;
#1180 = VERTEX_POINT ( 'NONE', #10214 ) ;
#1181 = CARTESIAN_POINT ( 'NONE',  ( -105.2527671768314548, 17.45248019613228863, 12.50784186996179059 ) ) ;
#1182 = CARTESIAN_POINT ( 'NONE',  ( 199.9999999999999147, -13.00175152101318510, -13.87559618198639022 ) ) ;
#1183 = CARTESIAN_POINT ( 'NONE',  ( 22.92196489052106401, -23.44087486047334323, 42.99364193793560673 ) ) ;
#1184 = CARTESIAN_POINT ( 'NONE',  ( 0.000000000000000000, 0.000000000000000000, 0.000000000000000000 ) ) ;
#1185 = CARTESIAN_POINT ( 'NONE',  ( 199.0075387591496110, 2.605640672139595715, -19.82598477556707195 ) ) ;
#1186 = DIRECTION ( 'NONE',  ( 1.000000000000000000, 1.836970198721025990E-16, 0.000000000000000000 ) ) ;
#1187 = CARTESIAN_POINT ( 'NONE',  ( -192.9588430854690273, 39.99999999999992895, 14.46834944099983922 ) ) ;
#1188 = DIRECTION ( 'NONE',  ( 1.000000000000000000, -0.000000000000000000, -0.000000000000000000 ) ) ;
#1189 = EDGE_CURVE ( 'NONE', #23238, #6963, #17697, .T. ) ;
#1190 = CARTESIAN_POINT ( 'NONE',  ( 160.9163046357249129, -205.7889608577475542, 61.61140153332252112 ) ) ;
#1191 = CARTESIAN_POINT ( 'NONE',  ( -135.8532207217289738, -30.84685318188647685, -2.449293598294708485E-15 ) ) ;
#1193 = CARTESIAN_POINT ( 'NONE',  ( -598.6670741908344553, 38.75362502970266121, -9.956152867874221712 ) ) ;
#1192 = CARTESIAN_POINT ( 'NONE',  ( 60.14720761601253685, -15.75494750867305704, -31.22869220293659609 ) ) ;
#1194 = EDGE_CURVE ( 'NONE', #8799, #7462, #15578, .T. ) ;
#1195 = CARTESIAN_POINT ( 'NONE',  ( 136.1360204305621551, -4.966164525587043244, 40.00000000000002132 ) ) ;
#1196 = FACE_OUTER_BOUND ( 'NONE', #11209, .T. ) ;
#1197 = CARTESIAN_POINT ( 'NONE',  ( 136.1360204305621551, 40.00000000000009948, -4.966164525586641787 ) ) ;
#1198 = CARTESIAN_POINT ( 'NONE',  ( 170.2234770963711128, -40.00000000000024158, 24.55285855007145202 ) ) ;
#1199 = CARTESIAN_POINT ( 'NONE',  ( 156.5534228368365177, -27.23630265682181673, -11.28164594935398668 ) ) ;
#1200 = EDGE_CURVE ( 'NONE', #17385, #7220, #19400, .T. ) ;
#1201 = EDGE_CURVE ( 'NONE', #20449, #5206, #6685, .T. ) ;
#1202 = ORIENTED_EDGE ( 'NONE', *, *, #1431, .T. ) ;
#1204 = CARTESIAN_POINT ( 'NONE',  ( -4.027137536849638266, 43.00884733904534585, -23.45200847982327730 ) ) ;
#1203 = FACE_OUTER_BOUND ( 'NONE', #26317, .T. ) ;
#1205 = CARTESIAN_POINT ( 'NONE',  ( -213.1075012329537230, -13.71589010951915810, 40.00000000000002132 ) ) ;
#1206 =( LENGTH_UNIT ( ) NAMED_UNIT ( * ) SI_UNIT ( .MILLI., .METRE. ) );
#1207 = CARTESIAN_POINT ( 'NONE',  ( -192.9370391625991772, 44.11033075278052706, -24.26711063095028109 ) ) ;
#1208 = CARTESIAN_POINT ( 'NONE',  ( 0.000000000000000000, 0.000000000000000000, 0.000000000000000000 ) ) ;
#1209 = VERTEX_POINT ( 'NONE', #25254 ) ;
#1210 = ORIENTED_EDGE ( 'NONE', *, *, #56, .F. ) ;
#1211 = CARTESIAN_POINT ( 'NONE',  ( 146.6084372240433993, 24.48358557860341733, -24.48358557860313311 ) ) ;
#1212 = DIRECTION ( 'NONE',  ( 0.000000000000000000, 1.000000000000000000, 0.000000000000000000 ) ) ;
#1213 = ORIENTED_EDGE ( 'NONE', *, *, #19964, .F. ) ;
#1214 = EDGE_LOOP ( 'NONE', ( #19295, #19332, #11818, #2161, #19742, #15932, #25979, #23174 ) ) ;
#1215 = CARTESIAN_POINT ( 'NONE',  ( 200.0000000000000853, -10.31015863810315025, 15.97237410830284254 ) ) ;
#1216 = CARTESIAN_POINT ( 'NONE',  ( -199.9999999999999432, 14.17215463606929227, 49.28189405767592746 ) ) ;
#1217 = CARTESIAN_POINT ( 'NONE',  ( 57.59792236341147031, 26.56190807104684382, 26.56190807104692553 ) ) ;
#1218 = DIRECTION ( 'NONE',  ( 1.000000000000000000, 1.836970198721030181E-16, -0.000000000000000000 ) ) ;
#1219 = CARTESIAN_POINT ( 'NONE',  ( -100.7734535825088358, 6.065416334915073333E-14, -22.67402823373191723 ) ) ;
#1220 = DIRECTION ( 'NONE',  ( 0.000000000000000000, -1.000000000000000000, 0.000000000000000000 ) ) ;
#1221 = CARTESIAN_POINT ( 'NONE',  ( 98.29820294267867098, 17.44908643998556741, 10.13669746063099275 ) ) ;
#1222 = CARTESIAN_POINT ( 'NONE',  ( -259.2033419157646676, -40.00000000000017053, 9.517827891722212996 ) ) ;
#1223 = CARTESIAN_POINT ( 'NONE',  ( -213.1075012329537230, 5.259461644596141978E-13, -53.71589010951915100 ) ) ;
#1224 = CARTESIAN_POINT ( 'NONE',  ( -110.0904723790854689, -16.34339323353421136, 11.87257855583943922 ) ) ;
#1225 = CARTESIAN_POINT ( 'NONE',  ( -105.3755690713226727, 15.38646221621793231, -15.38646221621779020 ) ) ;
#1226 = CARTESIAN_POINT ( 'NONE',  ( 14.38125909742181108, -5.035366881890652543E-14, 15.17850393972633682 ) ) ;
#1227 = CARTESIAN_POINT ( 'NONE',  ( 19.06497207195981147, -10.03556273973439517, 10.03556273973429214 ) ) ;
#1228 = CARTESIAN_POINT ( 'NONE',  ( 132.4338126186516718, 29.78211700502412995, 12.33615677966351676 ) ) ;
#1229 = VECTOR ( 'NONE', #17312, 999.9999999999998863 ) ;
#1230 = CARTESIAN_POINT ( 'NONE',  ( -77.70896657118139217, 18.93513500903836899, -11.20032855621326995 ) ) ;
#1231 = CARTESIAN_POINT ( 'NONE',  ( 184.8905102610680444, 14.79361573936396113, -14.79361573936377461 ) ) ;
#1232 = CARTESIAN_POINT ( 'NONE',  ( -87.04313178897470493, -18.12206666836609159, 11.44454159255920445 ) ) ;
#1233 = CARTESIAN_POINT ( 'NONE',  ( 136.1360204305621551, -53.05693388239313890, 3.511608612530593199 ) ) ;
#1234 = CARTESIAN_POINT ( 'NONE',  ( -86.96347745069644475, -12.89780903124395195, -12.89780903124416511 ) ) ;
#1235 = CARTESIAN_POINT ( 'NONE',  ( -174.2682069747397975, -16.26528465553820268, -39.26787081120916412 ) ) ;
#1236 = CARTESIAN_POINT ( 'NONE',  ( -77.55640685876514340, 14.66025428152425469, 16.63820105393991611 ) ) ;
#1237 = ORIENTED_EDGE ( 'NONE', *, *, #12981, .F. ) ;
#1238 = CARTESIAN_POINT ( 'NONE',  ( 57.59792236341147031, 54.84617931850878136, 1.722363176415705910 ) ) ;
#1239 = FACE_OUTER_BOUND ( 'NONE', #12293, .T. ) ;
#1240 = CARTESIAN_POINT ( 'NONE',  ( -614.3062485512364219, 30.98201105461428995, 32.64211941558109942 ) ) ;
#1241 = ORIENTED_EDGE ( 'NONE', *, *, #9230, .F. ) ;
#1242 = CARTESIAN_POINT ( 'NONE',  ( 210.0000000000000284, 57.47694228411675255, -64.52066607436459833 ) ) ;
#1243 = CARTESIAN_POINT ( 'NONE',  ( 199.0233014162839140, -20.00325696956714339, -0.1274617848538161236 ) ) ;
#1244 = CARTESIAN_POINT ( 'NONE',  ( 12.01676469546555559, -44.88780742856556571, 24.84032989753427501 ) ) ;
#1245 = EDGE_LOOP ( 'NONE', ( #24383, #1697, #17206, #26322 ) ) ;
#1246 = EDGE_LOOP ( 'NONE', ( #5167, #4784 ) ) ;
#1247 = CARTESIAN_POINT ( 'NONE',  ( -192.9588430854690273, -38.51493924976932703, -18.05360324515463688 ) ) ;
#1248 = CARTESIAN_POINT ( 'NONE',  ( -238.4067589809705794, 39.99999999999997158, 0.9644942799827220803 ) ) ;
#1249 = CARTESIAN_POINT ( 'NONE',  ( -93.01854144614549114, -20.65013722621582914, -8.553566904110464719 ) ) ;
#1250 = CIRCLE ( 'NONE', #4658, 29.99999999999999289 ) ;
#1251 = CARTESIAN_POINT ( 'NONE',  ( 136.1360204305621266, 3.511608612530757068, -3.511608612530642937 ) ) ;
#1252 = CARTESIAN_POINT ( 'NONE',  ( -213.1075012329537230, -40.00000000000011369, 13.71589010951897691 ) ) ;
#1253 = CARTESIAN_POINT ( 'NONE',  ( 199.9999999999998010, -18.94725682776174835, -1.557189005449375330 ) ) ;
#1254 = CARTESIAN_POINT ( 'NONE',  ( -77.70092540962068028, 11.20694785794322179, 18.98758604048486731 ) ) ;
#1255 = CARTESIAN_POINT ( 'NONE',  ( -39.84211263226702471, -13.56589830548555398, -32.75097567531932441 ) ) ;
#1256 = CARTESIAN_POINT ( 'NONE',  ( 170.2234770963711128, 45.64576402573196390, -10.92277846919159856 ) ) ;
#1257 = DIRECTION ( 'NONE',  ( 1.000000000000000000, 0.000000000000000000, 0.000000000000000000 ) ) ;
#1258 = CARTESIAN_POINT ( 'NONE',  ( 170.2234770963711128, 40.00000000000021316, -15.44714144992773797 ) ) ;
#1259 = CARTESIAN_POINT ( 'NONE',  ( 170.0000000000000000, -24.95097643316998415, 3.062538285713072295 ) ) ;
#1260 = CARTESIAN_POINT ( 'NONE',  ( -56.48582580120559271, 9.153146818113576444, -0.000000000000000000 ) ) ;
#1261 = CARTESIAN_POINT ( 'NONE',  ( 192.4448373802100889, 20.00000000003945644, 0.000000000000000000 ) ) ;
#1262 = CARTESIAN_POINT ( 'NONE',  ( 91.82158438592156813, 40.45024623143950038, 16.11829626348447420 ) ) ;
#1263 = CARTESIAN_POINT ( 'NONE',  ( -86.96347745069645896, 21.75974354311648895, -40.00000000000002132 ) ) ;
#1264 = EDGE_CURVE ( 'NONE', #11892, #19940, #5795, .T. ) ;
#1266 = DIRECTION ( 'NONE',  ( -1.000000000000000000, 0.000000000000000000, 0.000000000000000000 ) ) ;
#1265 = CARTESIAN_POINT ( 'NONE',  ( -1.255560987024270991, -43.73013506549190765, -23.98612781107773984 ) ) ;
#1267 = CARTESIAN_POINT ( 'NONE',  ( -105.3755690713226727, -2.472783935621397949E-13, 21.75974354311649961 ) ) ;
#1268 = CARTESIAN_POINT ( 'NONE',  ( 151.7948205124836534, 33.06932595376365924, -23.49921654116018743 ) ) ;
#1269 = CARTESIAN_POINT ( 'NONE',  ( 192.4448373802100889, 19.99999999996064304, 2.449293598294708485E-15 ) ) ;
#1270 = EDGE_LOOP ( 'NONE', ( #6729, #18877, #7061, #15213, #21211, #293, #7924 ) ) ;
#1271 = CARTESIAN_POINT ( 'NONE',  ( 23.46661716383116669, -42.82867125331067371, 23.32081713244396681 ) ) ;
#1272 = CARTESIAN_POINT ( 'NONE',  ( 170.0000000000427178, -17.64300463311358769, 17.64300463311318268 ) ) ;
#1273 = CARTESIAN_POINT ( 'NONE',  ( 151.7948205124836534, -51.78348778862535795, 4.785054706298367044 ) ) ;
#1274 = FACE_OUTER_BOUND ( 'NONE', #4173, .T. ) ;
#1275 = CARTESIAN_POINT ( 'NONE',  ( -77.93819491933658128, 20.10517996227020987, 8.440354353651857267 ) ) ;
#1276 = CARTESIAN_POINT ( 'NONE',  ( 17.75917311731580739, -14.04884443869862487, -48.46615948699207621 ) ) ;
#1277 = CARTESIAN_POINT ( 'NONE',  ( 199.9999999999998295, 8.812783067309094776, 16.84096882534935702 ) ) ;
#1278 = DIRECTION ( 'NONE',  ( 0.000000000000000000, 0.000000000000000000, -1.000000000000000000 ) ) ;
#1279 = FACE_OUTER_BOUND ( 'NONE', #20923, .T. ) ;
#1280 = CARTESIAN_POINT ( 'NONE',  ( -100.7734535825088358, -16.03295912088728770, 16.03295912088687913 ) ) ;
#1281 = CARTESIAN_POINT ( 'NONE',  ( 19.06497207195980792, 18.24870850772790831, -38.31983398719609824 ) ) ;
#1282 = AXIS2_PLACEMENT_3D ( 'NONE', #20, #15834, #6140 ) ;
#1283 = CARTESIAN_POINT ( 'NONE',  ( -77.78698591354267933, -20.89067208891385974, -6.810288896245590529 ) ) ;
#1284 = PLANE ( 'NONE',  #7860 ) ;
#1285 = CARTESIAN_POINT ( 'NONE',  ( -30.26275506840323359, -1.198031551615522439, -57.76657404653986561 ) ) ;
#1287 = CARTESIAN_POINT ( 'NONE',  ( -208.1127848780264742, 10.60833733268383483, -67.17687982760675425 ) ) ;
#1286 = CARTESIAN_POINT ( 'NONE',  ( -259.2033419157646676, -21.55415060305824326, -21.55415060305857367 ) ) ;
#1288 = CARTESIAN_POINT ( 'NONE',  ( -56.48582580120559982, 50.09629031063956717, 6.472252184284792875 ) ) ;
#1289 = CARTESIAN_POINT ( 'NONE',  ( -105.2054292635175017, -14.23158570603253459, 16.16441072137211066 ) ) ;
#1290 = DIRECTION ( 'NONE',  ( -1.000000000000000000, -1.836970198721030427E-16, 0.000000000000000000 ) ) ;
#1291 =( BOUNDED_CURVE ( )  B_SPLINE_CURVE ( 3, ( #7283, #11398, #21403, #15399 ),
 .UNSPECIFIED., .F., .F. ) 
 B_SPLINE_CURVE_WITH_KNOTS ( ( 4, 4 ),
 ( 0.004183487405659152593, 0.01388163287021919670 ),
 .UNSPECIFIED. ) 
 CURVE ( )  GEOMETRIC_REPRESENTATION_ITEM ( )  RATIONAL_B_SPLINE_CURVE ( ( 0.6809743333591533609, 0.7608653435686130173, 0.8672072324488951933, 1.000000000000000000 ) ) 
 REPRESENTATION_ITEM ( '' )  );
#1292 = CARTESIAN_POINT ( 'NONE',  ( 98.29820294272414571, 7.653668647302724892, 18.47759065022804137 ) ) ;
#1293 = CARTESIAN_POINT ( 'NONE',  ( 192.4448373802101173, -14.14213562370342281, 42.42640687122062104 ) ) ;
#1294 = CARTESIAN_POINT ( 'NONE',  ( 14.38125909742180752, 15.17850393972634038, 40.00000000000002132 ) ) ;
#1295 = ORIENTED_EDGE ( 'NONE', *, *, #10302, .T. ) ;
#1296 = CARTESIAN_POINT ( 'NONE',  ( -30.26275506840325136, 57.76657404653985139, 1.198031551616126178 ) ) ;
#1297 = CARTESIAN_POINT ( 'NONE',  ( -87.11182023518614415, -17.01577573093364038, -13.17795446294752892 ) ) ;
#1298 = CARTESIAN_POINT ( 'NONE',  ( -296.0000000000000000, -4.857225732735059864E-14, 0.000000000000000000 ) ) ;
#1299 = CARTESIAN_POINT ( 'NONE',  ( -4.151555265633143144, -46.95165237383028511, -13.82020782288861049 ) ) ;
#1300 = B_SPLINE_CURVE_WITH_KNOTS ( 'NONE', 3,
 ( #17774, #5676, #13782, #21915, #16582, #4097, #6334, #18444, #18306, #24984, #12323, #22585, #219, #92, #10469, #8332, #6211, #8734, #12197, #22712, #12591, #14188, #4363, #22321, #24844, #24714, #16852 ),
 .UNSPECIFIED., .F., .F.,
 ( 4, 2, 1, 1, 2, 2, 2, 2, 2, 2, 2, 2, 1, 2, 4 ),
 ( -6.000000000158344332E-08, 0.0002171475752860021037, 0.0004343551505720058027, 0.0008687703011440085386, 0.001737600602288021275, 0.003475261204576048698, 0.006950582409152100509, 0.01390122481830420413, 0.02085186722745631036, 0.02432718843203236087, 0.02606484903432039479, 0.02693367933546441523, 0.02736809448603642544, 0.02758530206132243576, 0.02780250963660844607 ),
 .UNSPECIFIED. ) ;
#1301 = ORIENTED_EDGE ( 'NONE', *, *, #3436, .F. ) ;
#1302 = CARTESIAN_POINT ( 'NONE',  ( -187.8778500559185431, -43.02985669704839466, 17.82355023088355495 ) ) ;
#1303 = AXIS2_PLACEMENT_3D ( 'NONE', #1699, #13783, #11796 ) ;
#1304 = CARTESIAN_POINT ( 'NONE',  ( 199.9999999999996305, -13.87326568555608830, -12.99368172854615366 ) ) ;
#1305 = CARTESIAN_POINT ( 'NONE',  ( 98.29820294267315717, -7.653668647304116668, 18.47759065023120684 ) ) ;
#1306 = LINE ( 'NONE', #11034, #4996 ) ;
#1307 = CARTESIAN_POINT ( 'NONE',  ( 199.0053384867209445, 15.04244419640346031, -13.18878631234924192 ) ) ;
#1308 = CARTESIAN_POINT ( 'NONE',  ( -199.9999999999998010, 24.82633483071100500, -44.86878812508844305 ) ) ;
#1309 = CARTESIAN_POINT ( 'NONE',  ( -135.8532207217289738, 40.00000000000002842, -9.153146818113432559 ) ) ;
#1310 = CARTESIAN_POINT ( 'NONE',  ( -626.9846540392142060, 75.00000000000000000, 0.000000000000000000 ) ) ;
#1311 = CARTESIAN_POINT ( 'NONE',  ( 23.09931156284629239, 46.91113948292964864, -13.81622350327230109 ) ) ;
#1312 = CARTESIAN_POINT ( 'NONE',  ( 199.9999999999999432, -19.99999999999988987, -2.449293598294708485E-15 ) ) ;
#1313 = AXIS2_PLACEMENT_3D ( 'NONE', #15630, #7391, #23754 ) ;
#1315 = CARTESIAN_POINT ( 'NONE',  ( -611.8146452038604366, 30.48906968622233649, -25.89952525135564798 ) ) ;
#1314 = CARTESIAN_POINT ( 'NONE',  ( -183.1091233172942907, 22.43565125815459282, -41.47045062400935223 ) ) ;
#1316 = CARTESIAN_POINT ( 'NONE',  ( 170.2234770963711128, -15.44714144992813409, 40.00000000000002132 ) ) ;
#1317 = CARTESIAN_POINT ( 'NONE',  ( -198.0356074513804572, -15.37879056873074290, 0.000000000000000000 ) ) ;
#1318 = AXIS2_PLACEMENT_3D ( 'NONE', #22270, #8151, #8412 ) ;
#1319 = CARTESIAN_POINT ( 'NONE',  ( 19.06497207195980792, 14.19242893257840699, 40.00000000000002132 ) ) ;
#1320 = CARTESIAN_POINT ( 'NONE',  ( -100.7734535825088500, 39.99999999999976552, 22.67402823373233645 ) ) ;
#1321 = AXIS2_PLACEMENT_3D ( 'NONE', #15134, #2783, #25005 ) ;
#1322 = CARTESIAN_POINT ( 'NONE',  ( 184.8905102610680444, -40.00000000000021316, 20.92133201514402430 ) ) ;
#1323 = CARTESIAN_POINT ( 'NONE',  ( 98.93808658348716278, -18.71306740730482687, -7.751206313707100115 ) ) ;
#1324 = ORIENTED_EDGE ( 'NONE', *, *, #12009, .T. ) ;
#1326 = CARTESIAN_POINT ( 'NONE',  ( -4.260882601030880679, 46.91379881627385373, -13.81249720866881248 ) ) ;
#1325 = CARTESIAN_POINT ( 'NONE',  ( -86.94949953272028154, 20.30809431151143229, -6.679047987429632904 ) ) ;
#1327 = CARTESIAN_POINT ( 'NONE',  ( -213.1075012329537230, -53.71589010950170717, 40.00000000000002132 ) ) ;
#1328 = CARTESIAN_POINT ( 'NONE',  ( -86.96347745069644475, -15.38646221621807442, 15.38646221621768184 ) ) ;
#1329 = B_SPLINE_CURVE_WITH_KNOTS ( 'NONE', 3,
 ( #21318, #7074, #19683, #19306, #11317, #969, #23682, #13073, #11071, #17180, #21189, #2961, #5332, #19557 ),
 .UNSPECIFIED., .F., .F.,
 ( 4, 2, 2, 2, 2, 2, 4 ),
 ( 1.040834085586084257E-17, 0.002941681445496978960, 0.004412522168245460417, 0.005883362890993943176, 0.008825044336490900018, 0.01029588505923937844, 0.01176672578198786033 ),
 .UNSPECIFIED. ) ;
#1330 = CARTESIAN_POINT ( 'NONE',  ( -188.6013476421588564, 43.09288642756978760, -23.51433506917260630 ) ) ;
#1331 = DIRECTION ( 'NONE',  ( 1.000000000000000000, 0.000000000000000000, 0.000000000000000000 ) ) ;
#1332 = ORIENTED_EDGE ( 'NONE', *, *, #7657, .T. ) ;
#1333 = ORIENTED_EDGE ( 'NONE', *, *, #17104, .F. ) ;
#1334 = FACE_OUTER_BOUND ( 'NONE', #18817, .T. ) ;
#1335 = CARTESIAN_POINT ( 'NONE',  ( 164.1122551457364409, 10.10009781492438918, -24.38379312608493521 ) ) ;
#1336 = VERTEX_POINT ( 'NONE', #11014 ) ;
#1337 = EDGE_CURVE ( 'NONE', #2862, #11180, #19124, .T. ) ;
#1338 = VERTEX_POINT ( 'NONE', #8746 ) ;
#1339 = CARTESIAN_POINT ( 'NONE',  ( 200.0000000000003411, -11.08347333911627963, 15.44584840147742355 ) ) ;
#1340 = AXIS2_PLACEMENT_3D ( 'NONE', #8100, #26229, #11702 ) ;
#1341 = CARTESIAN_POINT ( 'NONE',  ( -315.0000000000000568, -4.857225732735059864E-14, 0.000000000000000000 ) ) ;
#1342 = CARTESIAN_POINT ( 'NONE',  ( -198.0356074513804572, 67.44298959253333692, 10.87444709760969452 ) ) ;
#1343 = AXIS2_PLACEMENT_3D ( 'NONE', #16929, #25063, #6815 ) ;
#1344 = ADVANCED_FACE ( 'NONE', ( #18724 ), #13391, .T. ) ;
#1345 = CARTESIAN_POINT ( 'NONE',  ( 170.0000000000000000, 24.95097643317003744, 0.000000000000000000 ) ) ;
#1346 = CARTESIAN_POINT ( 'NONE',  ( -198.0356074513804572, -9.007331120208026888E-14, 15.37879056873070560 ) ) ;
#1347 = CARTESIAN_POINT ( 'NONE',  ( -105.2276019129704991, -13.16696799169988452, -17.02331989733613327 ) ) ;
#1348 = CARTESIAN_POINT ( 'NONE',  ( -210.0000000000000284, 69.29737539576900929, -75.30386416458597409 ) ) ;
#1349 = B_SPLINE_CURVE_WITH_KNOTS ( 'NONE', 3,
 ( #13548, #17297, #15539, #5314, #1457, #9433, #11058, #13425, #21548, #7058, #19543, #17540, #1328, #7425, #25678, #23667, #21301, #5447, #9184, #21801, #9691, #7684, #17797, #23922, #3574, #13679, #15798, #25943, #11677, #19802 ),
 .UNSPECIFIED., .F., .F.,
 ( 4, 2, 2, 2, 2, 2, 2, 2, 2, 2, 2, 2, 2, 2, 4 ),
 ( 0.000000000000000000, 0.1357259735107005372, 0.1651108541090157700, 0.1944957347073310028, 0.3598804999793158710, 0.3867117631979620773, 0.4135430264166082281, 0.5789277916885930964, 0.6062785021374117456, 0.6336292125862302838, 0.8508620842112317728, 0.8814014469398914198, 0.9119408096685510667, 0.9559704048342755334, 0.9981086137545830406 ),
 .UNSPECIFIED. ) ;
#1350 = EDGE_CURVE ( 'NONE', #16014, #12649, #10884, .T. ) ;
#1351 = ADVANCED_FACE ( 'NONE', ( #8881 ), #18725, .T. ) ;
#1352 = CARTESIAN_POINT ( 'NONE',  ( -77.90255099906853786, 8.644468104252323926, -20.04994828524279882 ) ) ;
#1353 = CARTESIAN_POINT ( 'NONE',  ( -56.48582580120557850, -39.99999999999970868, -30.84685318188687120 ) ) ;
#1354 = CARTESIAN_POINT ( 'NONE',  ( 184.8905102610680444, 2.362515690532070066E-13, -19.07866798485558490 ) ) ;
#1355 = CARTESIAN_POINT ( 'NONE',  ( -114.6821015619795645, -12.10555619827156626, 18.42370988052079284 ) ) ;
#1356 = CARTESIAN_POINT ( 'NONE',  ( 14.38125909742181818, -39.01709431150904095, -17.55144818341490165 ) ) ;
#1357 = CARTESIAN_POINT ( 'NONE',  ( 151.7948205124836534, 40.00000000000017053, -33.23291073765538783 ) ) ;
#1358 = CARTESIAN_POINT ( 'NONE',  ( -126.6834154283287575, 24.04426794716025739, -11.16464792285741403 ) ) ;
#1359 = CARTESIAN_POINT ( 'NONE',  ( 155.1206158682454657, 27.79897307351018654, 11.51471166709261951 ) ) ;
#1360 = CARTESIAN_POINT ( 'NONE',  ( -77.67292258764840085, 18.59814239105719125, -11.80983163631141863 ) ) ;
#1361 = CARTESIAN_POINT ( 'NONE',  ( 170.2234770963711128, 45.64576402573181468, 10.92277846919223627 ) ) ;
#1362 = CARTESIAN_POINT ( 'NONE',  ( 91.82158438592159655, -39.99999999999994316, -17.20528682183314118 ) ) ;
#1363 = CARTESIAN_POINT ( 'NONE',  ( 91.82158438592158234, -12.16597498400057198, 44.40256751092329779 ) ) ;
#1364 = AXIS2_PLACEMENT_3D ( 'NONE', #13312, #5086, #21558 ) ;
#1365 = CARTESIAN_POINT ( 'NONE',  ( -238.4067589809705794, -57.25054294077233408, -0.6820004458489551391 ) ) ;
#1366 = CARTESIAN_POINT ( 'NONE',  ( -639.6467708969067871, 30.97534985185962242, -32.64842303514383559 ) ) ;
#1367 = CARTESIAN_POINT ( 'NONE',  ( 130.8568914410475372, -3.326198072800416995E-13, 34.05028731879788495 ) ) ;
#1368 = ORIENTED_EDGE ( 'NONE', *, *, #8822, .F. ) ;
#1369 = CARTESIAN_POINT ( 'NONE',  ( 130.8568914410475372, 4.207082182992923691, -4.207082182992794017 ) ) ;
#1370 = DIRECTION ( 'NONE',  ( 0.000000000000000000, -1.000000000000000000, 0.000000000000000000 ) ) ;
#1371 = CYLINDRICAL_SURFACE ( 'NONE', #14023, 5.000000000000004441 ) ;
#1372 = ORIENTED_EDGE ( 'NONE', *, *, #13149, .T. ) ;
#1373 = CARTESIAN_POINT ( 'NONE',  ( 200.0000000000000000, -40.00000000000019185, 19.99999999999968381 ) ) ;
#1374 = CARTESIAN_POINT ( 'NONE',  ( -2.652172544013602362, -23.73409167602005354, 43.38951316025630689 ) ) ;
#1375 = FACE_OUTER_BOUND ( 'NONE', #4952, .T. ) ;
#1376 = ORIENTED_EDGE ( 'NONE', *, *, #13301, .T. ) ;
#1377 = ORIENTED_EDGE ( 'NONE', *, *, #13860, .T. ) ;
#1378 = CARTESIAN_POINT ( 'NONE',  ( -86.96347745069645896, -12.89780903124382938, -43.67073346367985920 ) ) ;
#1379 = CARTESIAN_POINT ( 'NONE',  ( -259.2033419157646676, 39.99999999999987210, 30.48217210827754542 ) ) ;
#1380 = CARTESIAN_POINT ( 'NONE',  ( -114.7826396787323375, -16.63820453137681454, -14.66025082034670213 ) ) ;
#1381 = AXIS2_PLACEMENT_3D ( 'NONE', #11675, #9306, #19800 ) ;
#1382 = CARTESIAN_POINT ( 'NONE',  ( 170.0000000000133014, 17.64300463311800016, 17.64300463311827016 ) ) ;
#1383 = CARTESIAN_POINT ( 'NONE',  ( -213.1075012329537230, -2.291445344039133686E-13, 53.71589010951915100 ) ) ;
#1384 = CARTESIAN_POINT ( 'NONE',  ( 199.9999999999999716, -15.72304121538119936, -10.67928908684366540 ) ) ;
#1385 = CARTESIAN_POINT ( 'NONE',  ( -105.3755690713226585, 40.00000000000007816, -21.75974354311636461 ) ) ;
#1386 = DIRECTION ( 'NONE',  ( 1.000000000000000000, -0.000000000000000000, -0.000000000000000000 ) ) ;
#1387 = CARTESIAN_POINT ( 'NONE',  ( -5.866564133085600652, -13.69896896866330849, -46.35727274689645583 ) ) ;
#1388 = CARTESIAN_POINT ( 'NONE',  ( -238.4067589809705794, 27.60227080167080160, -28.96627169325299533 ) ) ;
#1389 = CARTESIAN_POINT ( 'NONE',  ( -317.0000000000000568, -4.857225732735059864E-14, -31.79780246617542616 ) ) ;
#1390 = CARTESIAN_POINT ( 'NONE',  ( 0.2972598230770103767, -39.99999999999945288, -54.33493731733979359 ) ) ;
#1391 = CARTESIAN_POINT ( 'NONE',  ( 73.43468551893268170, -28.18272074650139203, -9.843145830824745701 ) ) ;
#1392 = CARTESIAN_POINT ( 'NONE',  ( 163.1118516004056573, 27.26290988616876021, 40.00000000000002132 ) ) ;
#1393 = CARTESIAN_POINT ( 'NONE',  ( 0.2972598230769983307, -14.33493731733933352, -40.00000000000002132 ) ) ;
#1394 = CARTESIAN_POINT ( 'NONE',  ( 163.1118516004056573, 47.56205970284957374, 9.006482792074494981 ) ) ;
#1395 = CARTESIAN_POINT ( 'NONE',  ( -30.26275506840324070, -1.694272468446265112, 0.000000000000000000 ) ) ;
#1397 = CARTESIAN_POINT ( 'NONE',  ( -86.86493150571116928, -8.366608963953867217, -19.60045294882765887 ) ) ;
#1396 = CARTESIAN_POINT ( 'NONE',  ( 98.29820294272414571, 7.653668647302724892, 18.47759065022804137 ) ) ;
#1398 = DIRECTION ( 'NONE',  ( 0.000000000000000000, -1.000000000000000000, 0.000000000000000000 ) ) ;
#1399 = CARTESIAN_POINT ( 'NONE',  ( 163.1118516004056573, 9.006482792069629539, 9.006482792069634868 ) ) ;
#1400 = CARTESIAN_POINT ( 'NONE',  ( 136.1360204305621551, 4.966164525587093870, -40.00000000000002132 ) ) ;
#1401 = ORIENTED_EDGE ( 'NONE', *, *, #19720, .F. ) ;
#1402 = CARTESIAN_POINT ( 'NONE',  ( 67.79414719545434309, -28.72755866870028285, 14.15005687161233361 ) ) ;
#1403 =( BOUNDED_SURFACE ( )  B_SPLINE_SURFACE ( 3, 2, ( 
 ( #357, #24710, #8062 ),
 ( #14184, #6465, #14580 ),
 ( #22317, #18709, #89 ),
 ( #16178, #12587, #14714 ),
 ( #6080, #16709, #4621 ),
 ( #8461, #8198, #14318 ),
 ( #2351, #4094, #24841 ),
 ( #20717, #20316, #12194 ),
 ( #16314, #22709, #12720 ),
 ( #18172, #492, #2092 ),
 ( #12320, #24314, #14453 ),
 ( #10200, #1960, #22580 ),
 ( #18302, #4486, #24439 ),
 ( #10596, #4360, #8600 ),
 ( #6592, #6206, #22846 ),
 ( #22451, #4230, #18577 ),
 ( #2483, #10465, #10067 ),
 ( #16579, #26320, #20446 ),
 ( #2224, #10332, #216 ),
 ( #18441, #8327, #12451 ),
 ( #16451, #24575, #6331 ),
 ( #20578, #11243, #23366 ),
 ( #7124, #2621, #10735 ),
 ( #6861, #22976, #14843 ),
 ( #891, #8730, #25371 ),
 ( #16976, #19236, #9000 ),
 ( #2758, #24981, #21242 ),
 ( #5142, #21111, #1017 ),
 ( #624, #14978, #6731 ),
 ( #17230, #17105, #4753 ),
 ( #18980, #2890, #16848 ),
 ( #25237, #23112, #12859 ),
 ( #18846, #25112, #20845 ),
 ( #20977, #10861, #10998 ),
 ( #19107, #17361, #759 ),
 ( #15234, #8863, #13248 ),
 ( #4884, #6989, #9119 ),
 ( #11123, #12989, #5015 ),
 ( #23490, #9255, #15104 ),
 ( #23239, #13121, #3016 ),
 ( #21372, #3140, #19360 ),
 ( #1150, #25497, #7245 ),
 ( #15366, #5264, #9375 ),
 ( #17609, #11367, #17484 ),
 ( #13886, #1662, #25627 ),
 ( #21746, #13366, #23998 ),
 ( #7896, #13620, #23735 ),
 ( #3521, #9637, #26152 ),
 ( #5779, #3791, #11488 ),
 ( #1271, #22021, #16015 ),
 ( #7373, #1798, #24141 ),
 ( #21490, #23867, #5391 ),
 ( #11621, #25751, #19743 ),
 ( #13495, #15484, #23611 ),
 ( #9771, #3263, #9902 ),
 ( #11894, #21617, #20015 ),
 ( #3392, #25882, #7760 ),
 ( #18008, #19616, #19487 ),
 ( #1402, #26021, #9503 ),
 ( #7499, #7625, #15611 ),
 ( #5516, #1532, #17739 ),
 ( #15739, #15870, #5643 ) ),
 .UNSPECIFIED., .F., .F., .F. ) 
 B_SPLINE_SURFACE_WITH_KNOTS ( ( 4, 2, 2, 2, 2, 2, 2, 2, 2, 2, 2, 2, 2, 2, 2, 2, 2, 2, 2, 2, 2, 2, 2, 2, 2, 2, 2, 2, 2, 2, 4 ),
 ( 3, 3 ),
 ( 0.005118828937694837322, 0.02956064127319293564, 0.05400245360869103395, 0.07844426594418912879, 0.08149949248612639585, 0.08302710575709502938, 0.08379091239257935309, 0.08417281571032150800, 0.08436376736919258545, 0.08445924319862813112, 0.08450698111334589702, 0.08455471902806366291, 0.09066517211193818315, 0.09677562519581270339, 0.09983085173774997045, 0.1028860782796872375, 0.1089965313635617716, 0.1151069844474362919, 0.1181622109893735451, 0.1196898242603421786, 0.1204536308958265023, 0.1208355342135686572, 0.1208594031709275401, 0.1208832721282864231, 0.1209310100430041890, 0.1210264858724397347, 0.1212174375313108121, 0.1273278906151853462, 0.1517697029506834272, 0.1762115152861815359, 0.2006533276216796446 ),
 ( 0.000000000000000000, 1.000000000000000000 ),
 .UNSPECIFIED. ) 
 GEOMETRIC_REPRESENTATION_ITEM ( )  RATIONAL_B_SPLINE_SURFACE ( (
 ( 1.000000000000000000, 0.9997813423572990965, 1.000000000000000000),
 ( 1.000000000000000000, 0.9990919206318839008, 1.000000000000000000),
 ( 1.000000000000000000, 0.9967874177841469230, 1.000000000000000000),
 ( 1.000000000000000000, 0.9887544623280424272, 1.000000000000000000),
 ( 1.000000000000000000, 0.9830290792185782944, 1.000000000000000000),
 ( 1.000000000000000000, 0.9678345454235133261, 1.000000000000000000),
 ( 1.000000000000000000, 0.9583650305396005376, 1.000000000000000000),
 ( 1.000000000000000000, 0.9453335293272576711, 1.000000000000000000),
 ( 1.000000000000000000, 0.9438523872746900079, 1.000000000000000000),
 ( 1.000000000000000000, 0.9415799504610725679, 1.000000000000000000),
 ( 1.000000000000000000, 0.9408140170424496018, 1.000000000000000000),
 ( 1.000000000000000000, 0.9396523143998791738, 1.000000000000000000),
 ( 1.000000000000000000, 0.9392629463989451422, 1.000000000000000000),
 ( 1.000000000000000000, 0.9386756783046033004, 1.000000000000000000),
 ( 1.000000000000000000, 0.9384793862554601240, 1.000000000000000000),
 ( 1.000000000000000000, 0.9381841422087060511, 1.000000000000000000),
 ( 1.000000000000000000, 0.9380855931974548811, 1.000000000000000000),
 ( 1.000000000000000000, 0.9379375679425719925, 1.000000000000000000),
 ( 1.000000000000000000, 0.9378881925679177778, 1.000000000000000000),
 ( 1.000000000000000000, 0.9378140790407639704, 1.000000000000000000),
 ( 1.000000000000000000, 0.9377896949153107231, 1.000000000000000000),
 ( 1.000000000000000000, 0.9377409313168988403, 1.000000000000000000),
 ( 1.000000000000000000, 0.9377165729686763873, 1.000000000000000000),
 ( 1.000000000000000000, 0.9345773786260987981, 1.000000000000000000),
 ( 1.000000000000000000, 0.9318492984274224789, 1.000000000000000000),
 ( 1.000000000000000000, 0.9273872927429853696, 1.000000000000000000),
 ( 1.000000000000000000, 0.9256532593469947168, 1.000000000000000000),
 ( 1.000000000000000000, 0.9239357372751189068, 1.000000000000000000),
 ( 1.000000000000000000, 0.9235102113428168558, 1.000000000000000000),
 ( 1.000000000000000000, 0.9229728558028662544, 1.000000000000000000),
 ( 1.000000000000000000, 0.9228633126626074601, 1.000000000000000000),
 ( 1.000000000000000000, 0.9230139704737772011, 1.000000000000000000),
 ( 1.000000000000000000, 0.9237531682202682060, 1.000000000000000000),
 ( 1.000000000000000000, 0.9264156051932146418, 1.000000000000000000),
 ( 1.000000000000000000, 0.9283388455998524691, 1.000000000000000000),
 ( 1.000000000000000000, 0.9320050037531947273, 1.000000000000000000),
 ( 1.000000000000000000, 0.9333574575348377866, 1.000000000000000000),
 ( 1.000000000000000000, 0.9355411998009157681, 1.000000000000000000),
 ( 1.000000000000000000, 0.9362956009277125791, 1.000000000000000000),
 ( 1.000000000000000000, 0.9374637148015746435, 1.000000000000000000),
 ( 1.000000000000000000, 0.9378591705544939705, 1.000000000000000000),
 ( 1.000000000000000000, 0.9384610703419805633, 1.000000000000000000),
 ( 1.000000000000000000, 0.9386631562400454820, 1.000000000000000000),
 ( 1.000000000000000000, 0.9388793792114364933, 1.000000000000000000),
 ( 1.000000000000000000, 0.9388921037490475241, 1.000000000000000000),
 ( 1.000000000000000000, 0.9389175638858665573, 1.000000000000000000),
 ( 1.000000000000000000, 0.9389305010154709308, 1.000000000000000000),
 ( 1.000000000000000000, 0.9389691441648050363, 1.000000000000000000),
 ( 1.000000000000000000, 0.9389948969011622237, 1.000000000000000000),
 ( 1.000000000000000000, 0.9390721270299990930, 1.000000000000000000),
 ( 1.000000000000000000, 0.9391235763422335348, 1.000000000000000000),
 ( 1.000000000000000000, 0.9392778120326625846, 1.000000000000000000),
 ( 1.000000000000000000, 0.9393804861645765891, 1.000000000000000000),
 ( 1.000000000000000000, 0.9427638002347920043, 1.000000000000000000),
 ( 1.000000000000000000, 0.9458915987233171840, 1.000000000000000000),
 ( 1.000000000000000000, 0.9607963039206464106, 1.000000000000000000),
 ( 1.000000000000000000, 0.9703812854709539248, 1.000000000000000000),
 ( 1.000000000000000000, 0.9854660764533730299, 1.000000000000000000),
 ( 1.000000000000000000, 0.9909632567911320633, 1.000000000000000000),
 ( 1.000000000000000000, 0.9982308762617714271, 1.000000000000000000),
 ( 1.000000000000000000, 0.9999976772058264407, 1.000000000000000000),
 ( 1.000000000000000000, 1.000000000000000000, 1.000000000000000000) ) ) 
 REPRESENTATION_ITEM ( '' )  SURFACE ( )  );
#1404 = DIRECTION ( 'NONE',  ( -1.000000000000000000, 0.000000000000000000, 0.000000000000000000 ) ) ;
#1405 = CARTESIAN_POINT ( 'NONE',  ( -56.48582580120559982, -6.472252184284282173, 50.09629031063965243 ) ) ;
#1406 = CARTESIAN_POINT ( 'NONE',  ( 184.8905102610680444, 1.070102760522089011E-13, -20.92133201514444352 ) ) ;
#1407 = CARTESIAN_POINT ( 'NONE',  ( 151.7948205124836250, -23.49921654116371883, 23.49921654116317526 ) ) ;
#1408 = CARTESIAN_POINT ( 'NONE',  ( 14.38125909742180752, 55.17850393971008316, -40.00000000000002132 ) ) ;
#1409 = DIRECTION ( 'NONE',  ( -1.000000000000000000, 1.836970198721030181E-16, 0.000000000000000000 ) ) ;
#1410 = CARTESIAN_POINT ( 'NONE',  ( 200.0000000000000568, -6.707298731100607370, 17.79007541258576452 ) ) ;
#1411 = CARTESIAN_POINT ( 'NONE',  ( -82.23724611274339225, 0.6214486198419367780, -20.19553932739445656 ) ) ;
#1412 = CARTESIAN_POINT ( 'NONE',  ( -162.0762913951021176, 29.48230308784730980, 27.08623940707652622 ) ) ;
#1413 = CARTESIAN_POINT ( 'NONE',  ( -105.3755690713226585, 15.38646221621820764, -41.18208027870583265 ) ) ;
#1414 = CARTESIAN_POINT ( 'NONE',  ( 19.06497207195981147, -10.03556273973439517, 10.03556273973429214 ) ) ;
#1415 = CARTESIAN_POINT ( 'NONE',  ( 136.1360204305621266, -24.77266263493151044, 24.77266263493093135 ) ) ;
#1416 = CARTESIAN_POINT ( 'NONE',  ( 146.6084372240433709, 52.76785682606523409, -3.800685668858194255 ) ) ;
#1418 = CARTESIAN_POINT ( 'NONE',  ( 19.06497207195980792, -18.24870850772710540, -38.31983398719647482 ) ) ;
#1417 = CARTESIAN_POINT ( 'NONE',  ( 151.7948205124835681, 51.78348778862544322, -4.785054706298002891 ) ) ;
#1419 = CARTESIAN_POINT ( 'NONE',  ( -105.3755690713226727, -15.38646221621807619, 15.38646221621768362 ) ) ;
#1420 = CARTESIAN_POINT ( 'NONE',  ( -114.5520595707410081, -6.810300319901277710, -20.89066663055196926 ) ) ;
#1421 = CARTESIAN_POINT ( 'NONE',  ( 184.8905102610680444, -14.79361573936379415, -14.79361573936387941 ) ) ;
#1422 = CARTESIAN_POINT ( 'NONE',  ( -30.26275506840324070, -40.00000000000003553, 1.694272468446120117 ) ) ;
#1423 = CARTESIAN_POINT ( 'NONE',  ( 14.38125909742181285, -10.73282306404712472, -10.73282306404731301 ) ) ;
#1424 = CARTESIAN_POINT ( 'NONE',  ( -192.9588430854689989, 54.46834944099968823, 2.449293598294708485E-15 ) ) ;
#1426 = EDGE_CURVE ( 'NONE', #5206, #17844, #12718, .T. ) ;
#1425 = VERTEX_POINT ( 'NONE', #2470 ) ;
#1427 = CARTESIAN_POINT ( 'NONE',  ( 170.2234770963711128, 39.20704971665398375, -17.36149277826984871 ) ) ;
#1428 = CARTESIAN_POINT ( 'NONE',  ( 18.43739873636958393, 43.10664370278630031, 17.85535645007986716 ) ) ;
#1429 = CARTESIAN_POINT ( 'NONE',  ( 98.29820294267337033, 7.653668647303973671, 18.47759065023120328 ) ) ;
#1430 = CARTESIAN_POINT ( 'NONE',  ( -87.12800209209288482, -21.45652401693875078, 1.368681197236398361 ) ) ;
#1431 = EDGE_CURVE ( 'NONE', #11418, #14640, #18510, .T. ) ;
#1432 = ORIENTED_EDGE ( 'NONE', *, *, #16631, .F. ) ;
#1433 = CARTESIAN_POINT ( 'NONE',  ( -200.5022718138936284, -44.86987976039414860, 18.58571273880634322 ) ) ;
#1434 = CARTESIAN_POINT ( 'NONE',  ( 200.0000000000000000, -10.04040541317802315, -16.13598245992451297 ) ) ;
#1435 = CARTESIAN_POINT ( 'NONE',  ( 23.54890483848222615, -13.78807129923187169, 46.74501720879658961 ) ) ;
#1436 = EDGE_CURVE ( 'NONE', #20782, #10228, #1513, .T. ) ;
#1437 = AXIS2_PLACEMENT_3D ( 'NONE', #19135, #5044, #3043 ) ;
#1438 = CARTESIAN_POINT ( 'NONE',  ( 199.0055466334479206, 16.72508833076945223, -10.95857635003404873 ) ) ;
#1439 = CARTESIAN_POINT ( 'NONE',  ( -87.13361725327072804, 21.49321519333427233, -1.448021113139547951E-30 ) ) ;
#1440 = CARTESIAN_POINT ( 'NONE',  ( -86.96347745069645896, 40.00000000000008527, -21.75974354311636461 ) ) ;
#1441 = CARTESIAN_POINT ( 'NONE',  ( -91.56559293963834989, 6.234561990864368500E-14, -22.67402823373191723 ) ) ;
#1442 =( BOUNDED_CURVE ( )  B_SPLINE_CURVE ( 3, ( #15584, #17204, #991, #9096, #25341, #7098, #5235 ),
 .UNSPECIFIED., .F., .F. ) 
 B_SPLINE_CURVE_WITH_KNOTS ( ( 4, 3, 4 ),
 ( 0.007504621739143815112, 0.02318610956072928234, 0.03886759738231780614 ),
 .UNSPECIFIED. ) 
 CURVE ( )  GEOMETRIC_REPRESENTATION_ITEM ( )  RATIONAL_B_SPLINE_CURVE ( ( 0.5852718452494397594, 0.6660804010233953854, 0.8043231192735821322, 1.000000000000000000, 0.8043231192735440516, 0.6660804010233416506, 0.5852718452493926860 ) ) 
 REPRESENTATION_ITEM ( '' )  );
#1443 = CARTESIAN_POINT ( 'NONE',  ( 22.82385994800816320, 47.01156385802210025, -13.83113328680595266 ) ) ;
#1444 = CARTESIAN_POINT ( 'NONE',  ( 146.6084372240433993, -5.374981219216945938, -2.449293598294708485E-15 ) ) ;
#1446 = LINE ( 'NONE', #23782, #16395 ) ;
#1445 = CARTESIAN_POINT ( 'NONE',  ( -166.3490736462130144, 12.23457872939038715, -39.29841219616762515 ) ) ;
#1447 = CARTESIAN_POINT ( 'NONE',  ( -135.8532207217289738, 9.153146818113546246, -0.000000000000000000 ) ) ;
#1448 = CARTESIAN_POINT ( 'NONE',  ( 14.38125909742181285, -15.17850393972633505, 0.000000000000000000 ) ) ;
#1449 = CARTESIAN_POINT ( 'NONE',  ( 0.2972598230769930017, 14.33493731733933352, 40.00000000000002132 ) ) ;
#1450 = CARTESIAN_POINT ( 'NONE',  ( -135.8532207217289738, 40.00000000000031974, -30.84685318188603986 ) ) ;
#1451 = FACE_OUTER_BOUND ( 'NONE', #20749, .T. ) ;
#1452 = CARTESIAN_POINT ( 'NONE',  ( 98.47991336697563725, -18.54450719071631681, -7.681386385922040816 ) ) ;
#1453 = VERTEX_POINT ( 'NONE', #20834 ) ;
#1455 = CARTESIAN_POINT ( 'NONE',  ( 3.468680969976427608, 48.91035688725698805, -14.11592159092573162 ) ) ;
#1454 = CARTESIAN_POINT ( 'NONE',  ( -87.04503123322955105, 20.91882565556252871, -4.710636111838677031 ) ) ;
#1456 = CARTESIAN_POINT ( 'NONE',  ( 146.6084372240433993, 34.62501878078308692, 0.000000000000000000 ) ) ;
#1457 = CARTESIAN_POINT ( 'NONE',  ( -208.1127848780265026, 10.60833733269551615, -10.60833733269529766 ) ) ;
#1458 = DIRECTION ( 'NONE',  ( 0.000000000000000000, 0.000000000000000000, 1.000000000000000000 ) ) ;
#1459 =( NAMED_UNIT ( * ) SI_UNIT ( $, .STERADIAN. ) SOLID_ANGLE_UNIT ( ) );
#1460 = ORIENTED_EDGE ( 'NONE', *, *, #20049, .T. ) ;
#1461 = ORIENTED_EDGE ( 'NONE', *, *, #4114, .T. ) ;
#1462 = DIRECTION ( 'NONE',  ( 1.000000000000000000, 1.836970198721030427E-16, -0.000000000000000000 ) ) ;
#1463 = DIRECTION ( 'NONE',  ( 1.000000000000000000, 1.836970198721030427E-16, -0.000000000000000000 ) ) ;
#1464 = ORIENTED_EDGE ( 'NONE', *, *, #17113, .T. ) ;
#1465 = DIRECTION ( 'NONE',  ( 0.000000000000000000, 0.9767746502210199466, -0.2142691827715878516 ) ) ;
#1466 = ORIENTED_EDGE ( 'NONE', *, *, #15475, .T. ) ;
#1467 = CARTESIAN_POINT ( 'NONE',  ( 199.9999999999998863, -2.178116022715518074, 18.88665387132288487 ) ) ;
#1468 = CARTESIAN_POINT ( 'NONE',  ( -280.0000000000000000, 14.14213562373108424, -14.14213562373078759 ) ) ;
#1469 = CARTESIAN_POINT ( 'NONE',  ( 170.2234770963711128, 39.20704971665398375, -17.36149277826984871 ) ) ;
#1470 = LINE ( 'NONE', #1089, #20851 ) ;
#1471 = CARTESIAN_POINT ( 'NONE',  ( 0.2972598230769957217, -4.999556039334937811E-14, 14.33493731733933352 ) ) ;
#1472 = CARTESIAN_POINT ( 'NONE',  ( -190.6721700386038663, -23.91541588165673460, 43.63442057298713905 ) ) ;
#1473 = DIRECTION ( 'NONE',  ( 1.000000000000000000, -0.000000000000000000, -0.000000000000000000 ) ) ;
#1474 = DIRECTION ( 'NONE',  ( 0.000000000000000000, 1.000000000000000000, 0.000000000000000000 ) ) ;
#1475 = CARTESIAN_POINT ( 'NONE',  ( 170.2234770963711128, -2.259079968736224833E-13, 24.55285855007187124 ) ) ;
#1476 = CARTESIAN_POINT ( 'NONE',  ( -91.56559293963834989, -39.99999999999985789, -17.32597176626853042 ) ) ;
#1477 = CARTESIAN_POINT ( 'NONE',  ( -199.9999999999999432, -45.63305559644809506, -19.96680831879890761 ) ) ;
#1478 = CARTESIAN_POINT ( 'NONE',  ( 136.1360204305621266, -3.511608612530379592, -53.05693388239318153 ) ) ;
#1479 = CARTESIAN_POINT ( 'NONE',  ( -200.0000000000000000, 18.59955921182038807, -46.19968414209451169 ) ) ;
#1480 = CARTESIAN_POINT ( 'NONE',  ( 163.1118516004056573, -37.29075403953139300, -19.27778845539249630 ) ) ;
#1481 = CARTESIAN_POINT ( 'NONE',  ( -102.4068193528150061, 8.088405365068718211, 20.44188272012853957 ) ) ;
#1482 = EDGE_CURVE ( 'NONE', #10703, #20651, #8990, .T. ) ;
#1483 = CARTESIAN_POINT ( 'NONE',  ( -77.61378591600576726, 12.98772233503618878, -17.87002798532567027 ) ) ;
#1484 = CARTESIAN_POINT ( 'NONE',  ( 57.59792236341147031, 1.722363176415065089, -1.722363176415036445 ) ) ;
#1485 = CARTESIAN_POINT ( 'NONE',  ( 57.59792236341148453, -40.00000000000000000, -2.435789363418300546 ) ) ;
#1486 = CARTESIAN_POINT ( 'NONE',  ( -213.1075012329537230, 9.698598906462684965, 66.26714140138669507 ) ) ;
#1487 = CARTESIAN_POINT ( 'NONE',  ( -208.1127848780264742, -67.17687982760682530, -10.60833733268364298 ) ) ;
#1488 = CARTESIAN_POINT ( 'NONE',  ( -183.1091233172618615, -13.45963571010332949, -45.18843800007923051 ) ) ;
#1489 = DIRECTION ( 'NONE',  ( 0.000000000000000000, 1.000000000000000000, 0.000000000000000000 ) ) ;
#1490 = ORIENTED_EDGE ( 'NONE', *, *, #16234, .F. ) ;
#1491 = CARTESIAN_POINT ( 'NONE',  ( 4.995406935893290878, 39.06748935135239265, -39.06748935135144762 ) ) ;
#1492 = EDGE_CURVE ( 'NONE', #12353, #7498, #10988, .T. ) ;
#1493 = DIRECTION ( 'NONE',  ( -1.000000000000000000, -1.836970198721030181E-16, 0.000000000000000000 ) ) ;
#1494 = CARTESIAN_POINT ( 'NONE',  ( -615.3642883616319068, 30.56114224079260211, 33.03453977807346575 ) ) ;
#1495 = CARTESIAN_POINT ( 'NONE',  ( -213.1075012329537230, 9.698598906438871126, -66.26714140136179765 ) ) ;
#1496 = CARTESIAN_POINT ( 'NONE',  ( -265.6482238768269326, 4.898587196589409870E-15, 39.99999999999997158 ) ) ;
#1497 = ORIENTED_EDGE ( 'NONE', *, *, #23863, .F. ) ;
#1498 = CARTESIAN_POINT ( 'NONE',  ( 57.59792236341147031, -1.493297263419786540E-14, 2.435789363418160658 ) ) ;
#1499 = EDGE_CURVE ( 'NONE', #1963, #23636, #7438, .T. ) ;
#1500 = CARTESIAN_POINT ( 'NONE',  ( 199.0198738297864338, -18.40122271749203620, -7.840790799891646401 ) ) ;
#1501 = CARTESIAN_POINT ( 'NONE',  ( -77.90255099907078318, 8.644468104260425889, 20.04994828523877359 ) ) ;
#1502 = ORIENTED_EDGE ( 'NONE', *, *, #5255, .T. ) ;
#1503 = ORIENTED_EDGE ( 'NONE', *, *, #5754, .F. ) ;
#1504 = CARTESIAN_POINT ( 'NONE',  ( 184.8905102610680444, 19.07866798485562043, 2.449293598294708485E-15 ) ) ;
#1505 = CARTESIAN_POINT ( 'NONE',  ( -195.1685814578493421, -48.78510996053816484, -14.09692187700277444 ) ) ;
#1506 = CARTESIAN_POINT ( 'NONE',  ( 163.1118516004056573, 40.00000000000000711, 12.73709011382489642 ) ) ;
#1507 = CARTESIAN_POINT ( 'NONE',  ( -317.0000000000000568, -4.857225732735059864E-14, 0.000000000000000000 ) ) ;
#1508 = CARTESIAN_POINT ( 'NONE',  ( -208.1127848780265026, 38.89260858015777700, -38.89260858015687461 ) ) ;
#1509 = CARTESIAN_POINT ( 'NONE',  ( -135.8532207217289738, 39.99999999999990763, 9.153146818113990335 ) ) ;
#1510 = CARTESIAN_POINT ( 'NONE',  ( -91.56559293963834989, -7.976292724337646577E-14, 17.32597176626811120 ) ) ;
#1511 = CARTESIAN_POINT ( 'NONE',  ( 199.9999999999998579, -17.31468161508541570, -7.846489601088847188 ) ) ;
#1512 = COLOUR_RGB ( '',0.7921568627450980005, 0.8196078431372548767, 0.9333333333333333481 ) ;
#1513 = CIRCLE ( 'NONE', #21880, 14.99999999999999645 ) ;
#1514 = CARTESIAN_POINT ( 'NONE',  ( 200.0000000000000000, 40.00000000000012790, -19.99999999999996092 ) ) ;
#1515 = DIRECTION ( 'NONE',  ( 0.000000000000000000, 0.000000000000000000, -1.000000000000000000 ) ) ;
#1516 = CARTESIAN_POINT ( 'NONE',  ( -4.915070467875013449, -23.27857837409171182, -42.74707758271716074 ) ) ;
#1517 = CARTESIAN_POINT ( 'NONE',  ( -86.96347745069643054, 15.38646221621821297, -41.18208027870583265 ) ) ;
#1518 = DIRECTION ( 'NONE',  ( -1.511376984792852195E-16, -4.006716270543645993E-17, -1.000000000000000000 ) ) ;
#1519 = CARTESIAN_POINT ( 'NONE',  ( -280.0000000000000568, -40.00000000000028422, 19.99999999999959499 ) ) ;
#1520 = CARTESIAN_POINT ( 'NONE',  ( -200.0000000000000000, 66.50000000000009948, 66.50000000000005684 ) ) ;
#1521 = CARTESIAN_POINT ( 'NONE',  ( 57.59792236341147031, 2.435789363418171760, 0.000000000000000000 ) ) ;
#1522 = CARTESIAN_POINT ( 'NONE',  ( -135.8532207217289738, 9.153146818113548022, -40.00000000000002132 ) ) ;
#1523 = CARTESIAN_POINT ( 'NONE',  ( -56.48582580120559982, 34.75652343174597547, 21.81201906317791384 ) ) ;
#1524 = CIRCLE ( 'NONE', #247, 9.999999999999994671 ) ;
#1525 = CARTESIAN_POINT ( 'NONE',  ( 91.82158438592158234, 17.20528682183301683, 0.000000000000000000 ) ) ;
#1526 = CARTESIAN_POINT ( 'NONE',  ( 184.8905102610680444, -14.79361573936399665, 14.79361573936367158 ) ) ;
#1527 = CARTESIAN_POINT ( 'NONE',  ( -114.5247552372686357, 20.75064880308619308, 7.059277231979386613 ) ) ;
#1528 = CARTESIAN_POINT ( 'NONE',  ( -162.0762913951020892, 29.48230308784758691, 29.48230308784772191 ) ) ;
#1529 = ADVANCED_FACE ( 'NONE', ( #17473 ), #21477, .F. ) ;
#1530 = CARTESIAN_POINT ( 'NONE',  ( 170.2234770963711128, 15.44714144992819094, 2.449293598294708485E-15 ) ) ;
#1531 = EDGE_LOOP ( 'NONE', ( #6366, #4909, #3109, #25138 ) ) ;
#1532 = CARTESIAN_POINT ( 'NONE',  ( 90.68848423405329129, -21.28058941706692053, 8.814708751807811993 ) ) ;
#1533 = VECTOR ( 'NONE', #12308, 1000.000000000000000 ) ;
#1534 = CARTESIAN_POINT ( 'NONE',  ( 126.3230993689412855, 11.72464299830463652, 28.30579214049060610 ) ) ;
#1535 = CARTESIAN_POINT ( 'NONE',  ( 4.995406935893283773, 39.06748935135195211, -17.50105314357185193 ) ) ;
#1536 = CARTESIAN_POINT ( 'NONE',  ( 19.06497207195981858, -1.881589693694111225E-13, 54.19242893257843008 ) ) ;
#1537 = CARTESIAN_POINT ( 'NONE',  ( -56.48582580120559982, 21.81201906317729922, 34.75652343174635917 ) ) ;
#1538 = AXIS2_PLACEMENT_3D ( 'NONE', #24991, #24721, #9013 ) ;
#1539 = CARTESIAN_POINT ( 'NONE',  ( 130.8568914410475088, -34.05028731879786363, -40.00000000000002132 ) ) ;
#1540 = CARTESIAN_POINT ( 'NONE',  ( 200.0000000000000000, 60.27431767988573341, -73.32453023895050137 ) ) ;
#1541 = CARTESIAN_POINT ( 'NONE',  ( 199.9999999999998579, 3.088973468740698447, 18.75625871509165776 ) ) ;
#1542 = CARTESIAN_POINT ( 'NONE',  ( -86.86493150571115507, -7.943527260495787168, -19.77569912839188859 ) ) ;
#1543 = CARTESIAN_POINT ( 'NONE',  ( -30.26275506840324070, 1.198031551616030033, -1.198031551616006496 ) ) ;
#1544 = CARTESIAN_POINT ( 'NONE',  ( -91.56559293963834989, -12.25131212657475466, -12.25131212657495361 ) ) ;
#1545 = CARTESIAN_POINT ( 'NONE',  ( 91.82158438592158234, 12.16597498397773869, -12.16597498397759303 ) ) ;
#1546 = CARTESIAN_POINT ( 'NONE',  ( 91.82158438592158234, -1.633484621919921769E-13, 17.20528682183300262 ) ) ;
#1547 = CARTESIAN_POINT ( 'NONE',  ( 91.82158438592156813, 40.45024623143973486, -16.11829626348390931 ) ) ;
#1548 = AXIS2_PLACEMENT_3D ( 'NONE', #18108, #1759, #22118 ) ;
#1550 = CARTESIAN_POINT ( 'NONE',  ( -86.96347745069644475, -43.67073346367964604, -12.89780903124457545 ) ) ;
#1549 = CARTESIAN_POINT ( 'NONE',  ( -198.0356074513804288, -39.15871834505882276, -39.15871834505946936 ) ) ;
#1551 = CARTESIAN_POINT ( 'NONE',  ( 91.82158438592158234, -12.16597498399995203, -44.40256751092347542 ) ) ;
#1552 = CARTESIAN_POINT ( 'NONE',  ( -259.2033419157646676, 6.730120644403521979, -6.730120644403498886 ) ) ;
#1553 = CARTESIAN_POINT ( 'NONE',  ( 170.0000000000000000, 24.95097643317003744, 0.000000000000000000 ) ) ;
#1555 = CARTESIAN_POINT ( 'NONE',  ( 184.8905102610680444, -39.99999999999991473, -20.92133201514458207 ) ) ;
#1554 = CARTESIAN_POINT ( 'NONE',  ( 57.59792236341147031, 26.56190807104652052, 30.00663442387728708 ) ) ;
#1556 = CARTESIAN_POINT ( 'NONE',  ( -56.48582580120558561, 6.472252184283903809, 50.09629031063968796 ) ) ;
#1557 = CARTESIAN_POINT ( 'NONE',  ( 199.9999999999999432, 14.14213562373093680, 14.14213562373114641 ) ) ;
#1558 = CARTESIAN_POINT ( 'NONE',  ( 151.7948205124836534, 6.767089262349056611, 40.00000000000002132 ) ) ;
#1559 = ORIENTED_EDGE ( 'NONE', *, *, #25834, .T. ) ;
#1560 = CARTESIAN_POINT ( 'NONE',  ( -162.0762913951020892, 1.198031840385716418, 1.198031840385750169 ) ) ;
#1561 = CARTESIAN_POINT ( 'NONE',  ( -77.92915424793434909, 20.15198149301296482, 8.347224043097730473 ) ) ;
#1562 = CARTESIAN_POINT ( 'NONE',  ( 98.29820294267334191, 7.653668647303994099, 18.47759065023120684 ) ) ;
#1563 = CARTESIAN_POINT ( 'NONE',  ( 98.29820294267339875, -20.00000000000581224, -1.310413973304028090 ) ) ;
#1564 = VERTEX_POINT ( 'NONE', #25870 ) ;
#1565 = CARTESIAN_POINT ( 'NONE',  ( -200.4317933031552741, -49.29858032309926585, 14.17468109412851796 ) ) ;
#1566 = CARTESIAN_POINT ( 'NONE',  ( 200.0000000000000568, -15.63904601878861733, 10.81246610429574595 ) ) ;
#1567 = CARTESIAN_POINT ( 'NONE',  ( -3.205219349397939510, -17.96245967913801778, 43.36521377095295549 ) ) ;
#1568 = CARTESIAN_POINT ( 'NONE',  ( 22.79879570922453169, 17.88067497375744352, -43.16776802602858254 ) ) ;
#1569 = CARTESIAN_POINT ( 'NONE',  ( 199.0059805750804571, 8.391908656364034158, -18.14947886101857932 ) ) ;
#1570 = UNCERTAINTY_MEASURE_WITH_UNIT (LENGTH_MEASURE( 1.000000000000000082E-05 ), #17119, 'distance_accuracy_value', 'NONE');
#1571 = CARTESIAN_POINT ( 'NONE',  ( -105.4741150117379789, -19.60045294982730724, -8.366608964594114184 ) ) ;
#1572 = CARTESIAN_POINT ( 'NONE',  ( 14.38125909742180930, 39.99999999999982947, 55.17850393971022527 ) ) ;
#1574 = AXIS2_PLACEMENT_3D ( 'NONE', #23163, #13295, #7298 ) ;
#1573 = CARTESIAN_POINT ( 'NONE',  ( -87.13361725327072804, -2.411356650979014119E-13, 21.49321519333428299 ) ) ;
#1575 = CARTESIAN_POINT ( 'NONE',  ( 19.06497207195981147, 38.31983398719673772, -38.31983398719579981 ) ) ;
#1576 = CARTESIAN_POINT ( 'NONE',  ( -105.3755690713226585, -18.24025645688355013, 40.00000000000002132 ) ) ;
#1578 = CARTESIAN_POINT ( 'NONE',  ( -265.0000000000000000, -4.857225732735059864E-14, 10.00000000000000000 ) ) ;
#1577 = CARTESIAN_POINT ( 'NONE',  ( 190.0000000000000000, 66.50000000000009948, -66.50000000000005684 ) ) ;
#1579 = DIRECTION ( 'NONE',  ( 0.7071067811865500152, 8.659560562354903276E-17, 0.7071067811865451302 ) ) ;
#1580 = CARTESIAN_POINT ( 'NONE',  ( 91.82158438592158234, 17.20528682183301683, 0.000000000000000000 ) ) ;
#1581 = CARTESIAN_POINT ( 'NONE',  ( 130.8568914410475088, -34.05028731879786363, 40.00000000000002132 ) ) ;
#1582 = CARTESIAN_POINT ( 'NONE',  ( 136.1360204305621551, -39.99999999999994316, -4.966164525587488221 ) ) ;
#1583 = CARTESIAN_POINT ( 'NONE',  ( 98.29820294273281434, -7.653668647304240125, 18.47759065023114644 ) ) ;
#1584 = CARTESIAN_POINT ( 'NONE',  ( -198.0356074513804572, 17.40982414986501325, -39.15871834505897198 ) ) ;
#1585 = ORIENTED_EDGE ( 'NONE', *, *, #12200, .F. ) ;
#1586 = CARTESIAN_POINT ( 'NONE',  ( -210.0000000000000284, 66.50000000000009948, 66.50000000000005684 ) ) ;
#1587 = CARTESIAN_POINT ( 'NONE',  ( 170.2234770963711128, 24.55285855007190676, 40.00000000000002132 ) ) ;
#1588 = EDGE_CURVE ( 'NONE', #11219, #16477, #2420, .T. ) ;
#1589 = FACE_OUTER_BOUND ( 'NONE', #24909, .T. ) ;
#1590 = CARTESIAN_POINT ( 'NONE',  ( -88.37877758189179644, -8.026456974226181984, 20.15391234919130525 ) ) ;
#1591 = ITEM_DEFINED_TRANSFORMATION ( 'NONE', 'NONE', #19755,  #21058 ) ;
#1592 = ORIENTED_EDGE ( 'NONE', *, *, #17520, .T. ) ;
#1593 = VERTEX_POINT ( 'NONE', #3641 ) ;
#1594 = CARTESIAN_POINT ( 'NONE',  ( 91.82158438592159655, -44.40256751092324095, -12.16597498400075139 ) ) ;
#1595 = CARTESIAN_POINT ( 'NONE',  ( 22.37977766478896058, -43.15105302556170130, -23.55755712318277162 ) ) ;
#1596 = VERTEX_POINT ( 'NONE', #23600 ) ;
#1597 = CARTESIAN_POINT ( 'NONE',  ( -208.1127848780264742, 15.00245453012665742, -40.00000000000002132 ) ) ;
#1598 = CARTESIAN_POINT ( 'NONE',  ( -105.4741150117399684, -19.60045294982700170, 8.366608964593480025 ) ) ;
#1599 = ORIENTED_EDGE ( 'NONE', *, *, #18731, .T. ) ;
#1600 = CARTESIAN_POINT ( 'NONE',  ( 199.9999999999996874, -6.995992324030534171, 17.67857064404661926 ) ) ;
#1601 = DIRECTION ( 'NONE',  ( -1.000000000000000000, 0.000000000000000000, 0.000000000000000000 ) ) ;
#1602 = CARTESIAN_POINT ( 'NONE',  ( 170.2234770963711128, -17.36149277826995885, 39.20704971665388427 ) ) ;
#1603 = B_SPLINE_CURVE_WITH_KNOTS ( 'NONE', 3,
 ( #9185, #3575, #17798, #3714, #5838, #9558, #1986, #13942, #3850, #25944, #17666, #5575 ),
 .UNSPECIFIED., .F., .F.,
 ( 4, 2, 2, 2, 2, 4 ),
 ( 0.000000000000000000, 0.005971690550335614737, 0.008957535825503465041, 0.01045045846308743052, 0.01119691978187945143, 0.01194338110067147407 ),
 .UNSPECIFIED. ) ;
#1604 = CARTESIAN_POINT ( 'NONE',  ( -200.0000000000000000, 0.000000000000000000, 0.000000000000000000 ) ) ;
#1605 =( BOUNDED_SURFACE ( )  B_SPLINE_SURFACE ( 3, 2, ( 
 ( #13412, #17920, #25666 ),
 ( #7292, #11804, #22065 ),
 ( #19790, #21536, #13536 ),
 ( #7672, #7412, #21661 ),
 ( #15526, #15784, #11407 ),
 ( #19658, #19529, #1445 ),
 ( #19924, #7801, #24050 ),
 ( #1314, #23781, #13667 ),
 ( #19409, #21790, #3562 ),
 ( #11666, #1707, #9680 ),
 ( #22334, #372, #7941 ),
 ( #12073, #8476, #6093 ),
 ( #12208, #4109, #16594 ),
 ( #24727, #24185, #22201 ),
 ( #14465, #18594, #16466 ),
 ( #20066, #24590, #18455 ),
 ( #10215, #9944, #16059 ),
 ( #14200, #6483, #11940 ),
 ( #16328, #1842, #24457 ),
 ( #4245, #2106, #103 ),
 ( #4374, #2368, #20194 ),
 ( #8210, #20329, #18321 ),
 ( #1974, #24329, #14595 ),
 ( #12464, #20592, #18054 ),
 ( #26205, #14334, #6221 ),
 ( #10080, #22466, #22724 ),
 ( #12335, #5959, #16196 ),
 ( #14069, #18185, #20463 ),
 ( #3976, #2237, #26335 ),
 ( #8076, #233, #10345 ),
 ( #8345, #6346, #22598 ),
 ( #10480, #19255, #18862 ),
 ( #17124, #10613, #1035 ),
 ( #25255, #16726, #6878 ) ),
 .UNSPECIFIED., .F., .F., .F. ) 
 B_SPLINE_SURFACE_WITH_KNOTS ( ( 4, 2, 2, 2, 2, 2, 2, 2, 2, 2, 2, 2, 2, 2, 2, 2, 4 ),
 ( 3, 3 ),
 ( 0.005135431517081130715, 0.02907016617530081351, 0.05300490083352049631, 0.07693963549174018257, 0.08292331915629509720, 0.08441924007243381545, 0.08446598760106314996, 0.08448936136537782415, 0.08451273512969248447, 0.08460623018695115349, 0.08479322030146849154, 0.08516720053050318151, 0.08591516098857254757, 0.08890700282085001183, 0.09189884465312747608, 0.09489068648540494033, 0.1008743701499598550 ),
 ( 0.000000000000000000, 1.000000000000000000 ),
 .UNSPECIFIED. ) 
 GEOMETRIC_REPRESENTATION_ITEM ( )  RATIONAL_B_SPLINE_SURFACE ( (
 ( 1.000000000000000000, 0.9997813423552077694, 1.000000000000000000),
 ( 1.000000000000000000, 0.9991063894442805404, 1.000000000000000000),
 ( 1.000000000000000000, 0.9968824679670509337, 1.000000000000000000),
 ( 1.000000000000000000, 0.9891556708430848666, 1.000000000000000000),
 ( 1.000000000000000000, 0.9836552227697955564, 1.000000000000000000),
 ( 1.000000000000000000, 0.9690804699604719241, 1.000000000000000000),
 ( 1.000000000000000000, 0.9600093828083156033, 1.000000000000000000),
 ( 1.000000000000000000, 0.9461484455230979584, 1.000000000000000000),
 ( 1.000000000000000000, 0.9432496483671297671, 1.000000000000000000),
 ( 1.000000000000000000, 0.9394619383806620538, 1.000000000000000000),
 ( 1.000000000000000000, 0.9386961831920602739, 1.000000000000000000),
 ( 1.000000000000000000, 0.9378979462694526648, 1.000000000000000000),
 ( 1.000000000000000000, 0.9378737491732507259, 1.000000000000000000),
 ( 1.000000000000000000, 0.9378374413774228646, 1.000000000000000000),
 ( 1.000000000000000000, 0.9378252326299143515, 1.000000000000000000),
 ( 1.000000000000000000, 0.9378013115143155609, 1.000000000000000000),
 ( 1.000000000000000000, 0.9377893564346093669, 1.000000000000000000),
 ( 1.000000000000000000, 0.9377296084626354222, 1.000000000000000000),
 ( 1.000000000000000000, 0.9376818978498914214, 1.000000000000000000),
 ( 1.000000000000000000, 0.9375390306864402890, 1.000000000000000000),
 ( 1.000000000000000000, 0.9374441388111856011, 1.000000000000000000),
 ( 1.000000000000000000, 0.9371605328928512835, 1.000000000000000000),
 ( 1.000000000000000000, 0.9369728885716379629, 1.000000000000000000),
 ( 1.000000000000000000, 0.9364143219790427297, 1.000000000000000000),
 ( 1.000000000000000000, 0.9360477663173715213, 1.000000000000000000),
 ( 1.000000000000000000, 0.9342452504720836215, 1.000000000000000000),
 ( 1.000000000000000000, 0.9329001521054777202, 1.000000000000000000),
 ( 1.000000000000000000, 0.9304320728631004789, 1.000000000000000000),
 ( 1.000000000000000000, 0.9293115496650089513, 1.000000000000000000),
 ( 1.000000000000000000, 0.9273349178230613221, 1.000000000000000000),
 ( 1.000000000000000000, 0.9264755994061862898, 1.000000000000000000),
 ( 1.000000000000000000, 0.9243018539389631361, 1.000000000000000000),
 ( 1.000000000000000000, 0.9233922906946041564, 1.000000000000000000),
 ( 1.000000000000000000, 0.9230540990195960083, 1.000000000000000000) ) ) 
 REPRESENTATION_ITEM ( '' )  SURFACE ( )  );
#1606 = CARTESIAN_POINT ( 'NONE',  ( 0.2972598230769959993, 38.42060263243713081, -38.42060263243619289 ) ) ;
#1607 = FACE_OUTER_BOUND ( 'NONE', #5363, .T. ) ;
#1608 = CARTESIAN_POINT ( 'NONE',  ( -362.0709805440841365, -4.734761052820324085E-14, -10.00000000000004796 ) ) ;
#1609 = CARTESIAN_POINT ( 'NONE',  ( -93.12335834970892279, -16.03295912088728414, 16.03295912088688269 ) ) ;
#1610 = CARTESIAN_POINT ( 'NONE',  ( -280.0000000000000000, -2.609240458947769655E-13, 20.00000000000001421 ) ) ;
#1611 = CARTESIAN_POINT ( 'NONE',  ( -114.4940140763160912, -9.297404372800567529, 19.81979918810025154 ) ) ;
#1612 = CARTESIAN_POINT ( 'NONE',  ( 91.82158438592156813, -16.11829626348402655, -40.45024623143966380 ) ) ;
#1613 = CARTESIAN_POINT ( 'NONE',  ( -259.2033419157646676, -30.48217210827743884, -40.00000000000002132 ) ) ;
#1614 = CARTESIAN_POINT ( 'NONE',  ( -105.3755690713226585, -12.89780903124383471, -43.67073346367985920 ) ) ;
#1615 = CARTESIAN_POINT ( 'NONE',  ( -96.93773665438791909, -9.001171854902402458, 20.58457565566394010 ) ) ;
#1616 = DIRECTION ( 'NONE',  ( -5.098616525425841937E-32, 2.775557561562890858E-16, 1.000000000000000000 ) ) ;
#1617 = CARTESIAN_POINT ( 'NONE',  ( -192.9588430854689989, 1.161019517985663313E-13, -14.46834944099969533 ) ) ;
#1618 = CARTESIAN_POINT ( 'NONE',  ( 136.1360204305621266, 1.473277640373554421E-13, -35.03383547441296741 ) ) ;
#1619 = CARTESIAN_POINT ( 'NONE',  ( 0.2972598230769990524, -18.14793986248724522, 38.42060263243662632 ) ) ;
#1620 = CARTESIAN_POINT ( 'NONE',  ( -100.7734535825088500, 16.03295912088691821, 16.03295912088721309 ) ) ;
#1621 = CARTESIAN_POINT ( 'NONE',  ( -195.5008451367478983, -18.44412755965894846, -44.52806290062954986 ) ) ;
#1622 = CARTESIAN_POINT ( 'NONE',  ( -192.9588430854689989, -10.23066800230756890, 10.23066800230742501 ) ) ;
#1623 = ORIENTED_EDGE ( 'NONE', *, *, #25740, .F. ) ;
#1624 = CARTESIAN_POINT ( 'NONE',  ( -238.4067589809705794, 28.96627169325354956, -28.96627169325289231 ) ) ;
#1625 = CARTESIAN_POINT ( 'NONE',  ( -114.7537493279899223, -2.780162309571297286, 21.97305528828380261 ) ) ;
#1626 = CARTESIAN_POINT ( 'NONE',  ( -105.3755690713226585, 21.75974354311648185, -40.00000000000002132 ) ) ;
#1627 = FACE_OUTER_BOUND ( 'NONE', #2486, .T. ) ;
#1628 = CARTESIAN_POINT ( 'NONE',  ( 4.995406935893294431, -17.50105314357144337, -39.06748935135212264 ) ) ;
#1629 = CARTESIAN_POINT ( 'NONE',  ( -77.59415595804735233, 2.768978254217757673, 21.92621357340613031 ) ) ;
#1630 = ORIENTED_EDGE ( 'NONE', *, *, #20692, .F. ) ;
#1631 = CARTESIAN_POINT ( 'NONE',  ( -86.96347745069644475, -2.438961472018186339E-13, 21.75974354311649961 ) ) ;
#1632 = CARTESIAN_POINT ( 'NONE',  ( 23.37394308801976806, -13.80096434448233111, -46.80823611210209378 ) ) ;
#1633 = CARTESIAN_POINT ( 'NONE',  ( -16.78454218904764872, 16.41855578209794686, 39.63790004357517915 ) ) ;
#1634 = VERTEX_POINT ( 'NONE', #15471 ) ;
#1635 = ORIENTED_EDGE ( 'NONE', *, *, #25912, .T. ) ;
#1636 = CARTESIAN_POINT ( 'NONE',  ( 146.6084372240433993, 5.374981219216999229, 2.449293598294708485E-15 ) ) ;
#1637 = CARTESIAN_POINT ( 'NONE',  ( -198.0356074513804572, -10.87444709759729911, 10.87444709759714812 ) ) ;
#1638 = CARTESIAN_POINT ( 'NONE',  ( -56.48582580120559982, 39.99999999999990763, 30.84685318188658698 ) ) ;
#1639 = CARTESIAN_POINT ( 'NONE',  ( -210.0000000000000284, -61.50000000000002132, -66.50000000000005684 ) ) ;
#1640 = EDGE_CURVE ( 'NONE', #23552, #10975, #18053, .T. ) ;
#1641 = AXIS2_PLACEMENT_3D ( 'NONE', #21190, #23317, #16661 ) ;
#1642 = CARTESIAN_POINT ( 'NONE',  ( 91.82158438592158234, 16.11829626346161604, -16.11829626346121103 ) ) ;
#1643 = CARTESIAN_POINT ( 'NONE',  ( 151.7948205124836250, -3.202120068677277203E-13, 33.23291073765553705 ) ) ;
#1644 = CARTESIAN_POINT ( 'NONE',  ( 180.0000000000000284, -125.7889608577475116, 82.50000000000001421 ) ) ;
#1645 = CARTESIAN_POINT ( 'NONE',  ( -129.2303492456788945, 9.309000511628456209, 25.82246949224157362 ) ) ;
#1646 = CARTESIAN_POINT ( 'NONE',  ( -2.557884977122323100, -23.77085849408081231, -43.43882039326604882 ) ) ;
#1647 = CARTESIAN_POINT ( 'NONE',  ( 19.06497207195982924, -66.60410523465809263, -10.03556273973493163 ) ) ;
#1648 = DIRECTION ( 'NONE',  ( -1.000000000000000000, 0.000000000000000000, 1.511376984792852195E-16 ) ) ;
#1649 = CARTESIAN_POINT ( 'NONE',  ( -198.0356074513804288, -39.15871834505936278, 39.15871834505892224 ) ) ;
#1650 = CARTESIAN_POINT ( 'NONE',  ( 163.1118516004056573, -40.00000000000027711, 27.26290988616830546 ) ) ;
#1651 = CARTESIAN_POINT ( 'NONE',  ( -626.9846540392142060, 95.00000000000000000, 30.00000000000005329 ) ) ;
#1652 = DIRECTION ( 'NONE',  ( -1.000000000000000000, -1.836970198721030181E-16, 0.000000000000000000 ) ) ;
#1653 = CARTESIAN_POINT ( 'NONE',  ( -86.96347745069644475, -18.24025645688354302, -2.449293598294708485E-15 ) ) ;
#1654 = CARTESIAN_POINT ( 'NONE',  ( 19.06497207195980792, 18.24870850772737185, 38.31983398719634692 ) ) ;
#1655 = CARTESIAN_POINT ( 'NONE',  ( 14.38125909742182884, -55.17850393971007605, 40.00000000000002132 ) ) ;
#1656 = CARTESIAN_POINT ( 'NONE',  ( -3.069599232962560986, -43.28003856805334237, -23.65302469262813290 ) ) ;
#1657 = CARTESIAN_POINT ( 'NONE',  ( 184.8905102610680444, -1.851754852062639767E-13, 20.92133201514444352 ) ) ;
#1658 = CARTESIAN_POINT ( 'NONE',  ( 130.8568914410475088, 32.49135343045483637, -24.07718906446901030 ) ) ;
#1659 = CARTESIAN_POINT ( 'NONE',  ( 192.4448373802100889, -20.00000000003938538, 0.000000000000000000 ) ) ;
#1661 = ORIENTED_EDGE ( 'NONE', *, *, #9798, .F. ) ;
#1660 = AXIS2_PLACEMENT_3D ( 'NONE', #24424, #14168, #4078 ) ;
#1662 = CARTESIAN_POINT ( 'NONE',  ( 22.76403192593588543, -43.17745271018599595, 17.88468650128193715 ) ) ;
#1663 = CARTESIAN_POINT ( 'NONE',  ( 104.1600437297061745, 8.548029202655486714, 20.63676802864342363 ) ) ;
#1664 = EDGE_CURVE ( 'NONE', #23424, #6149, #13484, .T. ) ;
#1665 = CARTESIAN_POINT ( 'NONE',  ( -198.0356074513804572, 39.15871834505912119, -17.40982414986464377 ) ) ;
#1666 = CARTESIAN_POINT ( 'NONE',  ( 184.8905102610680444, -39.99999999999991473, -20.92133201514458207 ) ) ;
#1667 = CARTESIAN_POINT ( 'NONE',  ( -86.96347745069644475, -15.38646221621807442, 15.38646221621768184 ) ) ;
#1668 = EDGE_CURVE ( 'NONE', #12661, #21773, #1139, .T. ) ;
#1669 = DIRECTION ( 'NONE',  ( 0.000000000000000000, -1.000000000000000000, 0.000000000000000000 ) ) ;
#1670 = CARTESIAN_POINT ( 'NONE',  ( -30.26275506840324070, 1.694272468446254232, 0.000000000000000000 ) ) ;
#1671 = FACE_OUTER_BOUND ( 'NONE', #18068, .T. ) ;
#1672 = CARTESIAN_POINT ( 'NONE',  ( 199.9999999999998863, 18.50936851023984886, -4.296315843485498220 ) ) ;
#1673 = EDGE_CURVE ( 'NONE', #19299, #23960, #24451, .T. ) ;
#1674 = EDGE_CURVE ( 'NONE', #3292, #2226, #4485, .T. ) ;
#1675 = CARTESIAN_POINT ( 'NONE',  ( 199.9999999999999432, -18.10102589806735907, -5.808760618774897466 ) ) ;
#1676 = CARTESIAN_POINT ( 'NONE',  ( -100.7734535825088500, 40.53558337403654832, 16.03295912088756481 ) ) ;
#1677 = CARTESIAN_POINT ( 'NONE',  ( 136.1360204305621551, 24.77266263493153176, -31.79587985999237887 ) ) ;
#1678 = DIRECTION ( 'NONE',  ( 1.000000000000000000, -0.000000000000000000, -0.000000000000000000 ) ) ;
#1679 = CARTESIAN_POINT ( 'NONE',  ( -87.04313178894985015, 18.12206666836759084, -11.44454159254445891 ) ) ;
#1680 = CARTESIAN_POINT ( 'NONE',  ( 163.1118516004056573, 19.27778845539265618, -37.29075403953135037 ) ) ;
#1682 = CARTESIAN_POINT ( 'NONE',  ( -210.0000000000000284, 72.72568232011437317, -59.67546976104961942 ) ) ;
#1681 = CARTESIAN_POINT ( 'NONE',  ( 57.59792236341148453, 1.722363176415528940, -54.84617931850878136 ) ) ;
#1683 = CARTESIAN_POINT ( 'NONE',  ( -238.4067589809705794, -27.60227080167029001, -28.96627169325357798 ) ) ;
#1684 = CARTESIAN_POINT ( 'NONE',  ( -210.0000000000000284, 66.50000000000009948, 66.50000000000005684 ) ) ;
#1685 = FACE_BOUND ( 'NONE', #26345, .T. ) ;
#1686 = AXIS2_PLACEMENT_3D ( 'NONE', #17256, #9399, #13145 ) ;
#1688 = CARTESIAN_POINT ( 'NONE',  ( -91.56559293963834989, -39.99999999999995737, -22.67402823373205933 ) ) ;
#1687 = CARTESIAN_POINT ( 'NONE',  ( 184.8905102610680444, -14.79361573936399665, 14.79361573936367158 ) ) ;
#1689 = CARTESIAN_POINT ( 'NONE',  ( -162.0762913951020607, -1.198031840455708430, 57.76657433537920383 ) ) ;
#1690 = CARTESIAN_POINT ( 'NONE',  ( 57.59792236341147031, -1.722363176415055985, 1.722363176415024677 ) ) ;
#1691 = CARTESIAN_POINT ( 'NONE',  ( -100.7734535825088500, 17.32597176626808988, 40.00000000000002132 ) ) ;
#1692 = ORIENTED_EDGE ( 'NONE', *, *, #20350, .T. ) ;
#1693 = CARTESIAN_POINT ( 'NONE',  ( -238.4067589809705794, 28.96627169325324758, -27.60227080167054581 ) ) ;
#1694 = LINE ( 'NONE', #15510, #2299 ) ;
#1695 = CARTESIAN_POINT ( 'NONE',  ( -317.0000000000000568, -4.857225732735059864E-14, 0.000000000000000000 ) ) ;
#1696 = CARTESIAN_POINT ( 'NONE',  ( 163.1118516004056573, -27.26290988616869626, 0.000000000000000000 ) ) ;
#1697 = ORIENTED_EDGE ( 'NONE', *, *, #15786, .F. ) ;
#1698 = CARTESIAN_POINT ( 'NONE',  ( -192.1963514251730203, -43.96876056340474292, 24.16258207727632978 ) ) ;
#1699 = CARTESIAN_POINT ( 'NONE',  ( -190.0000000000000000, -66.50000000000001421, -66.50000000000005684 ) ) ;
#1700 = CARTESIAN_POINT ( 'NONE',  ( -4.031723327955650582, -23.45082932595530423, 43.00750292060842384 ) ) ;
#1701 = VECTOR ( 'NONE', #17330, 1000.000000000000000 ) ;
#1702 = CARTESIAN_POINT ( 'NONE',  ( 23.35928221536270399, 23.34300348377183454, -42.86167611819463019 ) ) ;
#1703 = CARTESIAN_POINT ( 'NONE',  ( 199.0069448139248891, 19.47830345430216070, -4.521371627647083891 ) ) ;
#1704 = CARTESIAN_POINT ( 'NONE',  ( -362.0709805440841365, -4.605747634845933236E-14, -20.53474504356812247 ) ) ;
#1705 = CARTESIAN_POINT ( 'NONE',  ( 4.995406935893286438, 67.35176059880245703, -10.78321810387767066 ) ) ;
#1706 = CARTESIAN_POINT ( 'NONE',  ( -56.48582580120558561, -30.84685318188645908, 40.00000000000002132 ) ) ;
#1708 = CARTESIAN_POINT ( 'NONE',  ( -604.5625608938773894, 34.67764305556000437, -19.95380784793596973 ) ) ;
#1707 = CARTESIAN_POINT ( 'NONE',  ( -187.8779108535516400, 17.82355704116720574, -43.02987313850719886 ) ) ;
#1709 = CARTESIAN_POINT ( 'NONE',  ( 130.8568914410475372, 34.05028731879791337, 0.000000000000000000 ) ) ;
#1710 = CARTESIAN_POINT ( 'NONE',  ( 14.38125909742181285, -15.17850393972633505, -40.00000000000002132 ) ) ;
#1711 = CARTESIAN_POINT ( 'NONE',  ( 14.38125909742180752, 15.17850393972634038, 40.00000000000002132 ) ) ;
#1712 = CARTESIAN_POINT ( 'NONE',  ( 130.8568914410475372, 8.880724697947696879E-14, -5.949712681206690945 ) ) ;
#1713 = CARTESIAN_POINT ( 'NONE',  ( -30.26275506840324070, 1.218738420030236455E-14, -1.694272468446259783 ) ) ;
#1714 = CARTESIAN_POINT ( 'NONE',  ( -280.0000000000000000, 14.14213562373078581, 14.14213562373108424 ) ) ;
#1715 = ORIENTED_EDGE ( 'NONE', *, *, #626, .F. ) ;
#1716 = DIRECTION ( 'NONE',  ( -1.000000000000000000, -1.836970198721024264E-16, 0.000000000000000000 ) ) ;
#1717 = CARTESIAN_POINT ( 'NONE',  ( -192.9588430854689989, 10.23066800230742679, 10.23066800230749607 ) ) ;
#1718 = VECTOR ( 'NONE', #5729, 1000.000000000000000 ) ;
#1719 = CARTESIAN_POINT ( 'NONE',  ( -102.4294859495866348, -8.407280617917511023, 20.29697089056567805 ) ) ;
#1720 = SHAPE_DEFINITION_REPRESENTATION ( #22072, #14572 ) ;
#1721 = VERTEX_POINT ( 'NONE', #26011 ) ;
#1722 = ORIENTED_EDGE ( 'NONE', *, *, #12326, .T. ) ;
#1723 = CARTESIAN_POINT ( 'NONE',  ( -91.56559293963834989, -40.53558337403669753, -16.03295912088728770 ) ) ;
#1724 = CARTESIAN_POINT ( 'NONE',  ( 23.54890483848231852, -46.74501720879656119, -13.78807129923171892 ) ) ;
#1725 = ORIENTED_EDGE ( 'NONE', *, *, #3774, .F. ) ;
#1726 = CARTESIAN_POINT ( 'NONE',  ( -135.8532207217289738, -9.153146818113595984, -40.00000000000002132 ) ) ;
#1727 = CARTESIAN_POINT ( 'NONE',  ( -265.6482238768269326, 0.000000000000000000, -39.99999999999997158 ) ) ;
#1728 = EDGE_LOOP ( 'NONE', ( #13953, #10765, #25682, #21394 ) ) ;
#1729 = CARTESIAN_POINT ( 'NONE',  ( 200.0000000000000284, 10.29196162618721644, 15.98165385515595815 ) ) ;
#1730 = CARTESIAN_POINT ( 'NONE',  ( 150.0000000000000284, -125.7889608577475116, 82.50000000000001421 ) ) ;
#1731 = CARTESIAN_POINT ( 'NONE',  ( 163.1118516004056573, 9.006482792069629539, 9.006482792069634868 ) ) ;
#1732 = CARTESIAN_POINT ( 'NONE',  ( -188.9524938556045583, -43.19211203807761024, -23.58789616778846110 ) ) ;
#1733 = CARTESIAN_POINT ( 'NONE',  ( -213.1075012329537230, -2.291445344039133686E-13, 53.71589010951915100 ) ) ;
#1734 = CARTESIAN_POINT ( 'NONE',  ( 14.38125909742180752, 15.17850393972634038, 0.000000000000000000 ) ) ;
#1735 = CARTESIAN_POINT ( 'NONE',  ( -56.48582580120559982, -6.472252184283581400, -50.09629031063973059 ) ) ;
#1736 = CYLINDRICAL_SURFACE ( 'NONE', #23013, 10.00000000000000000 ) ;
#1737 = CIRCLE ( 'NONE', #16606, 6.000000000000005329 ) ;
#1738 = CARTESIAN_POINT ( 'NONE',  ( -30.26275506840324070, -1.147469862568086380E-14, 1.694272468446259783 ) ) ;
#1739 = CARTESIAN_POINT ( 'NONE',  ( -280.0000000000000568, -40.00000000000028422, 19.99999999999959499 ) ) ;
#1740 = EDGE_CURVE ( 'NONE', #20774, #862, #9363, .T. ) ;
#1741 = CARTESIAN_POINT ( 'NONE',  ( -110.0723150831631330, -10.27950330707893656, 17.37189535808295915 ) ) ;
#1742 = CARTESIAN_POINT ( 'NONE',  ( 151.7948205124836534, -33.06932595376343897, -23.49921654116042902 ) ) ;
#1743 = CARTESIAN_POINT ( 'NONE',  ( -30.26275506840324070, -1.694272468446265112, 0.000000000000000000 ) ) ;
#1744 = CARTESIAN_POINT ( 'NONE',  ( -213.1075012329537230, -37.98287015391232302, -18.58567234101164800 ) ) ;
#1745 = CARTESIAN_POINT ( 'NONE',  ( -102.4068193528148356, -8.735227608997083948, 20.17396017424882260 ) ) ;
#1746 = CARTESIAN_POINT ( 'NONE',  ( -716.9846540392142060, 52.49999999999991473, -82.49999999999998579 ) ) ;
#1747 = CARTESIAN_POINT ( 'NONE',  ( -208.1127848780264742, 40.00000000000014211, -15.00245453012627728 ) ) ;
#1748 = CARTESIAN_POINT ( 'NONE',  ( 14.38125909742181818, -40.00000000000007816, 15.17850393972619649 ) ) ;
#1749 = CARTESIAN_POINT ( 'NONE',  ( 130.8568914410475088, 32.49135343045483637, -24.07718906446901030 ) ) ;
#1750 = CARTESIAN_POINT ( 'NONE',  ( -114.4955329334175786, 9.314646064825868876, 19.81372178018229135 ) ) ;
#1751 = CARTESIAN_POINT ( 'NONE',  ( -188.3392995398488949, -13.83024151208627650, -47.00482667599261788 ) ) ;
#1752 = LINE ( 'NONE', #26110, #21903 ) ;
#1753 = EDGE_LOOP ( 'NONE', ( #10197, #3904, #12389, #11955 ) ) ;
#1754 = CARTESIAN_POINT ( 'NONE',  ( 151.7948205124836534, -51.78348778862529400, -4.785054706299085581 ) ) ;
#1755 = CARTESIAN_POINT ( 'NONE',  ( -114.6318783467511508, -5.473070270845196816, 21.31802243456079538 ) ) ;
#1756 = CARTESIAN_POINT ( 'NONE',  ( 19.06497207195981503, -14.19242893257840166, 0.000000000000000000 ) ) ;
#1757 = CARTESIAN_POINT ( 'NONE',  ( -716.9846540392142060, 52.50000000000007816, -52.49999999999999289 ) ) ;
#1758 = CARTESIAN_POINT ( 'NONE',  ( 170.2234770963711128, 10.92277846919216522, -10.92277846919186501 ) ) ;
#1759 = DIRECTION ( 'NONE',  ( 0.000000000000000000, 1.000000000000000000, 0.000000000000000000 ) ) ;
#1760 = VERTEX_POINT ( 'NONE', #1651 ) ;
#1761 = CIRCLE ( 'NONE', #7270, 30.00000000000000355 ) ;
#1762 = CARTESIAN_POINT ( 'NONE',  ( 200.0000000000000000, 18.75319608166667251, -3.074485549213874069 ) ) ;
#1763 = CARTESIAN_POINT ( 'NONE',  ( 48.46046611906520241, -11.89583623498083575, -37.63122027851154172 ) ) ;
#1764 = ADVANCED_FACE ( 'NONE', ( #15599, #23724, #21735 ), #7614, .F. ) ;
#1765 = CARTESIAN_POINT ( 'NONE',  ( -4.027137536851070898, 23.45200847982306414, 43.00884733904467794 ) ) ;
#1766 = AXIS2_PLACEMENT_3D ( 'NONE', #25196, #2714, #11077 ) ;
#1767 = ORIENTED_EDGE ( 'NONE', *, *, #12722, .F. ) ;
#1768 = EDGE_LOOP ( 'NONE', ( #17544, #2552, #14244, #8261 ) ) ;
#1769 = CARTESIAN_POINT ( 'NONE',  ( -56.48582580120559271, -6.472252184284187138, -6.472252184284199572 ) ) ;
#1770 = CARTESIAN_POINT ( 'NONE',  ( 199.0064300168743898, 6.416848550863170964, -18.94043562797172697 ) ) ;
#1771 = CARTESIAN_POINT ( 'NONE',  ( -77.55640685876514340, -14.66025389215425712, -16.63820144330994566 ) ) ;
#1772 = ADVANCED_FACE ( 'NONE', ( #5251 ), #11611, .T. ) ;
#1773 = CARTESIAN_POINT ( 'NONE',  ( -93.01741312761159008, -20.50009083235103446, -8.946232117463726041 ) ) ;
#1774 = DIRECTION ( 'NONE',  ( 1.000000000000000000, 1.836970198721030181E-16, 0.000000000000000000 ) ) ;
#1775 = EDGE_CURVE ( 'NONE', #13725, #1634, #18127, .T. ) ;
#1776 = CARTESIAN_POINT ( 'NONE',  ( 57.59792236341147031, -1.493297263419786540E-14, 2.435789363418160658 ) ) ;
#1777 = CYLINDRICAL_SURFACE ( 'NONE', #3646, 5.000000000000011546 ) ;
#1778 = CARTESIAN_POINT ( 'NONE',  ( -629.0557304578984485, 26.53345902544097967, -29.93287798360601570 ) ) ;
#1779 = AXIS2_PLACEMENT_3D ( 'NONE', #16083, #3998, #18078 ) ;
#1780 = FACE_OUTER_BOUND ( 'NONE', #14683, .T. ) ;
#1781 = CARTESIAN_POINT ( 'NONE',  ( 199.0160554649137907, 14.01242985958090692, 14.27167877623515757 ) ) ;
#1782 = CARTESIAN_POINT ( 'NONE',  ( -151.4802849345942093, 11.09498666340387096, 33.96623543969244707 ) ) ;
#1783 = CARTESIAN_POINT ( 'NONE',  ( 5.823571940223073895, -24.75780943188384242, -44.77584346942393267 ) ) ;
#1784 = CARTESIAN_POINT ( 'NONE',  ( -280.0000000000000568, -42.42640687119305198, 14.14213562373058686 ) ) ;
#1785 = CARTESIAN_POINT ( 'NONE',  ( -86.94949953272053733, -19.08279132442580561, 9.637191076868178996 ) ) ;
#1786 = CARTESIAN_POINT ( 'NONE',  ( -86.96347745069644475, -12.89780903124413491, 12.89780903124398037 ) ) ;
#1787 = CARTESIAN_POINT ( 'NONE',  ( -100.7734535825088358, -2.560096224687585342E-13, 22.67402823373191723 ) ) ;
#1788 = FACE_OUTER_BOUND ( 'NONE', #17941, .T. ) ;
#1789 = CARTESIAN_POINT ( 'NONE',  ( -213.1075012329537230, 18.58567234101174037, -37.98287015391222354 ) ) ;
#1790 = CARTESIAN_POINT ( 'NONE',  ( 151.7948205124836250, -6.767089262349004208, -2.449293598294708485E-15 ) ) ;
#1791 = DIRECTION ( 'NONE',  ( 1.000000000000000000, 1.836970198721030181E-16, 0.000000000000000000 ) ) ;
#1792 = CARTESIAN_POINT ( 'NONE',  ( -192.9588430854690273, -54.46834944098226572, 40.00000000000002132 ) ) ;
#1793 = CARTESIAN_POINT ( 'NONE',  ( -105.3209481228352615, 10.91022678754919006, 18.42900430629945774 ) ) ;
#1794 = CARTESIAN_POINT ( 'NONE',  ( 0.2972598230769956662, 40.00000000000058975, -54.33493731733894094 ) ) ;
#1795 = CARTESIAN_POINT ( 'NONE',  ( -238.4067589809705794, 0.6820004457912757223, 0.6820004457913219076 ) ) ;
#1796 = CARTESIAN_POINT ( 'NONE',  ( -30.26275506840324070, 1.694272468446254232, 0.000000000000000000 ) ) ;
#1797 = ORIENTED_EDGE ( 'NONE', *, *, #5393, .F. ) ;
#1798 = CARTESIAN_POINT ( 'NONE',  ( 22.89778847645078486, -43.13990468001248502, 17.86913359794352019 ) ) ;
#1799 = CIRCLE ( 'NONE', #3481, 6.000000000000019540 ) ;
#1800 = CARTESIAN_POINT ( 'NONE',  ( 140.2235668266256425, 12.60094438999802868, 30.42137084504315325 ) ) ;
#1801 = CARTESIAN_POINT ( 'NONE',  ( 192.4448373802101173, 42.42640687116508502, -14.14213562375874567 ) ) ;
#1802 = CARTESIAN_POINT ( 'NONE',  ( -238.4067589809705794, -40.00000000000021316, 40.96449427990166470 ) ) ;
#1803 = CARTESIAN_POINT ( 'NONE',  ( -162.0762913951021176, 29.48230308784730980, 27.08623940707652622 ) ) ;
#1804 = CARTESIAN_POINT ( 'NONE',  ( 199.9999999999999432, -1.727494763561684666E-13, 20.00000000000010303 ) ) ;
#1805 = CARTESIAN_POINT ( 'NONE',  ( -238.4067589809705794, 0.9644942799825386714, 0.000000000000000000 ) ) ;
#1806 = CARTESIAN_POINT ( 'NONE',  ( 199.0053211798077086, 14.13837298227953987, -14.13837298578013701 ) ) ;
#1807 = CARTESIAN_POINT ( 'NONE',  ( 199.9999999999999432, 16.89472078740815775, 8.702431973737679627 ) ) ;
#1808 = CARTESIAN_POINT ( 'NONE',  ( 199.9999999999999147, -18.88644897276319412, 2.180134100127611330 ) ) ;
#1809 = CARTESIAN_POINT ( 'NONE',  ( -198.0356074513804572, 67.44298959250878056, -10.87444709758402261 ) ) ;
#1810 = CARTESIAN_POINT ( 'NONE',  ( 130.8568914410475372, -4.207082182992785135, -4.207082182992884611 ) ) ;
#1811 = CARTESIAN_POINT ( 'NONE',  ( -110.0913210856344904, 19.97012681669859191, -3.048699489023670495 ) ) ;
#1812 = CARTESIAN_POINT ( 'NONE',  ( -87.05569247516073972, 17.94468678732786060, -11.73639047247175604 ) ) ;
#1813 = CARTESIAN_POINT ( 'NONE',  ( -91.56559293963834989, -40.53558337403692491, 16.03295912088671571 ) ) ;
#1815 = CARTESIAN_POINT ( 'NONE',  ( 192.4448373802100889, -14.14213562375896061, 14.14213562375865330 ) ) ;
#1814 = CARTESIAN_POINT ( 'NONE',  ( 130.8568914410475372, -4.207082182992785135, -4.207082182992884611 ) ) ;
#1816 = CARTESIAN_POINT ( 'NONE',  ( 4.995406935893294431, -17.50105314357144337, -39.06748935135212264 ) ) ;
#1817 = CARTESIAN_POINT ( 'NONE',  ( 146.6084372240433993, -34.62501878078303008, 0.000000000000000000 ) ) ;
#1818 = CARTESIAN_POINT ( 'NONE',  ( 199.0148629966199962, 15.54375530361796010, 12.59047442983698417 ) ) ;
#1819 = ADVANCED_FACE ( 'NONE', ( #21360 ), #3129, .F. ) ;
#1821 = CARTESIAN_POINT ( 'NONE',  ( -105.3755690713226585, -40.00000000000010658, 18.24025645688337249 ) ) ;
#1820 = CARTESIAN_POINT ( 'NONE',  ( -100.7734535825088500, -16.03295912088659492, -40.53558337403696044 ) ) ;
#1822 = CARTESIAN_POINT ( 'NONE',  ( 146.6084372240433709, 52.76785682606519146, 3.800685668858932775 ) ) ;
#1823 = CARTESIAN_POINT ( 'NONE',  ( -192.9588430854689989, 10.23066800230756712, -10.23066800230735396 ) ) ;
#1824 = CARTESIAN_POINT ( 'NONE',  ( 19.06497207195980792, 14.19242893257840699, 40.00000000000002132 ) ) ;
#1825 = EDGE_LOOP ( 'NONE', ( #17662, #23179 ) ) ;
#1826 = CARTESIAN_POINT ( 'NONE',  ( 170.2234770963711128, -17.36149277826985937, -17.36149277826995174 ) ) ;
#1827 = ADVANCED_FACE ( 'NONE', ( #11882 ), #11690, .T. ) ;
#1828 = CARTESIAN_POINT ( 'NONE',  ( 14.63649358215962515, 43.53262337840171625, 18.03180300901562916 ) ) ;
#1829 = CARTESIAN_POINT ( 'NONE',  ( 59.93546481434775330, 13.19882033562931056, 31.86477106141393989 ) ) ;
#1830 = CARTESIAN_POINT ( 'NONE',  ( -105.2054292635175585, -2.444554031225951202E-13, 21.49321519473985020 ) ) ;
#1831 = ADVANCED_FACE ( 'NONE', ( #1788 ), #23328, .T. ) ;
#1832 = ORIENTED_EDGE ( 'NONE', *, *, #10625, .F. ) ;
#1833 = CARTESIAN_POINT ( 'NONE',  ( -200.4317933031570647, -44.88237357214666901, 24.83634732651998789 ) ) ;
#1834 = CARTESIAN_POINT ( 'NONE',  ( 199.9999999999999147, -18.99336422956244874, -0.7807574862979690389 ) ) ;
#1835 = CARTESIAN_POINT ( 'NONE',  ( 19.66474694216432795, -18.18658454057326068, 43.90629905113207343 ) ) ;
#1836 = CARTESIAN_POINT ( 'NONE',  ( 22.76838195347366067, 17.88421977190837708, -43.17632592580126527 ) ) ;
#1837 = CARTESIAN_POINT ( 'NONE',  ( 199.0183492910935286, -16.99256592298258184, -10.55490704374186883 ) ) ;
#1838 = DIRECTION ( 'NONE',  ( 0.000000000000000000, 1.000000000000000000, 0.000000000000000000 ) ) ;
#1839 = CARTESIAN_POINT ( 'NONE',  ( -184.9730489280271684, -13.59277546673063952, 45.83721239345848630 ) ) ;
#1840 = CARTESIAN_POINT ( 'NONE',  ( 200.0000000000000000, 42.42640687119267540, 14.14213562373153543 ) ) ;
#1841 = CARTESIAN_POINT ( 'NONE',  ( 4.995406935893309530, -55.24977328856464709, 40.00000000000002132 ) ) ;
#1843 = CARTESIAN_POINT ( 'NONE',  ( 136.1360204305621266, -24.77266263493151044, 24.77266263493093135 ) ) ;
#1842 = CARTESIAN_POINT ( 'NONE',  ( -188.9478905404506577, 17.94277290414884973, -43.31768569177498307 ) ) ;
#1844 = CARTESIAN_POINT ( 'NONE',  ( -199.9999999999998579, 24.82633483071252201, 44.86878812508700776 ) ) ;
#1845 = CARTESIAN_POINT ( 'NONE',  ( 163.1118516004056573, 27.26290988616875310, 0.000000000000000000 ) ) ;
#1846 = CARTESIAN_POINT ( 'NONE',  ( 170.2234770963711128, -24.55285855007183926, 0.000000000000000000 ) ) ;
#1847 = CARTESIAN_POINT ( 'NONE',  ( 146.6084372240433993, 8.568076647504290689E-14, -5.374981219216972583 ) ) ;
#1848 = CARTESIAN_POINT ( 'NONE',  ( -30.26275506840324070, 1.198031551615912571, 57.76657404653985139 ) ) ;
#1849 = EDGE_CURVE ( 'NONE', #25714, #12267, #18484, .T. ) ;
#1850 = DIRECTION ( 'NONE',  ( 0.000000000000000000, -1.000000000000000000, 0.000000000000000000 ) ) ;
#1851 = CARTESIAN_POINT ( 'NONE',  ( 190.0000000000000000, -61.50000000000001421, -66.50000000000005684 ) ) ;
#1852 = ORIENTED_EDGE ( 'NONE', *, *, #12545, .T. ) ;
#1853 = CARTESIAN_POINT ( 'NONE',  ( -30.26275506840324070, 1.198031551616013601, 1.198031551616023371 ) ) ;
#1854 = B_SPLINE_CURVE_WITH_KNOTS ( 'NONE', 3,
 ( #21166, #21417, #23291, #17030, #5442, #1199, #15412, #2939, #814, #7049, #11049, #7170, #9053, #19160, #17535, #21294, #1068, #945, #19537, #21669, #17158, #11170, #3445, #19285, #9177, #8920, #11298, #17288, #3189, #15287, #25422, #11541, #9304, #17410, #5309, #13420, #21543, #3317, #1323, #9428, #1452, #18062, #10088 ),
 .UNSPECIFIED., .F., .F.,
 ( 4, 2, 2, 2, 2, 2, 2, 2, 2, 2, 2, 2, 2, 2, 2, 2, 2, 2, 1, 1, 1, 2, 4 ),
 ( 0.03014611463440037761, 0.03932844241433864491, 0.04391960630430777335, 0.04506739727680003638, 0.04621518824929229941, 0.04851077019427690873, 0.05310193408424610656, 0.05539751602923075058, 0.05769309797421538766, 0.06228426186418467569, 0.06687542575415394985, 0.06917100769913860081, 0.07146658964412323789, 0.07376217158910787497, 0.07605775353409251205, 0.08524008131403096322, 0.09442240909396941440, 0.09901357298393861917, 0.1013091549289232424, 0.1024569459014155609, 0.1030308413876617202, 0.1033177891307847929, 0.1036047368739078656 ),
 .UNSPECIFIED. ) ;
#1855 = CARTESIAN_POINT ( 'NONE',  ( -162.0762913951020892, -1.694272876828353702, 0.000000000000000000 ) ) ;
#1856 = CARTESIAN_POINT ( 'NONE',  ( -89.91498783732212985, -8.087768383116706872, 20.43892340025324117 ) ) ;
#1857 = APPLICATION_PROTOCOL_DEFINITION ( 'draft international standard', 'automotive_design', 1998, #24315 ) ;
#1858 = VERTEX_POINT ( 'NONE', #17248 ) ;
#1859 = ORIENTED_EDGE ( 'NONE', *, *, #18389, .T. ) ;
#1860 = CARTESIAN_POINT ( 'NONE',  ( -135.8532207217289738, -21.81201906317758343, -34.75652343174620995 ) ) ;
#1861 = CARTESIAN_POINT ( 'NONE',  ( 45.01779936602802223, -36.09695843547836347, -18.90344565818509537 ) ) ;
#1862 = EDGE_CURVE ( 'NONE', #16337, #25804, #232, .T. ) ;
#1863 = ORIENTED_EDGE ( 'NONE', *, *, #1350, .T. ) ;
#1864 = CARTESIAN_POINT ( 'NONE',  ( 14.38125909742180752, 15.17850393972634038, -40.00000000000002132 ) ) ;
#1865 = DIRECTION ( 'NONE',  ( 3.936061032557164822E-17, -0.2142691827715878794, -0.9767746502210200576 ) ) ;
#1866 = ORIENTED_EDGE ( 'NONE', *, *, #7645, .T. ) ;
#1867 = CARTESIAN_POINT ( 'NONE',  ( 199.9999999999998863, 8.252615397115851792, 17.12261885615216173 ) ) ;
#1868 = CARTESIAN_POINT ( 'NONE',  ( -726.9846540392142060, 66.50000000000009948, 61.50000000000005684 ) ) ;
#1869 = CARTESIAN_POINT ( 'NONE',  ( 184.8905102610680444, 13.49065550809817715, -43.07788698682574591 ) ) ;
#1870 = CARTESIAN_POINT ( 'NONE',  ( -188.8842637254079193, -43.30125340596319461, -17.93596642850435785 ) ) ;
#1871 = CARTESIAN_POINT ( 'NONE',  ( 19.06497207195981858, -40.00000000000007105, 14.19242893257826665 ) ) ;
#1872 = CARTESIAN_POINT ( 'NONE',  ( -135.8532207217289738, -9.153146818113595984, 40.00000000000002132 ) ) ;
#1873 = CARTESIAN_POINT ( 'NONE',  ( -30.26275506840323715, 29.48230279907829754, -29.48230279907758344 ) ) ;
#1874 = CARTESIAN_POINT ( 'NONE',  ( 199.0245441510845410, -3.586860678693493565, 19.68275873856094549 ) ) ;
#1875 = CARTESIAN_POINT ( 'NONE',  ( 19.06497207195981147, -4.605042221739098431E-14, 14.19242893257840521 ) ) ;
#1876 = CARTESIAN_POINT ( 'NONE',  ( 146.6084372240433709, -40.00000000000036238, 34.62501878078263218 ) ) ;
#1877 = CARTESIAN_POINT ( 'NONE',  ( -199.9999999999999716, -44.89135967046717468, -23.83302776610000961 ) ) ;
#1878 = CARTESIAN_POINT ( 'NONE',  ( -280.0000000000000568, 14.14213562373067745, 42.42640687119295251 ) ) ;
#1879 = CARTESIAN_POINT ( 'NONE',  ( -56.48582580120559982, -21.81201906317755501, -34.75652343174621706 ) ) ;
#1880 = DIRECTION ( 'NONE',  ( 0.000000000000000000, 1.000000000000000000, 0.000000000000000000 ) ) ;
#1881 = CARTESIAN_POINT ( 'NONE',  ( -295.0000000000000568, -4.734761052820324716E-14, -9.999999999999996447 ) ) ;
#1882 = CARTESIAN_POINT ( 'NONE',  ( 151.7948205124836250, -3.202120068677277203E-13, 33.23291073765553705 ) ) ;
#1883 = CARTESIAN_POINT ( 'NONE',  ( -86.96347745069644475, 5.999880687339585546E-14, -21.75974354311649961 ) ) ;
#1884 = CARTESIAN_POINT ( 'NONE',  ( 57.59792236341147031, 26.56190807104684382, 26.56190807104692553 ) ) ;
#1885 = CARTESIAN_POINT ( 'NONE',  ( 14.38125909742181818, -39.01709431150928253, 17.55144818341435808 ) ) ;
#1886 = CARTESIAN_POINT ( 'NONE',  ( -191.2490444017885522, -18.16428715638061675, -43.85246840378096067 ) ) ;
#1887 = CARTESIAN_POINT ( 'NONE',  ( 136.1360204305621266, -3.419521671106983309E-13, 35.03383547441296741 ) ) ;
#1888 = VERTEX_POINT ( 'NONE', #25639 ) ;
#1889 = CARTESIAN_POINT ( 'NONE',  ( -91.56559293963834989, -44.31723036834885932, -12.25131212657538171 ) ) ;
#1890 = DIRECTION ( 'NONE',  ( 0.000000000000000000, 0.000000000000000000, -1.000000000000000000 ) ) ;
#1891 = CARTESIAN_POINT ( 'NONE',  ( -114.5450021253300861, -6.791646844855799614, 20.85732849908779940 ) ) ;
#1892 = CARTESIAN_POINT ( 'NONE',  ( -105.3755690713226869, 21.75974354311648540, -0.000000000000000000 ) ) ;
#1893 = DIRECTION ( 'NONE',  ( 0.01051738792036196329, 0.9166396752537513404, 0.3995761383041158132 ) ) ;
#1894 = CARTESIAN_POINT ( 'NONE',  ( -105.3755690713226585, -15.38646221621738164, -41.18208027870615240 ) ) ;
#1895 =( NAMED_UNIT ( * ) SI_UNIT ( $, .STERADIAN. ) SOLID_ANGLE_UNIT ( ) );
#1896 = CARTESIAN_POINT ( 'NONE',  ( -77.58513204268632535, 2.423266694375444619, 21.97516623138666603 ) ) ;
#1897 = ORIENTED_EDGE ( 'NONE', *, *, #626, .T. ) ;
#1898 = CARTESIAN_POINT ( 'NONE',  ( 199.9999999999999432, 17.99863635774381621, -6.096428138147773623 ) ) ;
#1899 = CARTESIAN_POINT ( 'NONE',  ( -105.2334157265389507, -16.99665894158227175, 13.14152336620594141 ) ) ;
#1900 = CARTESIAN_POINT ( 'NONE',  ( 1.925538622541579148, 14.07631154915297778, 48.64880301060233592 ) ) ;
#1901 = ORIENTED_EDGE ( 'NONE', *, *, #389, .F. ) ;
#1902 = VERTEX_POINT ( 'NONE', #9516 ) ;
#1903 = PRODUCT_DEFINITION_SHAPE ( 'NONE', 'NONE',  #26355 ) ;
#1904 = CARTESIAN_POINT ( 'NONE',  ( -86.96347745069644475, -21.75974354311651737, 0.000000000000000000 ) ) ;
#1905 = CARTESIAN_POINT ( 'NONE',  ( 199.0078712948245823, 1.622169390422157242, -19.93073376281416031 ) ) ;
#1906 = CARTESIAN_POINT ( 'NONE',  ( -192.1131137119205903, -43.98782916596421444, 24.17676406461175631 ) ) ;
#1907 = SURFACE_STYLE_FILL_AREA ( #18387 ) ;
#1908 = CARTESIAN_POINT ( 'NONE',  ( -94.58360650945819259, -8.190527749723793605, -20.91945674500546559 ) ) ;
#1909 = CARTESIAN_POINT ( 'NONE',  ( -192.9588430854689989, 1.161019517985663313E-13, -14.46834944099969533 ) ) ;
#1910 = CARTESIAN_POINT ( 'NONE',  ( -626.9846540392142060, 75.00000000000000000, -74.99999999999991473 ) ) ;
#1911 = CARTESIAN_POINT ( 'NONE',  ( -83.21262154144253032, -13.72187187061456015, -33.12752917118434226 ) ) ;
#1912 = CARTESIAN_POINT ( 'NONE',  ( 199.0218477376944577, 3.734929907270702287, 19.65178994764128717 ) ) ;
#1913 = CARTESIAN_POINT ( 'NONE',  ( -196.2219207559400047, 43.48224904004372604, 18.01093727487041107 ) ) ;
#1914 = CARTESIAN_POINT ( 'NONE',  ( -4.915070467874963711, -13.76630780994289438, -46.68718905935000407 ) ) ;
#1915 = CARTESIAN_POINT ( 'NONE',  ( -100.7734535825088358, -12.25131212657475643, -12.25131212657495539 ) ) ;
#1916 = DIRECTION ( 'NONE',  ( 0.000000000000000000, 0.000000000000000000, 1.000000000000000000 ) ) ;
#1917 = CARTESIAN_POINT ( 'NONE',  ( 136.1360204305621266, -3.511608612530379592, -53.05693388239318153 ) ) ;
#1918 = CARTESIAN_POINT ( 'NONE',  ( 0.2972598230770030492, -39.99999999999987210, -14.33493731733975451 ) ) ;
#1919 = CARTESIAN_POINT ( 'NONE',  ( -105.3755690713226727, 15.38646221621771737, 15.38646221621800514 ) ) ;
#1920 = CARTESIAN_POINT ( 'NONE',  ( -259.2033419157646676, -30.48217210827744239, -2.449293598294708485E-15 ) ) ;
#1921 = CARTESIAN_POINT ( 'NONE',  ( -678.9461782662789346, 75.00000000000000000, -24.99999999999826628 ) ) ;
#1922 = CARTESIAN_POINT ( 'NONE',  ( 146.6084372240433709, -5.374981219216942385, -40.00000000000002132 ) ) ;
#1923 = CARTESIAN_POINT ( 'NONE',  ( -94.58366989427231886, 20.91926462023913658, -8.190486896678999429 ) ) ;
#1924 = CARTESIAN_POINT ( 'NONE',  ( 184.8905102610680444, 40.00000000000025580, -19.07866798485515503 ) ) ;
#1925 = CARTESIAN_POINT ( 'NONE',  ( 91.82158438592158234, -12.16597498397761967, -12.16597498397768007 ) ) ;
#1926 = EDGE_CURVE ( 'NONE', #1425, #13433, #19253, .T. ) ;
#1927 = CARTESIAN_POINT ( 'NONE',  ( -105.3755690713226727, -21.75974354311652093, 0.000000000000000000 ) ) ;
#1928 = ORIENTED_EDGE ( 'NONE', *, *, #25834, .F. ) ;
#1930 = ORIENTED_EDGE ( 'NONE', *, *, #13283, .T. ) ;
#1929 = EDGE_CURVE ( 'NONE', #15177, #10228, #3634, .T. ) ;
#1931 = CARTESIAN_POINT ( 'NONE',  ( 14.38125909742180752, 15.17850393972634038, 40.00000000000002132 ) ) ;
#1932 = CARTESIAN_POINT ( 'NONE',  ( -83.21262154144250189, -13.72187187061479641, 33.12752917118422857 ) ) ;
#1933 = CARTESIAN_POINT ( 'NONE',  ( -135.8532207217289738, -40.00000000000014921, 30.84685318188631697 ) ) ;
#1934 = AXIS2_PLACEMENT_3D ( 'NONE', #1520, #11748, #11232 ) ;
#1935 = CARTESIAN_POINT ( 'NONE',  ( -91.56559293963834989, 12.25131212657428748, 44.31723036834913643 ) ) ;
#1936 = CARTESIAN_POINT ( 'NONE',  ( 57.59792236341147031, -2.435789363418150444, 0.000000000000000000 ) ) ;
#1937 = CARTESIAN_POINT ( 'NONE',  ( 91.82158438592158234, -17.20528682183298486, 0.000000000000000000 ) ) ;
#1938 = CARTESIAN_POINT ( 'NONE',  ( 169.9999999999999716, 22.62041470344888339, -9.369682556672254137 ) ) ;
#1939 = CARTESIAN_POINT ( 'NONE',  ( 200.0000000000005116, 16.46820326627658204, -9.481692438271846157 ) ) ;
#1940 = CARTESIAN_POINT ( 'NONE',  ( 199.9999999999999432, -18.70500695855449891, 3.403006402435800215 ) ) ;
#1941 = CARTESIAN_POINT ( 'NONE',  ( 19.06497207195980792, 66.60410523465830579, -10.03556273973354251 ) ) ;
#1942 = CARTESIAN_POINT ( 'NONE',  ( 4.995406935893305977, -39.06748935135157552, -39.06748935135225764 ) ) ;
#1943 = CARTESIAN_POINT ( 'NONE',  ( -100.7734535825088500, -16.03295912088659492, -40.53558337403696044 ) ) ;
#1944 = CARTESIAN_POINT ( 'NONE',  ( -110.0687879519081918, 19.47486782027040775, 5.333724827205037933 ) ) ;
#1945 = CARTESIAN_POINT ( 'NONE',  ( -77.56349232223030299, 14.64315958561415343, -16.60062240782661647 ) ) ;
#1946 = CARTESIAN_POINT ( 'NONE',  ( 163.1118516004056573, -37.29075403953166301, 19.27778845539196695 ) ) ;
#1947 = CARTESIAN_POINT ( 'NONE',  ( 57.59792236341147031, -1.722363176415055985, 1.722363176415024677 ) ) ;
#1948 = CARTESIAN_POINT ( 'NONE',  ( 192.4448373802101173, -42.42640687122053578, -14.14213562370360577 ) ) ;
#1949 = CARTESIAN_POINT ( 'NONE',  ( 91.82158438592158234, 12.16597498397773869, -12.16597498397759303 ) ) ;
#1950 = CARTESIAN_POINT ( 'NONE',  ( 199.0255783348552825, -7.592917736791534367, 18.50773992579789251 ) ) ;
#1952 = CARTESIAN_POINT ( 'NONE',  ( -100.7734535825088500, -39.99999999999995737, -22.67402823373205578 ) ) ;
#1951 = CARTESIAN_POINT ( 'NONE',  ( 200.0000000000000000, 42.42640687119267540, 14.14213562373153543 ) ) ;
#1953 = CIRCLE ( 'NONE', #12143, 14.99999999999999467 ) ;
#1954 = CARTESIAN_POINT ( 'NONE',  ( 192.4448373802100889, 14.14213562375873678, 14.14213562375894817 ) ) ;
#1955 = AXIS2_PLACEMENT_3D ( 'NONE', #23408, #21788, #23653 ) ;
#1956 = CARTESIAN_POINT ( 'NONE',  ( 22.90311673802928993, 42.99920082299722424, -23.44499648834960936 ) ) ;
#1957 = CARTESIAN_POINT ( 'NONE',  ( -238.4067589809705794, 40.96449428006337001, -40.00000000000002132 ) ) ;
#1958 = ORIENTED_EDGE ( 'NONE', *, *, #4931, .F. ) ;
#1959 = CARTESIAN_POINT ( 'NONE',  ( -259.2033419157646676, -9.517827891722680178, 0.000000000000000000 ) ) ;
#1960 = CARTESIAN_POINT ( 'NONE',  ( -4.580761711674998793, -42.99740816077039796, 17.81010960708318791 ) ) ;
#1961 = CARTESIAN_POINT ( 'NONE',  ( -259.2033419157646676, -9.517827891722680178, 40.00000000000002132 ) ) ;
#1962 = VECTOR ( 'NONE', #14925, 1000.000000000000000 ) ;
#1963 = VERTEX_POINT ( 'NONE', #1164 ) ;
#1964 = AXIS2_PLACEMENT_3D ( 'NONE', #11885, #17999, #22143 ) ;
#1965 = CARTESIAN_POINT ( 'NONE',  ( -190.7345856380928524, -43.65254615100791113, 23.92884448222190841 ) ) ;
#1966 = CARTESIAN_POINT ( 'NONE',  ( 200.0000000000001137, -18.36608873747554327, 4.914565663504686377 ) ) ;
#1967 = VECTOR ( 'NONE', #9633, 1000.000000000000000 ) ;
#1968 = CARTESIAN_POINT ( 'NONE',  ( -2.164901439740674505, -23.84421257765607294, 43.53794903249384873 ) ) ;
#1969 = CARTESIAN_POINT ( 'NONE',  ( 23.30336656375570215, 23.35569295765361986, -42.87878279885786270 ) ) ;
#1970 = CARTESIAN_POINT ( 'NONE',  ( 199.0201284062958962, -18.60237515726647572, -7.352601386804158423 ) ) ;
#1971 = DIRECTION ( 'NONE',  ( 1.000000000000000000, 1.836970198721030181E-16, 0.000000000000000000 ) ) ;
#1972 = CARTESIAN_POINT ( 'NONE',  ( 0.2972598230769959993, 38.42060263243713081, -38.42060263243619289 ) ) ;
#1973 = CARTESIAN_POINT ( 'NONE',  ( -198.0356074513804572, -15.37879056873074290, 0.000000000000000000 ) ) ;
#1975 = CARTESIAN_POINT ( 'NONE',  ( 146.6084372240433993, -24.48358557860353457, 24.48358557860296258 ) ) ;
#1974 = CARTESIAN_POINT ( 'NONE',  ( -188.6890294954694980, 23.53287096354939223, -43.11788624870165876 ) ) ;
#1976 = PLANE ( 'NONE',  #22060 ) ;
#1977 = CARTESIAN_POINT ( 'NONE',  ( 184.8905102610680444, 20.92133201514447194, -40.00000000000002132 ) ) ;
#1978 = CARTESIAN_POINT ( 'NONE',  ( 19.06497207195980792, 54.19242893257844429, 40.00000000000002132 ) ) ;
#1979 = CARTESIAN_POINT ( 'NONE',  ( -135.8532207217289738, -39.99999999999972289, -30.84685318188688541 ) ) ;
#1980 = CARTESIAN_POINT ( 'NONE',  ( -208.1127848780264742, 67.17687982760683951, 10.60833733268317403 ) ) ;
#1981 = VECTOR ( 'NONE', #5648, 1000.000000000000000 ) ;
#1982 = LINE ( 'NONE', #3983, #845 ) ;
#1983 = CARTESIAN_POINT ( 'NONE',  ( 0.2972598230769923355, 18.14793986248751168, -38.42060263243650553 ) ) ;
#1984 = VERTEX_POINT ( 'NONE', #7261 ) ;
#1985 = CARTESIAN_POINT ( 'NONE',  ( -105.3755690713226585, -43.67073346367983788, 12.89780903124397149 ) ) ;
#1986 = CARTESIAN_POINT ( 'NONE',  ( -190.1935165880707075, 47.62328200654632582, -13.92226094463961594 ) ) ;
#1987 = SHAPE_DEFINITION_REPRESENTATION ( #9744, #126 ) ;
#1988 = EDGE_LOOP ( 'NONE', ( #758, #21990, #4423, #14129 ) ) ;
#1989 = ORIENTED_EDGE ( 'NONE', *, *, #16482, .T. ) ;
#1990 = CARTESIAN_POINT ( 'NONE',  ( 184.8905102610680444, -41.77492675555986779, -14.79361573936407304 ) ) ;
#1991 = CARTESIAN_POINT ( 'NONE',  ( 23.41418334855293537, -46.79369727367380705, -13.79799959793995079 ) ) ;
#1992 = ORIENTED_EDGE ( 'NONE', *, *, #23543, .T. ) ;
#1993 = CARTESIAN_POINT ( 'NONE',  ( 163.1118516004056573, 12.73709011382478806, -40.00000000000002132 ) ) ;
#1994 = DIRECTION ( 'NONE',  ( 2.985653255390529422E-32, -4.182618615277681568E-16, 1.000000000000000000 ) ) ;
#1995 = EDGE_LOOP ( 'NONE', ( #11759, #20286, #16388, #3299 ) ) ;
#1996 = CARTESIAN_POINT ( 'NONE',  ( 199.9999999999995737, 11.06459441337805494, 15.46579378046570952 ) ) ;
#1997 = DIRECTION ( 'NONE',  ( -1.000000000000000000, 0.000000000000000000, 0.000000000000000000 ) ) ;
#1998 = CARTESIAN_POINT ( 'NONE',  ( 130.8568914410475088, 4.207082182989741348, -52.36146031193420924 ) ) ;
#1999 = CARTESIAN_POINT ( 'NONE',  ( -188.4702232936773214, -43.05505437950338177, -23.48628015402992020 ) ) ;
#2000 = AXIS2_PLACEMENT_3D ( 'NONE', #23417, #23537, #25292 ) ;
#2001 = EDGE_CURVE ( 'NONE', #23636, #1963, #4068, .T. ) ;
#2002 = CARTESIAN_POINT ( 'NONE',  ( 14.38125909742181818, -40.00000000000007816, 15.17850393972619649 ) ) ;
#2003 = CARTESIAN_POINT ( 'NONE',  ( -56.48582580120559271, -9.153146818113595984, 0.000000000000000000 ) ) ;
#2004 = CARTESIAN_POINT ( 'NONE',  ( 184.8905102610680444, -14.79361573936330565, -41.77492675556016621 ) ) ;
#2005 = CARTESIAN_POINT ( 'NONE',  ( 199.0247325273615502, -4.232801689760709252, 19.55205092890061280 ) ) ;
#2006 = ADVANCED_FACE ( 'NONE', ( #3029 ), #5031, .F. ) ;
#2007 = B_SPLINE_CURVE_WITH_KNOTS ( 'NONE', 3,
 ( #3756, #20254, #16384, #24517, #6276, #14391 ),
 .UNSPECIFIED., .F., .F.,
 ( 4, 2, 4 ),
 ( -5.998621905616971167E-08, 0.03937827992696036478, 0.07875661984013977712 ),
 .UNSPECIFIED. ) ;
#2008 = CARTESIAN_POINT ( 'NONE',  ( 151.7948205124836250, 1.439163438361279259E-13, -33.23291073765553705 ) ) ;
#2009 = CARTESIAN_POINT ( 'NONE',  ( 151.7948205124836250, 1.807796684091926154E-15, 6.767089262349031742 ) ) ;
#2010 = CARTESIAN_POINT ( 'NONE',  ( 0.2972598230770103767, -39.99999999999945288, -54.33493731733979359 ) ) ;
#2011 = CARTESIAN_POINT ( 'NONE',  ( 192.4448373802101173, 39.99999999999998579, 19.99999999996075317 ) ) ;
#2012 = CARTESIAN_POINT ( 'NONE',  ( 57.59792236341147031, 2.435789363418171760, 0.000000000000000000 ) ) ;
#2013 = CARTESIAN_POINT ( 'NONE',  ( -259.2033419157646676, 6.730120644403214669, 49.83842185052034068 ) ) ;
#2014 = EDGE_CURVE ( 'NONE', #6828, #18680, #13381, .T. ) ;
#2015 = CARTESIAN_POINT ( 'NONE',  ( 91.82158438592156813, 17.20528682183302038, -40.00000000000002132 ) ) ;
#2016 = ADVANCED_FACE ( 'NONE', ( #25514, #21508 ), #1284, .F. ) ;
#2017 = CARTESIAN_POINT ( 'NONE',  ( -105.3755690713226585, -41.18208027870589660, -15.38646221621809040 ) ) ;
#2018 = CARTESIAN_POINT ( 'NONE',  ( -94.58366989427226201, -9.000605044545805455, 20.58370269626814775 ) ) ;
#2019 = LINE ( 'NONE', #4153, #21289 ) ;
#2020 = CARTESIAN_POINT ( 'NONE',  ( -259.2033419157646676, -1.473088368616265084E-13, 9.517827891722632216 ) ) ;
#2021 = CARTESIAN_POINT ( 'NONE',  ( 199.9999999999999432, -3.553951640073651008E-14, 19.99999999999992539 ) ) ;
#2022 = CARTESIAN_POINT ( 'NONE',  ( -238.4067589809705794, 57.25054294077225592, 0.6820004458485544596 ) ) ;
#2023 = CARTESIAN_POINT ( 'NONE',  ( -114.7731140143791038, 16.71335482098725578, 14.51162400671975305 ) ) ;
#2024 = CARTESIAN_POINT ( 'NONE',  ( -188.2652746676664606, -23.44263257803881118, -42.99511404082397092 ) ) ;
#2025 = CARTESIAN_POINT ( 'NONE',  ( -30.26275506840324070, -1.198031551616032919, 1.198031551616014712 ) ) ;
#2026 = VERTEX_POINT ( 'NONE', #15496 ) ;
#2027 = CARTESIAN_POINT ( 'NONE',  ( 14.38125909742180752, 10.73282306404735387, -10.73282306404708919 ) ) ;
#2028 = CARTESIAN_POINT ( 'NONE',  ( -79.35537823250633949, 19.65633339167321481, 8.141919877358327895 ) ) ;
#2029 = CARTESIAN_POINT ( 'NONE',  ( -192.9588430854690273, -14.46834944099973264, -40.00000000000002132 ) ) ;
#2030 = DIRECTION ( 'NONE',  ( -1.000000000000000000, 0.000000000000000000, 0.000000000000000000 ) ) ;
#2031 = CARTESIAN_POINT ( 'NONE',  ( 146.6084372240433709, -24.48358557860284179, -32.08495691632087699 ) ) ;
#2032 = CARTESIAN_POINT ( 'NONE',  ( 160.9163046357249129, -125.7889608577475684, -55.61140153332245006 ) ) ;
#2033 = VERTEX_POINT ( 'NONE', #21629 ) ;
#2034 = CARTESIAN_POINT ( 'NONE',  ( 199.9999999999999432, 12.28098720308154945, 14.50824971548827946 ) ) ;
#2035 = CARTESIAN_POINT ( 'NONE',  ( -105.3175882261749194, -18.50843658929550983, 10.85998092706852347 ) ) ;
#2036 = CARTESIAN_POINT ( 'NONE',  ( -3.439026802540597672, 17.93765581402023557, 43.30533194338860881 ) ) ;
#2037 = ORIENTED_EDGE ( 'NONE', *, *, #17908, .T. ) ;
#2038 = ORIENTED_EDGE ( 'NONE', *, *, #20881, .F. ) ;
#2039 = CARTESIAN_POINT ( 'NONE',  ( -162.0762913951020892, 1.694272876828294194, 0.000000000000000000 ) ) ;
#2040 = CARTESIAN_POINT ( 'NONE',  ( 199.0075387591496110, 2.605640672139595715, -19.82598477556707195 ) ) ;
#2041 = CARTESIAN_POINT ( 'NONE',  ( -199.9999999999999716, -82.49999999999991473, -52.49999999999977973 ) ) ;
#2042 = CARTESIAN_POINT ( 'NONE',  ( -162.0762913951020892, 1.198031840385716418, 1.198031840385750169 ) ) ;
#2043 = CARTESIAN_POINT ( 'NONE',  ( -102.4294859496168755, -8.407280617747138862, -20.29697089062620918 ) ) ;
#2044 = CARTESIAN_POINT ( 'NONE',  ( 184.8905102610680444, -1.851754852062639767E-13, 20.92133201514444352 ) ) ;
#2045 = CARTESIAN_POINT ( 'NONE',  ( 200.0000000000001990, -15.46007656673369368, 11.06691610098113543 ) ) ;
#2046 = CARTESIAN_POINT ( 'NONE',  ( -86.95455603114054099, -20.33687888584654857, -6.703476574496026963 ) ) ;
#2047 = CARTESIAN_POINT ( 'NONE',  ( -109.1264249741455643, -33.12752917268982600, 13.72187187124576191 ) ) ;
#2048 = CARTESIAN_POINT ( 'NONE',  ( 199.0248683625651154, -4.715036670046848677, 19.44145415004932076 ) ) ;
#2049 = CARTESIAN_POINT ( 'NONE',  ( -716.9846540392142060, 82.50000000000008527, 52.49999999999980105 ) ) ;
#2050 = CARTESIAN_POINT ( 'NONE',  ( 8.273828130702915118, -18.58906013839226645, -44.87796109789693588 ) ) ;
#2051 = CARTESIAN_POINT ( 'NONE',  ( 163.1118516004056573, 19.27778845539265618, -37.29075403953135037 ) ) ;
#2052 = CARTESIAN_POINT ( 'NONE',  ( -114.7826396787039727, 1.385190677998766828, -22.13135001985627426 ) ) ;
#2053 = CARTESIAN_POINT ( 'NONE',  ( -198.0356074513804572, -67.44298959250878056, 10.87444709758448447 ) ) ;
#2054 = LINE ( 'NONE', #16410, #18940 ) ;
#2055 = CARTESIAN_POINT ( 'NONE',  ( -238.4067589809705794, -0.6820004457913585449, -0.6820004457913265705 ) ) ;
#2056 = APPLICATION_CONTEXT ( 'automotive_design' ) ;
#2057 = CARTESIAN_POINT ( 'NONE',  ( -192.9588430854689705, -54.46834944099975928, -2.449293598294708485E-15 ) ) ;
#2058 = CARTESIAN_POINT ( 'NONE',  ( -259.2033419157646676, -6.730120644403663199, 6.730120644403451813 ) ) ;
#2059 = CARTESIAN_POINT ( 'NONE',  ( 192.4448373802101173, -19.99999999996056843, -40.00000000000002132 ) ) ;
#2060 = CARTESIAN_POINT ( 'NONE',  ( -105.3330350205445143, 18.67663213883233908, 10.55153823230807397 ) ) ;
#2061 = CARTESIAN_POINT ( 'NONE',  ( -192.9588430854690273, 40.00000000000014211, -14.46834944099927966 ) ) ;
#2062 = CARTESIAN_POINT ( 'NONE',  ( -135.8532207217289738, -6.472252184284190690, -6.472252184284188914 ) ) ;
#2063 = CARTESIAN_POINT ( 'NONE',  ( -259.2033419157646676, -9.517827891722680178, 0.000000000000000000 ) ) ;
#2064 = ORIENTED_EDGE ( 'NONE', *, *, #22985, .T. ) ;
#2065 = ORIENTED_EDGE ( 'NONE', *, *, #22233, .F. ) ;
#2066 = CARTESIAN_POINT ( 'NONE',  ( 200.0000000000000000, -20.00000000000006750, 40.00000000000002132 ) ) ;
#2067 = CARTESIAN_POINT ( 'NONE',  ( -94.58366989427226201, -8.190486896679201934, -20.91926462023907263 ) ) ;
#2068 = CARTESIAN_POINT ( 'NONE',  ( 192.4448373802101173, -40.00000000000005684, 19.99999999996046185 ) ) ;
#2069 = CARTESIAN_POINT ( 'NONE',  ( 91.82158438592158234, 44.40256751092319121, 12.16597498400105515 ) ) ;
#2070 = FACE_OUTER_BOUND ( 'NONE', #16181, .T. ) ;
#2071 = CARTESIAN_POINT ( 'NONE',  ( 180.0000000000000284, -115.7889608577475258, 82.50000000000000000 ) ) ;
#2072 = DIRECTION ( 'NONE',  ( -1.000000000000000000, -1.836970198721030181E-16, -2.465190328815661892E-32 ) ) ;
#2073 = CARTESIAN_POINT ( 'NONE',  ( 199.9999999999999716, 17.67160698027466736, 6.995183481556395577 ) ) ;
#2074 = CARTESIAN_POINT ( 'NONE',  ( 199.9999999999998863, -18.51554692031677973, -4.309913066855557418 ) ) ;
#2075 = CARTESIAN_POINT ( 'NONE',  ( -259.2033419157646676, -6.730120644402966867, -49.83842185052038332 ) ) ;
#2076 = CARTESIAN_POINT ( 'NONE',  ( -192.9588430854690273, -38.51493924976957572, 18.05360324515410397 ) ) ;
#2077 = LINE ( 'NONE', #4214, #17372 ) ;
#2078 = CARTESIAN_POINT ( 'NONE',  ( 4.995406935893290878, 1.606505379428369110E-13, -15.24977328854832592 ) ) ;
#2079 = CARTESIAN_POINT ( 'NONE',  ( 0.2972598230770153171, -66.70487387989849992, -10.13633138497533004 ) ) ;
#2080 = ADVANCED_FACE ( 'NONE', ( #23626 ), #8039, .T. ) ;
#2081 = LINE ( 'NONE', #16303, #1533 ) ;
#2082 = CARTESIAN_POINT ( 'NONE',  ( -192.9588430854690273, -66.79921049724377724, 10.23066800231950069 ) ) ;
#2083 = CARTESIAN_POINT ( 'NONE',  ( 199.0253317321493398, -6.507757088401906032, 18.91903323328891062 ) ) ;
#2084 = AXIS2_PLACEMENT_3D ( 'NONE', #2569, #12809, #10684 ) ;
#2086 = CARTESIAN_POINT ( 'NONE',  ( -238.4067589809705794, -1.892706720741712928E-13, 40.96449427998260973 ) ) ;
#2085 = CARTESIAN_POINT ( 'NONE',  ( -238.4067589809705794, 0.6820004458491113475, -57.25054294077229144 ) ) ;
#2087 = CARTESIAN_POINT ( 'NONE',  ( -162.0762913951021176, 57.76657433523994456, -1.198031840315424867 ) ) ;
#2088 = CARTESIAN_POINT ( 'NONE',  ( 20.17262239840771088, 43.80323544016827242, -18.14389419515791246 ) ) ;
#2089 = CARTESIAN_POINT ( 'NONE',  ( 0.2972598230769930017, 54.33493731733938148, -40.00000000000002132 ) ) ;
#2090 = ORIENTED_EDGE ( 'NONE', *, *, #2687, .T. ) ;
#2091 = CARTESIAN_POINT ( 'NONE',  ( -198.0356074513804572, 15.37879056873067007, 0.000000000000000000 ) ) ;
#2092 = CARTESIAN_POINT ( 'NONE',  ( -6.342283169552854538, -46.19215417244088684, 13.66521761902479248 ) ) ;
#2093 = CARTESIAN_POINT ( 'NONE',  ( 91.82158438592158234, -17.20528682183298486, 40.00000000000002132 ) ) ;
#2094 = ORIENTED_EDGE ( 'NONE', *, *, #16482, .F. ) ;
#2095 = CARTESIAN_POINT ( 'NONE',  ( -188.2995950289364941, -46.99046209955426434, -13.82811170417247126 ) ) ;
#2096 = CARTESIAN_POINT ( 'NONE',  ( 199.9999999999998579, -15.18157530797039101, 11.44282300742696457 ) ) ;
#2097 = CARTESIAN_POINT ( 'NONE',  ( -3.117754532603109308, -17.97158175134531533, 43.38723640139177462 ) ) ;
#2098 = EDGE_CURVE ( 'NONE', #3856, #1984, #3667, .T. ) ;
#2099 = CARTESIAN_POINT ( 'NONE',  ( -4.076660308449107539, 13.82548859978937550, -46.97758120990494035 ) ) ;
#2100 = CARTESIAN_POINT ( 'NONE',  ( 199.0125641721520822, -8.847877585088737007, -17.93749959268865979 ) ) ;
#2101 = CARTESIAN_POINT ( 'NONE',  ( 85.88498456125454084, -23.37206003943197175, 8.769910163431326566 ) ) ;
#2102 = CARTESIAN_POINT ( 'NONE',  ( -575.0231298121445889, 75.00000000000000000, 29.99999999999825206 ) ) ;
#2103 = CARTESIAN_POINT ( 'NONE',  ( -144.0562696877088626, -10.50947022284602994, 31.27040355063070365 ) ) ;
#2104 = CARTESIAN_POINT ( 'NONE',  ( -198.0356074513804572, 39.15871834505956173, -39.15871834505865223 ) ) ;
#2105 = CARTESIAN_POINT ( 'NONE',  ( 170.0000000000000000, 24.95097643317004454, 3.062538285713123809 ) ) ;
#2107 = CARTESIAN_POINT ( 'NONE',  ( -238.4067589809705794, 28.96627169325285678, 27.60227080167094726 ) ) ;
#2106 = CARTESIAN_POINT ( 'NONE',  ( -189.0115661350385494, 17.94954792649267716, -43.33404204260362746 ) ) ;
#2108 = CYLINDRICAL_SURFACE ( 'NONE', #18230, 31.79780246617542616 ) ;
#2109 = CARTESIAN_POINT ( 'NONE',  ( -280.0000000000000568, -20.00000000000007105, 40.00000000000002132 ) ) ;
#2110 = CARTESIAN_POINT ( 'NONE',  ( -259.2033419157646676, 30.48217210827735713, -40.00000000000002132 ) ) ;
#2111 = CARTESIAN_POINT ( 'NONE',  ( -280.0000000000000000, -2.609240458947769655E-13, 20.00000000000001421 ) ) ;
#2112 = CARTESIAN_POINT ( 'NONE',  ( 0.2972598230769907257, 66.70487387989857098, 10.13633138497486641 ) ) ;
#2113 = CARTESIAN_POINT ( 'NONE',  ( 98.29820294270298575, 18.47759065022021474, -7.653668647299666894 ) ) ;
#2114 = CARTESIAN_POINT ( 'NONE',  ( 184.8905102610680444, -13.49065550809791603, -13.49065550809818781 ) ) ;
#2115 = ORIENTED_EDGE ( 'NONE', *, *, #11409, .F. ) ;
#2116 = CARTESIAN_POINT ( 'NONE',  ( -208.1127848780264742, -17.67593391476659548, 38.89260858015730804 ) ) ;
#2117 = CARTESIAN_POINT ( 'NONE',  ( 200.0000000000000000, 57.47694228411675255, -64.52066607436459833 ) ) ;
#2118 = PRODUCT_CONTEXT ( 'NONE', #10201, 'mechanical' ) ;
#2119 = ORIENTED_EDGE ( 'NONE', *, *, #8406, .T. ) ;
#2120 = EDGE_LOOP ( 'NONE', ( #10499, #15535, #8500, #5942 ) ) ;
#2121 = CARTESIAN_POINT ( 'NONE',  ( -259.2033419157646676, -49.83842185052031937, -6.730120644403796426 ) ) ;
#2122 = CARTESIAN_POINT ( 'NONE',  ( 23.30336656375535398, -46.83484695576522228, -13.80490921643035307 ) ) ;
#2123 = ORIENTED_EDGE ( 'NONE', *, *, #23092, .F. ) ;
#2124 = CARTESIAN_POINT ( 'NONE',  ( -56.48582580120559982, 30.84685318188643777, -40.00000000000002132 ) ) ;
#2125 = FACE_BOUND ( 'NONE', #428, .T. ) ;
#2126 = CIRCLE ( 'NONE', #10610, 20.53474504356812247 ) ;
#2127 = ORIENTED_EDGE ( 'NONE', *, *, #14586, .T. ) ;
#2128 = CARTESIAN_POINT ( 'NONE',  ( 199.9999999999999432, 17.03543292729471403, 8.423468753378063667 ) ) ;
#2129 = DIRECTION ( 'NONE',  ( 1.000000000000000000, -1.836970198721030181E-16, -0.000000000000000000 ) ) ;
#2130 = CARTESIAN_POINT ( 'NONE',  ( 14.38125909742180220, 39.01709431150916885, -17.55144818341463164 ) ) ;
#2131 = CARTESIAN_POINT ( 'NONE',  ( -188.8948648269077921, -43.30399732969039661, -17.93710299892621052 ) ) ;
#2132 = CARTESIAN_POINT ( 'NONE',  ( -238.4067589809705794, -40.00000000000007105, 0.9644942799824426372 ) ) ;
#2133 = CARTESIAN_POINT ( 'NONE',  ( 130.8568914410475088, -34.05028731879786363, 40.00000000000002132 ) ) ;
#2134 = CARTESIAN_POINT ( 'NONE',  ( -135.8532207217289738, 21.81201906317798134, -21.81201906317747685 ) ) ;
#2135 = CARTESIAN_POINT ( 'NONE',  ( 199.0258842571097375, -9.142960865851959440, 17.79628948870135829 ) ) ;
#2136 = CARTESIAN_POINT ( 'NONE',  ( -100.7734535825088358, 6.065416334915073333E-14, -22.67402823373191723 ) ) ;
#2137 = CARTESIAN_POINT ( 'NONE',  ( 57.59792236341149163, -40.00000000000014211, 37.56421063658172699 ) ) ;
#2138 = CARTESIAN_POINT ( 'NONE',  ( -91.56559293963834989, 6.234561990864368500E-14, -22.67402823373191723 ) ) ;
#2139 = DIRECTION ( 'NONE',  ( 1.000000000000000000, 1.836970198721030427E-16, -0.000000000000000000 ) ) ;
#2140 = CARTESIAN_POINT ( 'NONE',  ( 19.06497207195982924, -66.60410523465823474, 10.03556273973400081 ) ) ;
#2141 = CARTESIAN_POINT ( 'NONE',  ( -238.4067589809705794, -0.9644942799826262680, 0.000000000000000000 ) ) ;
#2142 = CARTESIAN_POINT ( 'NONE',  ( -105.3755690713226585, 15.38646221621762678, 41.18208027870604582 ) ) ;
#2143 = FACE_BOUND ( 'NONE', #4565, .T. ) ;
#2144 = AXIS2_PLACEMENT_3D ( 'NONE', #13336, #11585, #19580 ) ;
#2145 = CARTESIAN_POINT ( 'NONE',  ( -1.258540240222666418, -47.88180740053034157, 13.96099832920793737 ) ) ;
#2146 = CARTESIAN_POINT ( 'NONE',  ( 163.1118516004056573, -2.556006622855449647E-13, 27.26290988616872824 ) ) ;
#2147 = CARTESIAN_POINT ( 'NONE',  ( 57.59792236341147742, -1.230234673553095937E-13, 37.56421063658186199 ) ) ;
#2148 = CARTESIAN_POINT ( 'NONE',  ( -105.3755690713226585, 41.18208027870598187, -15.38646221621779731 ) ) ;
#2149 = CARTESIAN_POINT ( 'NONE',  ( -114.6238578290137724, 19.10716134690576595, 10.97953394730984478 ) ) ;
#2150 = CARTESIAN_POINT ( 'NONE',  ( -190.5535808404531508, -18.10342626499672036, -43.70553721438312778 ) ) ;
#2151 = CARTESIAN_POINT ( 'NONE',  ( -56.48582580120558561, -21.81201906317785699, 21.81201906317761896 ) ) ;
#2152 = VERTEX_POINT ( 'NONE', #16029 ) ;
#2153 = CARTESIAN_POINT ( 'NONE',  ( -100.7734535825088358, -16.03295912088728770, 16.03295912088687913 ) ) ;
#2154 = FACE_OUTER_BOUND ( 'NONE', #25295, .T. ) ;
#2155 = CARTESIAN_POINT ( 'NONE',  ( 184.8905102610680444, 20.92133201514447549, 0.000000000000000000 ) ) ;
#2156 = ADVANCED_FACE ( 'NONE', ( #21760 ), #12275, .T. ) ;
#2157 =( BOUNDED_SURFACE ( )  B_SPLINE_SURFACE ( 3, 3, ( 
 ( #5865, #2020, #20371, #7713, #4015, #3881, #1617, #18223, #15824, #12115, #13971, #8121, #10122, #6130, #19966, #10, #16238, #13833, #24367, #14112, #23954, #9724, #13708, #21968, #1882, #2146, #20105, #9986, #5601, #19831 ),
 ( #3602, #15965, #3740, #7843, #1747, #7981, #18097, #11711, #9855, #24231, #4154, #6004, #21833, #22378, #20239, #17694, #12249, #7583, #15695, #23819, #4285, #16761, #6784, #24764, #4674, #22507, #2681, #6387, #12776, #4545 ),
 ( #21030, #22765, #2406, #18898, #22634, #6650, #20631, #22895, #8653, #14765, #16899, #14374, #18365, #20903, #12643, #8517, #14503, #20768, #2538, #145, #10383, #10516, #16504, #14896, #18630, #10656, #413, #25031, #6261, #10788 ),
 ( #23036, #4409, #18765, #24629, #12503, #4811, #16635, #6517, #8249, #10256, #16366, #677, #14628, #549, #12913, #8786, #24500, #24895, #12374, #20502, #2274, #18494, #274, #8382, #8918, #7418, #19284, #13046, #13294, #23661 ),
 ( #1067, #7047, #21415, #15285, #19033, #2937, #3066, #9051, #25672, #11168, #5192, #13171, #17534, #25163, #5307, #21542, #812, #6914, #15031, #13542, #942, #15533, #17287, #17027, #5441, #17156, #5065, #23536, #3188, #3316 ),
 ( #25549, #15411, #2812, #13419, #23161, #10921, #9303, #9427, #23289, #4940, #21164, #17407, #7169, #11047, #23416, #19158, #11296, #9174, #25421, #11414, #25290, #15164, #7297, #19414, #21292, #19536, #1198, #1322, #9823, #12080 ),
 ( #15924, #3844, #7808, #9551, #11810, #5833, #23787, #19664, #13936, #26212, #15661, #9952, #19796, #11540, #1713, #3568, #22071, #10087, #7549, #19930, #21796, #3708, #7679, #11948, #20073, #5568, #15791, #25937, #8084, #11672 ) ),
 .UNSPECIFIED., .T., .F., .F. ) 
 B_SPLINE_SURFACE_WITH_KNOTS ( ( 4, 3, 4 ),
 ( 4, 2, 2, 2, 2, 2, 2, 2, 2, 2, 2, 2, 2, 2, 4 ),
 ( 0.000000000000000000, 0.5000000000000000000, 1.000000000000000000 ),
 ( 0.000000000000000000, 0.1357259735107005372, 0.1651108541090157700, 0.1944957347073310028, 0.3598804999793158710, 0.3867117631979620773, 0.4135430264166082281, 0.5789277916885930964, 0.6062785021374117456, 0.6336292125862302838, 0.8508620842112317728, 0.8814014469398914198, 0.9119408096685510667, 0.9559704048342755334, 1.000000000000000000 ),
 .UNSPECIFIED. ) 
 GEOMETRIC_REPRESENTATION_ITEM ( )  RATIONAL_B_SPLINE_SURFACE ( (
 ( 1.000000000000000000, 1.000000000000000000, 1.000000000000000000, 1.000000000000000000, 1.000000000000000000, 1.000000000000000000, 1.000000000000000000, 1.000000000000000000, 1.000000000000000000, 1.000000000000000000, 1.000000000000000000, 1.000000000000000000, 1.000000000000000000, 1.000000000000000000, 1.000000000000000000, 1.000000000000000000, 1.000000000000000000, 1.000000000000000000, 1.000000000000000000, 1.000000000000000000, 1.000000000000000000, 1.000000000000000000, 1.000000000000000000, 1.000000000000000000, 1.000000000000000000, 1.000000000000000000, 1.000000000000000000, 1.000000000000000000, 1.000000000000000000, 1.000000000000000000),
 ( 0.3333333333333333703, 0.3333333333333333703, 0.3333333333333333703, 0.3333333333333333703, 0.3333333333333333703, 0.3333333333333333703, 0.3333333333333333703, 0.3333333333333333703, 0.3333333333333333703, 0.3333333333333333703, 0.3333333333333333703, 0.3333333333333333703, 0.3333333333333333703, 0.3333333333333333703, 0.3333333333333333703, 0.3333333333333333703, 0.3333333333333333703, 0.3333333333333333703, 0.3333333333333333703, 0.3333333333333333703, 0.3333333333333333703, 0.3333333333333333703, 0.3333333333333333703, 0.3333333333333333703, 0.3333333333333333703, 0.3333333333333333703, 0.3333333333333333703, 0.3333333333333333703, 0.3333333333333333703, 0.3333333333333333703),
 ( 0.3333333333333333703, 0.3333333333333333703, 0.3333333333333333703, 0.3333333333333333703, 0.3333333333333333703, 0.3333333333333333703, 0.3333333333333333703, 0.3333333333333333703, 0.3333333333333333703, 0.3333333333333333703, 0.3333333333333333703, 0.3333333333333333703, 0.3333333333333333703, 0.3333333333333333703, 0.3333333333333333703, 0.3333333333333333703, 0.3333333333333333703, 0.3333333333333333703, 0.3333333333333333703, 0.3333333333333333703, 0.3333333333333333703, 0.3333333333333333703, 0.3333333333333333703, 0.3333333333333333703, 0.3333333333333333703, 0.3333333333333333703, 0.3333333333333333703, 0.3333333333333333703, 0.3333333333333333703, 0.3333333333333333703),
 ( 1.000000000000000000, 1.000000000000000000, 1.000000000000000000, 1.000000000000000000, 1.000000000000000000, 1.000000000000000000, 1.000000000000000000, 1.000000000000000000, 1.000000000000000000, 1.000000000000000000, 1.000000000000000000, 1.000000000000000000, 1.000000000000000000, 1.000000000000000000, 1.000000000000000000, 1.000000000000000000, 1.000000000000000000, 1.000000000000000000, 1.000000000000000000, 1.000000000000000000, 1.000000000000000000, 1.000000000000000000, 1.000000000000000000, 1.000000000000000000, 1.000000000000000000, 1.000000000000000000, 1.000000000000000000, 1.000000000000000000, 1.000000000000000000, 1.000000000000000000),
 ( 0.3333333333333333703, 0.3333333333333333703, 0.3333333333333333703, 0.3333333333333333703, 0.3333333333333333703, 0.3333333333333333703, 0.3333333333333333703, 0.3333333333333333703, 0.3333333333333333703, 0.3333333333333333703, 0.3333333333333333703, 0.3333333333333333703, 0.3333333333333333703, 0.3333333333333333703, 0.3333333333333333703, 0.3333333333333333703, 0.3333333333333333703, 0.3333333333333333703, 0.3333333333333333703, 0.3333333333333333703, 0.3333333333333333703, 0.3333333333333333703, 0.3333333333333333703, 0.3333333333333333703, 0.3333333333333333703, 0.3333333333333333703, 0.3333333333333333703, 0.3333333333333333703, 0.3333333333333333703, 0.3333333333333333703),
 ( 0.3333333333333333703, 0.3333333333333333703, 0.3333333333333333703, 0.3333333333333333703, 0.3333333333333333703, 0.3333333333333333703, 0.3333333333333333703, 0.3333333333333333703, 0.3333333333333333703, 0.3333333333333333703, 0.3333333333333333703, 0.3333333333333333703, 0.3333333333333333703, 0.3333333333333333703, 0.3333333333333333703, 0.3333333333333333703, 0.3333333333333333703, 0.3333333333333333703, 0.3333333333333333703, 0.3333333333333333703, 0.3333333333333333703, 0.3333333333333333703, 0.3333333333333333703, 0.3333333333333333703, 0.3333333333333333703, 0.3333333333333333703, 0.3333333333333333703, 0.3333333333333333703, 0.3333333333333333703, 0.3333333333333333703),
 ( 1.000000000000000000, 1.000000000000000000, 1.000000000000000000, 1.000000000000000000, 1.000000000000000000, 1.000000000000000000, 1.000000000000000000, 1.000000000000000000, 1.000000000000000000, 1.000000000000000000, 1.000000000000000000, 1.000000000000000000, 1.000000000000000000, 1.000000000000000000, 1.000000000000000000, 1.000000000000000000, 1.000000000000000000, 1.000000000000000000, 1.000000000000000000, 1.000000000000000000, 1.000000000000000000, 1.000000000000000000, 1.000000000000000000, 1.000000000000000000, 1.000000000000000000, 1.000000000000000000, 1.000000000000000000, 1.000000000000000000, 1.000000000000000000, 1.000000000000000000) ) ) 
 REPRESENTATION_ITEM ( '' )  SURFACE ( )  );
#2158 = CARTESIAN_POINT ( 'NONE',  ( -87.13361725327075646, 15.19799821270843765, 15.19799821270837015 ) ) ;
#2159 = CARTESIAN_POINT ( 'NONE',  ( -105.3755690713226727, -15.38646221621807619, 15.38646221621768362 ) ) ;
#2160 = EDGE_LOOP ( 'NONE', ( #12063, #8625, #3993, #6401, #1324 ) ) ;
#2161 = ORIENTED_EDGE ( 'NONE', *, *, #13851, .F. ) ;
#2162 = CARTESIAN_POINT ( 'NONE',  ( 200.0000000000000000, 9.495512316542487952, 16.46764514154290637 ) ) ;
#2163 = DIRECTION ( 'NONE',  ( 0.8802361161597900274, 0.000000000000000000, -0.4745359626076074422 ) ) ;
#2164 = CARTESIAN_POINT ( 'NONE',  ( 3.774039766383602945, 18.47898247162966356, 44.61221010184721081 ) ) ;
#2165 = ADVANCED_FACE ( 'NONE', ( #7613 ), #14146, .F. ) ;
#2166 = EDGE_LOOP ( 'NONE', ( #25011, #25719, #18779, #2522 ) ) ;
#2167 = EDGE_LOOP ( 'NONE', ( #7931, #12834, #17870, #16767 ) ) ;
#2168 = CARTESIAN_POINT ( 'NONE',  ( -238.4067589809705794, 0.9644942799825386714, 0.000000000000000000 ) ) ;
#2169 = CARTESIAN_POINT ( 'NONE',  ( 199.0057329523134513, 9.713090712928652337, -17.48024697358846069 ) ) ;
#2170 = CARTESIAN_POINT ( 'NONE',  ( -110.1017833367309890, -1.261434661933622303, -20.19517362623882306 ) ) ;
#2171 = EDGE_CURVE ( 'NONE', #24112, #7498, #20193, .T. ) ;
#2172 = ADVANCED_FACE ( 'NONE', ( #22935 ), #6425, .F. ) ;
#2173 = CARTESIAN_POINT ( 'NONE',  ( 48.46046611906923118, 37.63122027851007090, -11.89583623498074161 ) ) ;
#2174 = DIRECTION ( 'NONE',  ( 0.000000000000000000, 0.000000000000000000, 1.000000000000000000 ) ) ;
#2175 = CARTESIAN_POINT ( 'NONE',  ( 170.2234770963711128, 40.00000000000021316, -15.44714144992773797 ) ) ;
#2176 = CARTESIAN_POINT ( 'NONE',  ( 199.9999999999998863, -17.44218472118251384, 7.566354988273278792 ) ) ;
#2177 = CARTESIAN_POINT ( 'NONE',  ( -654.1659037529333318, 37.93148257888354635, 12.70525021040782754 ) ) ;
#2178 = CARTESIAN_POINT ( 'NONE',  ( -190.0000000000000000, 66.50000000000009948, 66.50000000000005684 ) ) ;
#2179 = CARTESIAN_POINT ( 'NONE',  ( 199.0212010157159455, 5.167062836304152640, 19.32642926518865423 ) ) ;
#2180 = DIRECTION ( 'NONE',  ( -1.000000000000000000, 0.000000000000000000, 0.000000000000000000 ) ) ;
#2181 = CARTESIAN_POINT ( 'NONE',  ( 11.28112952480041820, -18.58737866929310201, -44.87390167242637773 ) ) ;
#2182 = CARTESIAN_POINT ( 'NONE',  ( 0.2972598230770153171, -66.70487387989849992, -10.13633138497533004 ) ) ;
#2183 = CARTESIAN_POINT ( 'NONE',  ( -110.0368417077420418, 7.441767003006856562, -18.74474319002892031 ) ) ;
#2184 = CARTESIAN_POINT ( 'NONE',  ( 170.2234770963711128, -39.20704971665379190, -17.36149277827012938 ) ) ;
#2185 = CARTESIAN_POINT ( 'NONE',  ( -77.71518870763448206, 21.27450625603104939, 5.747100446277157104 ) ) ;
#2186 = VECTOR ( 'NONE', #25982, 1000.000000000000000 ) ;
#2187 = FACE_BOUND ( 'NONE', #25625, .T. ) ;
#2188 = CARTESIAN_POINT ( 'NONE',  ( -238.4067589809705794, -40.96449428006345528, 40.00000000000002132 ) ) ;
#2189 = CARTESIAN_POINT ( 'NONE',  ( 146.6084372240433993, 24.48358557860341733, -24.48358557860313311 ) ) ;
#2190 = AXIS2_PLACEMENT_3D ( 'NONE', #6287, #4316, #22000 ) ;
#2191 = CARTESIAN_POINT ( 'NONE',  ( -213.1075012329536946, -53.71589010951918652, -2.449293598294708485E-15 ) ) ;
#2192 = CARTESIAN_POINT ( 'NONE',  ( -105.2410663018207373, 17.15223596101294490, 12.91571364855967907 ) ) ;
#2193 = CIRCLE ( 'NONE', #17641, 10.00000000000000888 ) ;
#2194 = CARTESIAN_POINT ( 'NONE',  ( -213.1075012329537230, 40.00000000000055422, -53.71589010953623244 ) ) ;
#2195 = CARTESIAN_POINT ( 'NONE',  ( 0.2972598230769938343, 10.13633138497472252, 10.13633138497475628 ) ) ;
#2196 = CARTESIAN_POINT ( 'NONE',  ( -86.96347745069644475, -21.75974354311651737, 0.000000000000000000 ) ) ;
#2197 = ORIENTED_EDGE ( 'NONE', *, *, #2296, .F. ) ;
#2198 = ORIENTED_EDGE ( 'NONE', *, *, #19384, .F. ) ;
#2199 = CARTESIAN_POINT ( 'NONE',  ( 14.38125909742180752, 15.17850393972634038, 0.000000000000000000 ) ) ;
#2200 = CARTESIAN_POINT ( 'NONE',  ( -188.2995950289364089, -23.44932284465861727, -43.00522595870986464 ) ) ;
#2201 = AXIS2_PLACEMENT_3D ( 'NONE', #2794, #2665, #8636 ) ;
#2202 = CARTESIAN_POINT ( 'NONE',  ( -280.0000000000000568, 42.42640687119265408, 14.14213562373147504 ) ) ;
#2203 = CARTESIAN_POINT ( 'NONE',  ( -192.9588430854689989, 14.46834944099965981, 0.000000000000000000 ) ) ;
#2204 = FACE_OUTER_BOUND ( 'NONE', #13398, .T. ) ;
#2205 = CARTESIAN_POINT ( 'NONE',  ( -726.9846540392142060, -52.49999999999991473, 82.49999999999998579 ) ) ;
#2206 = CARTESIAN_POINT ( 'NONE',  ( 199.9999999999997442, 18.75350838795884201, -3.072479883316599381 ) ) ;
#2207 = CARTESIAN_POINT ( 'NONE',  ( 199.9999999999999147, -11.57906590988528528, -15.07304842808868273 ) ) ;
#2208 = CARTESIAN_POINT ( 'NONE',  ( -238.4067589809705794, 28.96627169325354956, -28.96627169325289231 ) ) ;
#2209 = CARTESIAN_POINT ( 'NONE',  ( -56.48582580120559982, -21.81201906317804173, 34.75652343174591152 ) ) ;
#2210 = CARTESIAN_POINT ( 'NONE',  ( -280.0000000000000000, -5.143516556418885689E-14, 0.000000000000000000 ) ) ;
#2211 = CARTESIAN_POINT ( 'NONE',  ( -259.2033419157646676, 39.99999999999987921, 9.517827891723049660 ) ) ;
#2212 = CARTESIAN_POINT ( 'NONE',  ( 136.1360204305621266, -3.511608612530630058, -3.511608612530719764 ) ) ;
#2213 = DIRECTION ( 'NONE',  ( 1.000000000000000000, 0.000000000000000000, 0.000000000000000000 ) ) ;
#2214 = CARTESIAN_POINT ( 'NONE',  ( 4.995406935893289102, 10.78321810388998081, 10.78321810389001811 ) ) ;
#2215 = CARTESIAN_POINT ( 'NONE',  ( 19.06497207195981147, -10.03556273973439517, 10.03556273973429214 ) ) ;
#2216 = CARTESIAN_POINT ( 'NONE',  ( 199.0260505877926960, -10.07036125175988772, 17.33556466753674385 ) ) ;
#2218 = CARTESIAN_POINT ( 'NONE',  ( 146.6084372240433709, -40.00000000000001421, 5.374981219216829587 ) ) ;
#2217 = CARTESIAN_POINT ( 'NONE',  ( 19.06497207195980792, 66.60410523465830579, -10.03556273973354251 ) ) ;
#2219 = CARTESIAN_POINT ( 'NONE',  ( -198.0356074513804572, 39.15871834505887250, 17.40982414986519089 ) ) ;
#2220 = VECTOR ( 'NONE', #5945, 1000.000000000000000 ) ;
#2221 = CARTESIAN_POINT ( 'NONE',  ( 22.72189371636483557, 47.04833883278845974, -13.83659596078922682 ) ) ;
#2222 = CARTESIAN_POINT ( 'NONE',  ( -135.8532207217289738, 30.84685318188643777, -40.00000000000002132 ) ) ;
#2223 = CARTESIAN_POINT ( 'NONE',  ( 0.2972598230769930572, 14.33493731733933352, 0.000000000000000000 ) ) ;
#2224 = CARTESIAN_POINT ( 'NONE',  ( -4.082462733454207182, -42.99255347688252726, 23.44093842354193313 ) ) ;
#2225 = CARTESIAN_POINT ( 'NONE',  ( 4.995406935893288214, 15.24977328854832770, 40.00000000000002132 ) ) ;
#2226 = VERTEX_POINT ( 'NONE', #12412 ) ;
#2227 = DIRECTION ( 'NONE',  ( -1.000000000000000000, -1.836970198721030181E-16, 0.000000000000000000 ) ) ;
#2228 = CARTESIAN_POINT ( 'NONE',  ( 192.4448373802100889, -14.14213562375876698, -14.14213562375885047 ) ) ;
#2229 = CARTESIAN_POINT ( 'NONE',  ( -70.28815428291109413, -9.450978460797621494, 22.81668038719991998 ) ) ;
#2230 = CARTESIAN_POINT ( 'NONE',  ( -4.121597284766290059, 23.43330939486714470, -42.98102224344789590 ) ) ;
#2231 = CARTESIAN_POINT ( 'NONE',  ( 199.0178460907175690, -16.45326163792621443, -11.37340206338170923 ) ) ;
#2232 = CARTESIAN_POINT ( 'NONE',  ( -114.4364955367336449, 20.04994829326807348, -8.644468109231272734 ) ) ;
#2233 = CARTESIAN_POINT ( 'NONE',  ( 146.5090579137182090, -29.94463907179424211, 12.40347562390428138 ) ) ;
#2234 = CARTESIAN_POINT ( 'NONE',  ( -183.1091233172535624, -13.45963571007644610, 45.18843800009203449 ) ) ;
#2235 = CARTESIAN_POINT ( 'NONE',  ( -105.3755690713226727, -15.38646221621807619, 15.38646221621768362 ) ) ;
#2236 = CARTESIAN_POINT ( 'NONE',  ( 170.2234770963711128, 24.55285855007190321, 0.000000000000000000 ) ) ;
#2238 = CARTESIAN_POINT ( 'NONE',  ( -208.1127848780265026, 10.60833733269551615, -10.60833733269529766 ) ) ;
#2237 = CARTESIAN_POINT ( 'NONE',  ( -193.3669098795969319, 18.32287322059355361, -44.23532903078456968 ) ) ;
#2239 = CARTESIAN_POINT ( 'NONE',  ( 146.6084372240433709, 3.800685668858042821, 52.76785682606522698 ) ) ;
#2240 = EDGE_CURVE ( 'NONE', #218, #23932, #5326, .T. ) ;
#2241 = CARTESIAN_POINT ( 'NONE',  ( 184.8905102610680444, -19.07866798485555293, -2.449293598294708485E-15 ) ) ;
#2242 = CARTESIAN_POINT ( 'NONE',  ( -91.56559293963834989, 17.32597176626809343, 2.449293598294708485E-15 ) ) ;
#2243 = CARTESIAN_POINT ( 'NONE',  ( 14.38125909742181818, -39.99999999999986500, -15.17850393972675604 ) ) ;
#2244 = CARTESIAN_POINT ( 'NONE',  ( 130.8568914410475372, 4.207082182992862407, 4.207082182992856190 ) ) ;
#2245 = CARTESIAN_POINT ( 'NONE',  ( -99.31364972222439746, 20.79869444142039470, -8.164808577100629350 ) ) ;
#2246 = CARTESIAN_POINT ( 'NONE',  ( 0.2972598230770100991, -38.42060263243632079, -38.42060263243699580 ) ) ;
#2247 = ORIENTED_EDGE ( 'NONE', *, *, #16442, .F. ) ;
#2248 = CARTESIAN_POINT ( 'NONE',  ( -198.0356074513804572, -17.40982414986482141, 39.15871834505909987 ) ) ;
#2249 = CARTESIAN_POINT ( 'NONE',  ( -190.0000000000000000, -52.49999999999992895, -52.49999999999999289 ) ) ;
#2250 = CARTESIAN_POINT ( 'NONE',  ( -91.56559293963834989, -12.25131212657492874, 12.25131212657477953 ) ) ;
#2251 = CARTESIAN_POINT ( 'NONE',  ( -3.205219349396362993, -43.36521377095327523, -17.96245967913666064 ) ) ;
#2252 = EDGE_CURVE ( 'NONE', #6112, #5576, #6594, .T. ) ;
#2253 = ORIENTED_EDGE ( 'NONE', *, *, #21362, .T. ) ;
#2254 = CARTESIAN_POINT ( 'NONE',  ( 18.90082769090740555, -48.20711988125818692, -14.00978943384287767 ) ) ;
#2255 = DIRECTION ( 'NONE',  ( 1.836970198721030181E-16, 1.000000000000000000, 0.000000000000000000 ) ) ;
#2257 = EDGE_LOOP ( 'NONE', ( #16312, #18069, #19048, #6656 ) ) ;
#2256 = EDGE_CURVE ( 'NONE', #18680, #16217, #11268, .T. ) ;
#2258 = CARTESIAN_POINT ( 'NONE',  ( 200.0000000000001137, 17.30391983412833667, 7.856783789979721710 ) ) ;
#2259 = CYLINDRICAL_SURFACE ( 'NONE', #10711, 69.99999999999994316 ) ;
#2260 = CARTESIAN_POINT ( 'NONE',  ( 130.8568914410475372, -24.07718906447222551, -24.07718906447233209 ) ) ;
#2261 = CARTESIAN_POINT ( 'NONE',  ( -188.9478905404515103, -43.31768569177536676, -17.94277290414884618 ) ) ;
#2262 = CARTESIAN_POINT ( 'NONE',  ( 151.7948205124836534, -40.00000000000001421, 6.767089262348889633 ) ) ;
#2263 = CARTESIAN_POINT ( 'NONE',  ( -30.26275506840324425, 41.69427246844627177, 40.00000000000002132 ) ) ;
#2264 = CARTESIAN_POINT ( 'NONE',  ( 4.995406935893294431, -17.50105314357144337, -39.06748935135212264 ) ) ;
#2265 = DIRECTION ( 'NONE',  ( -1.000000000000000000, -1.836970198721030181E-16, -2.465190328815661892E-32 ) ) ;
#2266 = CARTESIAN_POINT ( 'NONE',  ( -192.9588430854689989, -8.596193650988133061E-14, 14.46834944099969533 ) ) ;
#2267 = CARTESIAN_POINT ( 'NONE',  ( -162.0762913951021176, -40.00000000000019895, 41.69427287672974813 ) ) ;
#2268 = CARTESIAN_POINT ( 'NONE',  ( 4.995406935893290878, -5.232665749138292703E-14, 15.24977328854832592 ) ) ;
#2269 = FACE_OUTER_BOUND ( 'NONE', #1728, .T. ) ;
#2270 = CARTESIAN_POINT ( 'NONE',  ( -259.2033419157646676, -30.48217210827744950, 40.00000000000002132 ) ) ;
#2271 = CARTESIAN_POINT ( 'NONE',  ( 14.38125909742182529, -39.01709431150933938, 39.01709431150894147 ) ) ;
#2272 = CARTESIAN_POINT ( 'NONE',  ( 130.8888609958233076, -12.21841679119707891, -29.49786752803538548 ) ) ;
#2273 = PLANE ( 'NONE',  #23836 ) ;
#2274 = CARTESIAN_POINT ( 'NONE',  ( 91.82158438592158234, 2.580785920671402147E-13, -22.79471317813470321 ) ) ;
#2275 = CARTESIAN_POINT ( 'NONE',  ( 163.1118516004056573, -1.695744499706194789E-14, 12.73709011382475254 ) ) ;
#2276 = CARTESIAN_POINT ( 'NONE',  ( 91.82158438592158234, 16.11829626346139577, 16.11829626346143840 ) ) ;
#2277 = LINE ( 'NONE', #10386, #3682 ) ;
#2278 = CARTESIAN_POINT ( 'NONE',  ( -89.92902785008709543, -8.734793929541330826, -20.17328762787300533 ) ) ;
#2279 = CARTESIAN_POINT ( 'NONE',  ( 130.8568914410475088, -32.49135343045460900, -24.07718906446924478 ) ) ;
#2280 = EDGE_LOOP ( 'NONE', ( #12322, #25337 ) ) ;
#2281 = CARTESIAN_POINT ( 'NONE',  ( 136.1360204305621551, -53.05693388239309627, -3.511608612531332163 ) ) ;
#2282 = CARTESIAN_POINT ( 'NONE',  ( 133.2080217031555378, 29.90338805389124488, -12.38638889282725408 ) ) ;
#2283 = CARTESIAN_POINT ( 'NONE',  ( 4.995406935893307754, -55.24977328854835434, -2.449293598294708485E-15 ) ) ;
#2284 = CARTESIAN_POINT ( 'NONE',  ( -105.3220356878035915, 10.86389608387957395, 18.46482525816570330 ) ) ;
#2285 = DIRECTION ( 'NONE',  ( -1.000000000000000000, 0.000000000000000000, 0.000000000000000000 ) ) ;
#2286 = ORIENTED_EDGE ( 'NONE', *, *, #15342, .T. ) ;
#2287 = EDGE_LOOP ( 'NONE', ( #15332, #4523, #9187, #4693 ) ) ;
#2288 = CARTESIAN_POINT ( 'NONE',  ( 199.9999999999999147, 18.96428544249645043, -1.225771028434774923 ) ) ;
#2289 = CARTESIAN_POINT ( 'NONE',  ( 5.823571940223288834, 14.15488761396325046, 49.16771748719407498 ) ) ;
#2290 = ORIENTED_EDGE ( 'NONE', *, *, #15245, .T. ) ;
#2291 = ORIENTED_EDGE ( 'NONE', *, *, #1024, .F. ) ;
#2292 = CARTESIAN_POINT ( 'NONE',  ( -198.0356074513804572, 15.37879056873067007, 0.000000000000000000 ) ) ;
#2293 = CARTESIAN_POINT ( 'NONE',  ( 199.0060750228415429, 7.941611777091910795, -18.35102805502410561 ) ) ;
#2294 = CARTESIAN_POINT ( 'NONE',  ( -259.2033419157646676, 49.83842185052027673, -6.730120644403441155 ) ) ;
#2295 = CARTESIAN_POINT ( 'NONE',  ( -196.0240701155048271, -24.63338802315931986, 44.60678452943332672 ) ) ;
#2296 = EDGE_CURVE ( 'NONE', #858, #22654, #8641, .T. ) ;
#2297 = CARTESIAN_POINT ( 'NONE',  ( -280.0000000000000000, -5.143516556418885689E-14, 0.000000000000000000 ) ) ;
#2298 = CARTESIAN_POINT ( 'NONE',  ( -86.96347745069645896, 40.00000000000019895, -18.24025645688310249 ) ) ;
#2299 = VECTOR ( 'NONE', #14052, 1000.000000000000000 ) ;
#2300 = CARTESIAN_POINT ( 'NONE',  ( -238.4067589809705794, 39.99999999999999289, -0.9644942799821634161 ) ) ;
#2301 = CARTESIAN_POINT ( 'NONE',  ( -655.8941833601360258, 39.18869065112085082, 8.031053782042897993 ) ) ;
#2302 = DIRECTION ( 'NONE',  ( 1.000000000000000000, 1.836970198721030427E-16, -0.000000000000000000 ) ) ;
#2303 = CARTESIAN_POINT ( 'NONE',  ( 199.0201394418415077, 7.332745681712491859, 18.61237044096938575 ) ) ;
#2304 = CARTESIAN_POINT ( 'NONE',  ( -188.2652133075138750, 13.82568790539370163, 46.97855991888750538 ) ) ;
#2305 = CARTESIAN_POINT ( 'NONE',  ( -198.0356074513804572, -39.15871834505931304, 17.40982414986437377 ) ) ;
#2306 =( BOUNDED_SURFACE ( )  B_SPLINE_SURFACE ( 3, 2, ( 
 ( #6998, #503, #23250 ),
 ( #24851, #15119, #4765 ),
 ( #13003, #23121, #14590 ),
 ( #22718, #12869, #16985 ),
 ( #2635, #13132, #18855 ),
 ( #635, #6603, #24990 ),
 ( #20987, #2768, #20728 ),
 ( #18718, #10877, #18589 ),
 ( #11007, #19117, #18992 ),
 ( #25122, #900, #769 ) ),
 .UNSPECIFIED., .F., .F., .T. ) 
 B_SPLINE_SURFACE_WITH_KNOTS ( ( 4, 2, 2, 2, 4 ),
 ( 3, 3 ),
 ( 0.04143701731398998639, 0.04847035109443004197, 0.05022868453954006107, 0.05198701798465007323, 0.05550368487487010449 ),
 ( 0.000000000000000000, 1.000000000000000000 ),
 .UNSPECIFIED. ) 
 GEOMETRIC_REPRESENTATION_ITEM ( )  RATIONAL_B_SPLINE_SURFACE ( (
 ( 1.000000000000000000, 0.9541700779530608578, 1.000000000000000000),
 ( 1.000000000000000000, 0.9520138072637328586, 1.000000000000000000),
 ( 1.000000000000000000, 0.9503242346237325000, 1.000000000000000000),
 ( 1.000000000000000000, 0.9488844900981833197, 1.000000000000000000),
 ( 1.000000000000000000, 0.9486296596067500531, 1.000000000000000000),
 ( 1.000000000000000000, 0.9481942170211148380, 1.000000000000000000),
 ( 1.000000000000000000, 0.9480132043934548225, 1.000000000000000000),
 ( 1.000000000000000000, 0.9475791817277525730, 1.000000000000000000),
 ( 1.000000000000000000, 0.9474351099636038054, 1.000000000000000000),
 ( 1.000000000000000000, 0.9474350314971538012, 1.000000000000000000) ) ) 
 REPRESENTATION_ITEM ( '' )  SURFACE ( )  );
#2307 = CARTESIAN_POINT ( 'NONE',  ( -114.6380096433489797, -11.20642776433569665, -18.98727595036316984 ) ) ;
#2308 = CARTESIAN_POINT ( 'NONE',  ( -86.96347745069645896, 43.67073346367970288, 12.89780903124427702 ) ) ;
#2309 = CARTESIAN_POINT ( 'NONE',  ( -77.70130000790294389, 5.505113979798187174, 21.34877220993403313 ) ) ;
#2310 = CARTESIAN_POINT ( 'NONE',  ( 0.2972598230770048811, -10.13633138497415942, -66.70487387989865624 ) ) ;
#2311 = CARTESIAN_POINT ( 'NONE',  ( -660.6855337863669320, 43.99654503343406020, 9.519970529664389502 ) ) ;
#2312 = CARTESIAN_POINT ( 'NONE',  ( -91.56559293963836410, 22.67402823373190301, 40.00000000000002132 ) ) ;
#2313 = EDGE_CURVE ( 'NONE', #25993, #2419, #22542, .T. ) ;
#2314 = CARTESIAN_POINT ( 'NONE',  ( -105.3755690713226727, -15.38646221621807619, 15.38646221621768362 ) ) ;
#2315 = CARTESIAN_POINT ( 'NONE',  ( 184.8905102610680444, 20.92133201514447194, 40.00000000000002132 ) ) ;
#2316 = CARTESIAN_POINT ( 'NONE',  ( -110.0880539878520352, 16.49558164034374741, 11.64549321196552256 ) ) ;
#2317 = CARTESIAN_POINT ( 'NONE',  ( 91.82158438592156813, 40.00000000000027711, -22.79471317813428044 ) ) ;
#2318 = CARTESIAN_POINT ( 'NONE',  ( -56.48582580120559271, -6.472252184284187138, -6.472252184284199572 ) ) ;
#2319 = CARTESIAN_POINT ( 'NONE',  ( 132.4338126186516149, -12.33615677966369972, 29.78211700502403048 ) ) ;
#2320 = ORIENTED_EDGE ( 'NONE', *, *, #25191, .F. ) ;
#2321 = ORIENTED_EDGE ( 'NONE', *, *, #26327, .F. ) ;
#2322 = VERTEX_POINT ( 'NONE', #4715 ) ;
#2323 = CARTESIAN_POINT ( 'NONE',  ( 199.9999999999999432, -20.00000000000006750, 0.000000000000000000 ) ) ;
#2324 = CARTESIAN_POINT ( 'NONE',  ( -88.39148973765149719, -8.027153355909691257, -20.15708830332379975 ) ) ;
#2325 = CARTESIAN_POINT ( 'NONE',  ( -91.56559293963834989, 12.25131212657497848, -12.25131212657469426 ) ) ;
#2326 = LINE ( 'NONE', #18553, #4936 ) ;
#2327 = EDGE_CURVE ( 'NONE', #7090, #61, #14669, .T. ) ;
#2328 = CARTESIAN_POINT ( 'NONE',  ( -199.9999999999999147, -49.28189405767606956, -14.17215463606684089 ) ) ;
#2329 = PRODUCT_DEFINITION_SHAPE ( 'NONE', 'NONE',  #26363 ) ;
#2330 = CARTESIAN_POINT ( 'NONE',  ( -126.6834154283331912, 11.16464792285796293, 24.04426794716179572 ) ) ;
#2331 = CARTESIAN_POINT ( 'NONE',  ( 200.0000000000000000, 2.939587388390868306, -18.77290383772223592 ) ) ;
#2332 = CARTESIAN_POINT ( 'NONE',  ( 199.9999999999999716, -2.174716591481574035, -18.87967999152925103 ) ) ;
#2333 = CARTESIAN_POINT ( 'NONE',  ( -213.1075012329537230, 9.698598906450543566, -9.698598906450348167 ) ) ;
#2334 = CARTESIAN_POINT ( 'NONE',  ( 14.38125909742181818, -39.01709431150928253, 17.55144818341435808 ) ) ;
#2335 = CARTESIAN_POINT ( 'NONE',  ( -110.0946026131977789, 20.04280215252648034, 2.777995947984109648 ) ) ;
#2336 = CARTESIAN_POINT ( 'NONE',  ( -56.48582580120560692, 39.99999999999991473, 9.153146818114004546 ) ) ;
#2337 = CARTESIAN_POINT ( 'NONE',  ( 14.38125909742181818, -39.01709431150928253, 17.55144818341435808 ) ) ;
#2338 = CARTESIAN_POINT ( 'NONE',  ( 3.854699808470062550, 14.12217777258775087, 48.95177852071779512 ) ) ;
#2339 = CARTESIAN_POINT ( 'NONE',  ( 91.82158438592158234, -12.16597498397778843, 12.16597498397750954 ) ) ;
#2340 = ADVANCED_FACE ( 'NONE', ( #12819 ), #178, .F. ) ;
#2341 = EDGE_CURVE ( 'NONE', #17934, #4130, #16539, .T. ) ;
#2342 = CARTESIAN_POINT ( 'NONE',  ( -91.56559293963836410, -12.25131212657462321, -44.31723036834905827 ) ) ;
#2343 = CARTESIAN_POINT ( 'NONE',  ( 199.0193791362118532, 8.756460839110824068, 17.98522136602180055 ) ) ;
#2345 = CARTESIAN_POINT ( 'NONE',  ( 91.82158438592158234, -6.516925787240506436E-14, 22.79471317813470321 ) ) ;
#2344 = CARTESIAN_POINT ( 'NONE',  ( 4.995406935893286438, 67.35176059880245703, -10.78321810387767066 ) ) ;
#2346 = CARTESIAN_POINT ( 'NONE',  ( -100.7734535825088500, 12.25131212657428748, 44.31723036834913643 ) ) ;
#2347 = CARTESIAN_POINT ( 'NONE',  ( 23.46661716383104590, 46.77475180958804657, -13.79413593526249926 ) ) ;
#2348 = CARTESIAN_POINT ( 'NONE',  ( 57.59792236341147031, 37.56421063658187620, 2.449293598294708485E-15 ) ) ;
#2349 = CARTESIAN_POINT ( 'NONE',  ( -238.4067589809705794, 0.6820004457912757223, 0.6820004457913219076 ) ) ;
#2350 = CARTESIAN_POINT ( 'NONE',  ( 17.75917276260962296, -24.33671690504799656, -44.20478326162363913 ) ) ;
#2351 = CARTESIAN_POINT ( 'NONE',  ( -17.28139728211570869, -39.07633224435642205, 20.85871090875331646 ) ) ;
#2352 = AXIS2_PLACEMENT_3D ( 'NONE', #13008, #11378, #25253 ) ;
#2353 = CARTESIAN_POINT ( 'NONE',  ( 14.38125909742180752, 15.17850393972634038, 40.00000000000002132 ) ) ;
#2354 = ORIENTED_EDGE ( 'NONE', *, *, #14093, .T. ) ;
#2355 = CARTESIAN_POINT ( 'NONE',  ( -199.9999999999999432, 43.68705981750494516, 18.09577267661451927 ) ) ;
#2356 = CARTESIAN_POINT ( 'NONE',  ( 91.82158438592158234, -40.45024623143958564, 16.11829626348418998 ) ) ;
#2357 = CARTESIAN_POINT ( 'NONE',  ( -5.379830816902156698, -23.18791234549711788, 42.60994460517750326 ) ) ;
#2358 =( GEOMETRIC_REPRESENTATION_CONTEXT ( 3 ) GLOBAL_UNCERTAINTY_ASSIGNED_CONTEXT ( ( #5119 ) ) GLOBAL_UNIT_ASSIGNED_CONTEXT ( ( #23048, #4421, #690 ) ) REPRESENTATION_CONTEXT ( 'NONE', 'WORKASPACE' ) );
#2359 = CARTESIAN_POINT ( 'NONE',  ( 9.345847406388463341, 24.85453859512489316, -44.90706793518255324 ) ) ;
#2360 = CARTESIAN_POINT ( 'NONE',  ( 199.0130599948309680, -9.716555752287060699, -17.48250520384952367 ) ) ;
#2361 = CARTESIAN_POINT ( 'NONE',  ( 184.8905102610680444, -1.851754852062639767E-13, 20.92133201514444352 ) ) ;
#2362 = CARTESIAN_POINT ( 'NONE',  ( 200.0000000000000000, 75.00000000000000000, 0.000000000000000000 ) ) ;
#2363 = CARTESIAN_POINT ( 'NONE',  ( -197.4153392276943748, -24.72549520223458330, 44.73189834455659764 ) ) ;
#2364 = CARTESIAN_POINT ( 'NONE',  ( 151.7948205124836534, -23.49921654115981084, -33.06932595376387951 ) ) ;
#2365 = CARTESIAN_POINT ( 'NONE',  ( -105.2940237833716282, 11.46076537571703646, -18.12284447397524190 ) ) ;
#2366 = VECTOR ( 'NONE', #194, 1000.000000000000227 ) ;
#2367 = VECTOR ( 'NONE', #4874, 1000.000000000000114 ) ;
#2369 = CARTESIAN_POINT ( 'NONE',  ( -91.56559293963834989, -16.03295912088728414, 16.03295912088688269 ) ) ;
#2368 = CARTESIAN_POINT ( 'NONE',  ( -189.0540493709910095, 17.95404051684933577, -43.34488811517292106 ) ) ;
#2370 = CARTESIAN_POINT ( 'NONE',  ( 184.8905102610680444, -14.79361573936399665, 14.79361573936367158 ) ) ;
#2371 = CARTESIAN_POINT ( 'NONE',  ( -86.96347745069644475, -18.24025645688354302, -2.449293598294708485E-15 ) ) ;
#2372 = CARTESIAN_POINT ( 'NONE',  ( -238.4067589809705794, 40.96449427998256709, 2.449293598294708485E-15 ) ) ;
#2373 = CARTESIAN_POINT ( 'NONE',  ( -162.0762913951020892, -1.202636532414034422E-14, -1.694272876828323948 ) ) ;
#2374 = CARTESIAN_POINT ( 'NONE',  ( 151.7948205124836534, -23.49921654116027980, 33.06932595376354556 ) ) ;
#2375 = CARTESIAN_POINT ( 'NONE',  ( -188.2995950289364941, -13.82811170417257607, 46.99046209955427855 ) ) ;
#2376 = CARTESIAN_POINT ( 'NONE',  ( -30.26275506840323359, -1.198031551615522439, -57.76657404653986561 ) ) ;
#2377 = CARTESIAN_POINT ( 'NONE',  ( 130.8568914410475088, 52.36146031193420924, 4.207082182989907437 ) ) ;
#2378 = ORIENTED_EDGE ( 'NONE', *, *, #17423, .F. ) ;
#2379 = VECTOR ( 'NONE', #1409, 1000.000000000000000 ) ;
#2380 = CARTESIAN_POINT ( 'NONE',  ( 19.06497207195980792, 10.03556273973433299, 10.03556273973436319 ) ) ;
#2381 = CARTESIAN_POINT ( 'NONE',  ( -196.0240701155051113, -14.12332411291384737, -48.96019554246502281 ) ) ;
#2382 = CARTESIAN_POINT ( 'NONE',  ( 146.6084372240433709, 24.48358557860311180, 32.08495691632071356 ) ) ;
#2383 = CARTESIAN_POINT ( 'NONE',  ( -3.921555385251674686, -43.03974577853533390, -23.47492146735003615 ) ) ;
#2384 = VERTEX_POINT ( 'NONE', #18806 ) ;
#2385 = DIRECTION ( 'NONE',  ( 0.000000000000000000, 0.000000000000000000, -1.000000000000000000 ) ) ;
#2386 = CARTESIAN_POINT ( 'NONE',  ( -82.26522686998488609, -10.29055646685526426, -17.41035301669956681 ) ) ;
#2387 = VERTEX_POINT ( 'NONE', #24941 ) ;
#2388 = CARTESIAN_POINT ( 'NONE',  ( 199.9999999999996021, 4.009690090792337180, -18.57554820616829261 ) ) ;
#2389 = CIRCLE ( 'NONE', #20666, 6.000000000000019540 ) ;
#2390 = DIRECTION ( 'NONE',  ( 0.000000000000000000, 0.000000000000000000, 1.000000000000000000 ) ) ;
#2391 = CARTESIAN_POINT ( 'NONE',  ( -190.0144721488881601, -47.57279682963539358, -13.91469502168864203 ) ) ;
#2392 = CARTESIAN_POINT ( 'NONE',  ( 4.995406935893298872, -1.944352046434030652E-13, 55.24977328854835434 ) ) ;
#2393 = CARTESIAN_POINT ( 'NONE',  ( -56.48582580120559982, 30.84685318188643777, -40.00000000000002132 ) ) ;
#2394 = CARTESIAN_POINT ( 'NONE',  ( 184.8905102610680444, -43.07788698682556827, -13.49065550809859104 ) ) ;
#2395 = CARTESIAN_POINT ( 'NONE',  ( 199.0262120803540995, -11.39568569719682145, 16.44280778893389439 ) ) ;
#2396 = CIRCLE ( 'NONE', #1538, 15.00000000000000178 ) ;
#2397 = CARTESIAN_POINT ( 'NONE',  ( 14.38125909742182529, -40.00000000000021316, 55.17850393974251944 ) ) ;
#2398 = CARTESIAN_POINT ( 'NONE',  ( 184.8905102610680444, 40.00000000000013500, -20.92133201514430141 ) ) ;
#2399 = CARTESIAN_POINT ( 'NONE',  ( -190.1760961843334030, -23.85870989132040521, -43.55713529792407002 ) ) ;
#2400 = CYLINDRICAL_SURFACE ( 'NONE', #15990, 29.99999999999999289 ) ;
#2401 = CARTESIAN_POINT ( 'NONE',  ( 199.9999999999999432, -19.99999999999988987, -2.449293598294708485E-15 ) ) ;
#2402 = CARTESIAN_POINT ( 'NONE',  ( -198.0356074513804572, 17.40982414986446969, 39.15871834505921356 ) ) ;
#2403 = CARTESIAN_POINT ( 'NONE',  ( -213.1075012329537230, 1.045191102001431893E-13, -13.71589010951911902 ) ) ;
#2404 = EDGE_CURVE ( 'NONE', #1338, #2553, #2054, .T. ) ;
#2405 = CARTESIAN_POINT ( 'NONE',  ( -716.9846540392142060, -52.49999999999992895, -52.49999999999999289 ) ) ;
#2406 = CARTESIAN_POINT ( 'NONE',  ( -238.4067589809705794, 40.00000000000040501, -40.96449427990138759 ) ) ;
#2407 = CARTESIAN_POINT ( 'NONE',  ( -213.1075012329537230, 39.99999999999979394, 53.71589010950180665 ) ) ;
#2408 = CARTESIAN_POINT ( 'NONE',  ( 199.0261461916015264, -10.84957391917088110, 16.80813345823991867 ) ) ;
#2409 = VECTOR ( 'NONE', #2139, 1000.000000000000000 ) ;
#2410 = FACE_OUTER_BOUND ( 'NONE', #20252, .T. ) ;
#2411 = CARTESIAN_POINT ( 'NONE',  ( -114.4364955367335881, -20.04994829326802019, 8.644468109231409514 ) ) ;
#2412 = CARTESIAN_POINT ( 'NONE',  ( 151.7948205124835681, -4.785054706298153882, -51.78348778862540058 ) ) ;
#2413 = ORIENTED_EDGE ( 'NONE', *, *, #2459, .T. ) ;
#2414 = CARTESIAN_POINT ( 'NONE',  ( -24.88648382767190270, 36.77569126515872711, -19.35593139203984592 ) ) ;
#2415 = CARTESIAN_POINT ( 'NONE',  ( -190.0000000000000000, 52.50000000000007816, -52.49999999999999289 ) ) ;
#2416 = CARTESIAN_POINT ( 'NONE',  ( 4.995406935893307754, -55.24977328853207581, -40.00000000000002132 ) ) ;
#2417 = CARTESIAN_POINT ( 'NONE',  ( -114.7823189589621649, 14.64951506468985798, -16.64646944818631980 ) ) ;
#2418 = CARTESIAN_POINT ( 'NONE',  ( 19.06497207195980792, 10.03556273973447155, -10.03556273973422286 ) ) ;
#2419 = VERTEX_POINT ( 'NONE', #14277 ) ;
#2420 =( BOUNDED_CURVE ( )  B_SPLINE_CURVE ( 3, ( #25615, #21605, #1259, #9760 ),
 .UNSPECIFIED., .F., .F. ) 
 B_SPLINE_CURVE_WITH_KNOTS ( ( 4, 4 ),
 ( 0.004183487405659177746, 0.01388163287021749320 ),
 .UNSPECIFIED. ) 
 CURVE ( )  GEOMETRIC_REPRESENTATION_ITEM ( )  RATIONAL_B_SPLINE_CURVE ( ( 0.6809743333591599113, 0.7608653435686186794, 0.8672072324488987460, 1.000000000000000000 ) ) 
 REPRESENTATION_ITEM ( '' )  );
#2421 = ORIENTED_EDGE ( 'NONE', *, *, #965, .T. ) ;
#2422 = CARTESIAN_POINT ( 'NONE',  ( 199.9999999999999716, -6.125576256895536531, 18.00661530747469996 ) ) ;
#2423 = CARTESIAN_POINT ( 'NONE',  ( -99.31364972216337605, 8.164808577109676335, -20.79869444142046575 ) ) ;
#2424 = CARTESIAN_POINT ( 'NONE',  ( 23.35901252181146859, 23.34306388117459008, 42.86175755505350793 ) ) ;
#2425 = VERTEX_POINT ( 'NONE', #453 ) ;
#2426 = ORIENTED_EDGE ( 'NONE', *, *, #1020, .T. ) ;
#2427 = CARTESIAN_POINT ( 'NONE',  ( 4.995406935893294431, -17.50105314357198694, 39.06748935135188816 ) ) ;
#2428 = CARTESIAN_POINT ( 'NONE',  ( 199.0198127172867828, -18.35326955327933618, -7.958687714023728432 ) ) ;
#2429 = CARTESIAN_POINT ( 'NONE',  ( -110.0822598093780300, -4.084357705409311201, 19.77208535310552051 ) ) ;
#2430 = CARTESIAN_POINT ( 'NONE',  ( -30.26275506840325136, 57.76657404653985139, 1.198031551616126178 ) ) ;
#2431 = CARTESIAN_POINT ( 'NONE',  ( -105.2054292635175727, 7.329160573984922335E-13, -21.49321519473985020 ) ) ;
#2432 = DIRECTION ( 'NONE',  ( 0.000000000000000000, 1.000000000000000000, 0.000000000000000000 ) ) ;
#2433 = CARTESIAN_POINT ( 'NONE',  ( -198.0356074513804572, 5.461327841961909642E-13, -55.37879056873073580 ) ) ;
#2434 = CARTESIAN_POINT ( 'NONE',  ( 200.0000000000000000, 39.99999999999985079, 20.00000000000052225 ) ) ;
#2435 = CARTESIAN_POINT ( 'NONE',  ( -163.5815475687401204, 38.33196416463010081, -12.03526863292965388 ) ) ;
#2436 = CARTESIAN_POINT ( 'NONE',  ( -265.0000000000000000, -4.867971026610730343E-14, -6.532754371361504014E-30 ) ) ;
#2437 = CARTESIAN_POINT ( 'NONE',  ( 199.0066757862822726, 19.23093628729661475, -5.478378800400602877 ) ) ;
#2438 = CARTESIAN_POINT ( 'NONE',  ( -188.3392535381826178, 23.45796413245995282, 43.01687576774276778 ) ) ;
#2439 = CARTESIAN_POINT ( 'NONE',  ( -100.7734535825088500, 16.03295912088691821, 16.03295912088721309 ) ) ;
#2440 = CARTESIAN_POINT ( 'NONE',  ( 98.29820294267865677, 17.41560179325850655, -10.21753654889061202 ) ) ;
#2441 = CARTESIAN_POINT ( 'NONE',  ( -192.9588430854690273, 18.05360324515418924, 38.51493924976949756 ) ) ;
#2442 = DIRECTION ( 'NONE',  ( -1.000000000000000000, -1.836970198721030427E-16, 0.000000000000000000 ) ) ;
#2443 = CARTESIAN_POINT ( 'NONE',  ( 130.8568914410475088, 24.07718906446937623, -32.49135343045455215 ) ) ;
#2444 = CARTESIAN_POINT ( 'NONE',  ( -200.0000000000000000, 45.81998439131063350, -19.51623549979301586 ) ) ;
#2445 = CARTESIAN_POINT ( 'NONE',  ( 130.8568914410475372, 34.05028731879791337, 0.000000000000000000 ) ) ;
#2446 = B_SPLINE_CURVE_WITH_KNOTS ( 'NONE', 3,
 ( #22171, #12847, #14965, #2607, #25356, #1137, #12704, #18829, #3127, #17348, #6977, #21229 ),
 .UNSPECIFIED., .F., .F.,
 ( 4, 2, 2, 2, 2, 4 ),
 ( 0.004260855364862041646, 0.008951250736248025225, 0.01129644842194101745, 0.01364164610763400967, 0.01833204147901999065, 0.02302243685040597510 ),
 .UNSPECIFIED. ) ;
#2447 = CARTESIAN_POINT ( 'NONE',  ( 136.1360204305621551, 3.511608612530062512, 53.05693388239318864 ) ) ;
#2448 = CARTESIAN_POINT ( 'NONE',  ( -91.56559293963836410, 22.67402823373189946, -0.000000000000000000 ) ) ;
#2449 = CARTESIAN_POINT ( 'NONE',  ( -592.4863246237233625, 44.61088836317698281, 5.935200987246425974 ) ) ;
#2450 = APPLICATION_CONTEXT ( 'automotive_design' ) ;
#2451 = CARTESIAN_POINT ( 'NONE',  ( -100.7734535825088358, 1.654174317907124744E-13, -17.32597176626811120 ) ) ;
#2452 = CARTESIAN_POINT ( 'NONE',  ( 199.0118788846117468, -7.586312082139164303, -18.50318004405354699 ) ) ;
#2453 = DIRECTION ( 'NONE',  ( 0.000000000000000000, -1.000000000000000000, 0.000000000000000000 ) ) ;
#2454 = ORIENTED_EDGE ( 'NONE', *, *, #3381, .F. ) ;
#2455 = VERTEX_POINT ( 'NONE', #6167 ) ;
#2456 = CARTESIAN_POINT ( 'NONE',  ( 0.2972598230769930572, 14.33493731733933352, 0.000000000000000000 ) ) ;
#2457 = SURFACE_STYLE_USAGE ( .BOTH. , #331 ) ;
#2458 = CARTESIAN_POINT ( 'NONE',  ( 14.38125909742181108, 39.01709431150961649, -39.01709431150867147 ) ) ;
#2459 = EDGE_CURVE ( 'NONE', #13654, #22653, #3464, .T. ) ;
#2460 = CARTESIAN_POINT ( 'NONE',  ( 98.29820294267332770, 18.47759065023125302, -7.653668647303920380 ) ) ;
#2461 = CARTESIAN_POINT ( 'NONE',  ( -188.2995950289364089, -43.00522595870943832, -23.44932284466036521 ) ) ;
#2462 =( BOUNDED_SURFACE ( )  B_SPLINE_SURFACE ( 3, 2, ( 
 ( #21358, #8851, #14699 ),
 ( #3002, #8988, #10720 ),
 ( #16833, #15091, #4871 ),
 ( #11230, #15222, #5003 ),
 ( #16961, #12975, #21098 ),
 ( #17092, #24967, #23353 ) ),
 .UNSPECIFIED., .F., .F., .F. ) 
 B_SPLINE_SURFACE_WITH_KNOTS ( ( 4, 2, 4 ),
 ( 3, 3 ),
 ( 0.04143195986178510593, 0.04845790097403032681, 0.05548384208627555464 ),
 ( 0.000000000000000000, 1.000000000000000000 ),
 .UNSPECIFIED. ) 
 GEOMETRIC_REPRESENTATION_ITEM ( )  RATIONAL_B_SPLINE_SURFACE ( (
 ( 1.000000000000000000, 0.9541700777564472435, 1.000000000000000000),
 ( 1.000000000000000000, 0.9520117016571142399, 1.000000000000000000),
 ( 1.000000000000000000, 0.9503157806795483609, 1.000000000000000000),
 ( 1.000000000000000000, 0.9480088156006571953, 1.000000000000000000),
 ( 1.000000000000000000, 0.9474362554090329791, 1.000000000000000000),
 ( 1.000000000000000000, 0.9474350312570024579, 1.000000000000000000) ) ) 
 REPRESENTATION_ITEM ( '' )  SURFACE ( )  );
#2463 = CARTESIAN_POINT ( 'NONE',  ( -83.28983882461058386, -1.484402994022060711E-13, 35.99236576815652455 ) ) ;
#2464 = CARTESIAN_POINT ( 'NONE',  ( 200.0000000000001137, 15.89309473284322749, -10.41337480477382371 ) ) ;
#2465 = CARTESIAN_POINT ( 'NONE',  ( 170.0000000000000000, -2.301191124287261779E-13, 24.95097643317000546 ) ) ;
#2466 = CARTESIAN_POINT ( 'NONE',  ( -100.7734535825088500, -16.03295912088659492, -40.53558337403696044 ) ) ;
#2467 = CARTESIAN_POINT ( 'NONE',  ( 163.1118516004056573, -9.006482792074626431, 47.56205970284951690 ) ) ;
#2468 = CARTESIAN_POINT ( 'NONE',  ( -190.0000000000000000, 71.50000000000009948, 66.50000000000005684 ) ) ;
#2469 = CARTESIAN_POINT ( 'NONE',  ( 136.1360204305621551, 40.00000000000009948, -4.966164525586641787 ) ) ;
#2470 = CARTESIAN_POINT ( 'NONE',  ( -351.0000000000000568, -4.857225732735059864E-14, 20.53474504356812247 ) ) ;
#2471 = CARTESIAN_POINT ( 'NONE',  ( -3.071327051952974063, 13.87830843099595057, 47.32824404903805515 ) ) ;
#2472 = CARTESIAN_POINT ( 'NONE',  ( -86.96347745069644475, -15.38646221621786125, -15.38646221621789856 ) ) ;
#2473 = CARTESIAN_POINT ( 'NONE',  ( 146.6084372240433709, -3.800685668858344801, -52.76785682606520567 ) ) ;
#2474 = CARTESIAN_POINT ( 'NONE',  ( 199.0112297511867325, 18.97400286213774834, 6.326091761587574247 ) ) ;
#2476 = CARTESIAN_POINT ( 'NONE',  ( -56.48582580120559982, 39.99999999999990763, 30.84685318188658698 ) ) ;
#2475 = CARTESIAN_POINT ( 'NONE',  ( 163.1118516004056573, -47.56205970284945295, -9.006482792074823607 ) ) ;
#2477 = CARTESIAN_POINT ( 'NONE',  ( 0.2972598230769907257, 66.70487387989869887, -10.13633138497392494 ) ) ;
#2478 = CARTESIAN_POINT ( 'NONE',  ( 23.26364522860148654, 42.89098160628032730, -23.36474233297085945 ) ) ;
#2479 = CARTESIAN_POINT ( 'NONE',  ( 136.1360204305621266, 4.966164525587089429, 2.449293598294708485E-15 ) ) ;
#2480 = CARTESIAN_POINT ( 'NONE',  ( -135.8532207217289738, -34.75652343174615311, 21.81201906317767936 ) ) ;
#2481 = CARTESIAN_POINT ( 'NONE',  ( -105.3755690713226585, 18.24025645688349684, 40.00000000000002132 ) ) ;
#2482 = ADVANCED_FACE ( 'NONE', ( #24803 ), #2580, .F. ) ;
#2483 = CARTESIAN_POINT ( 'NONE',  ( -4.201409602816726263, -42.95750343186489317, 23.41774994521231790 ) ) ;
#2484 = CARTESIAN_POINT ( 'NONE',  ( 163.1118516004056573, 12.73709011382477918, 40.00000000000002132 ) ) ;
#2485 = EDGE_CURVE ( 'NONE', #7299, #6050, #16556, .T. ) ;
#2486 = EDGE_LOOP ( 'NONE', ( #15483, #4393, #761, #12919 ) ) ;
#2487 = DIRECTION ( 'NONE',  ( 0.000000000000000000, 1.000000000000000000, 0.000000000000000000 ) ) ;
#2488 = CARTESIAN_POINT ( 'NONE',  ( -280.0000000000000000, -14.14213562373098831, -14.14213562373098654 ) ) ;
#2489 = CARTESIAN_POINT ( 'NONE',  ( 200.0000000000000000, -66.50000000000001421, 66.50000000000005684 ) ) ;
#2490 = ADVANCED_FACE ( 'NONE', ( #980 ), #8909, .T. ) ;
#2491 = ADVANCED_FACE ( 'NONE', ( #19068 ), #11608, .T. ) ;
#2492 = CARTESIAN_POINT ( 'NONE',  ( -4.421177063218397763, 13.80119274858276590, -46.85829989839402288 ) ) ;
#2493 = CARTESIAN_POINT ( 'NONE',  ( 199.9999999999997158, -10.44119114510941770, 15.88703355754643098 ) ) ;
#2494 = CARTESIAN_POINT ( 'NONE',  ( -100.7734535825088500, 12.25131212657428748, 44.31723036834913643 ) ) ;
#2495 = DIRECTION ( 'NONE',  ( -1.000000000000000000, 1.836970198721030181E-16, 0.000000000000000000 ) ) ;
#2496 = PRESENTATION_STYLE_ASSIGNMENT (( #11008 ) ) ;
#2498 = CARTESIAN_POINT ( 'NONE',  ( -189.1288815661663989, -23.62384257861548775, 43.24061771116531361 ) ) ;
#2497 = AXIS2_PLACEMENT_3D ( 'NONE', #14303, #74, #16164 ) ;
#2499 = DIRECTION ( 'NONE',  ( 0.000000000000000000, 1.000000000000000000, 0.000000000000000000 ) ) ;
#2500 = CARTESIAN_POINT ( 'NONE',  ( 136.1360204305621551, -24.77266263493081766, -31.79587985999290112 ) ) ;
#2501 = CARTESIAN_POINT ( 'NONE',  ( -105.4741150117369273, 8.366608964608960974, -19.60045294982168329 ) ) ;
#2503 = CARTESIAN_POINT ( 'NONE',  ( 57.59792236341147031, 26.56190807104720975, -26.56190807104655249 ) ) ;
#2502 = DIRECTION ( 'NONE',  ( -0.3301743753965505901, 0.9439199552035636431, 0.000000000000000000 ) ) ;
#2504 = CARTESIAN_POINT ( 'NONE',  ( 19.06497207195980792, 10.03556273973447155, -10.03556273973422286 ) ) ;
#2505 = CARTESIAN_POINT ( 'NONE',  ( -91.56559293963834989, -17.32597176626812896, 40.00000000000002132 ) ) ;
#2506 = CARTESIAN_POINT ( 'NONE',  ( 163.1118516004056573, 12.73709011382478273, 2.449293598294708485E-15 ) ) ;
#2507 = CARTESIAN_POINT ( 'NONE',  ( -100.7734535825088358, -2.560096224687585342E-13, 22.67402823373191723 ) ) ;
#2508 = CARTESIAN_POINT ( 'NONE',  ( 136.1360204305621551, 31.79587985999267374, -24.77266263493117293 ) ) ;
#2509 = CARTESIAN_POINT ( 'NONE',  ( -86.86578273022546171, 19.68494377654086591, -8.153770686795049016 ) ) ;
#2510 = CARTESIAN_POINT ( 'NONE',  ( -100.7734535825088500, 16.03295912088740494, -40.53558337403661938 ) ) ;
#2511 = CARTESIAN_POINT ( 'NONE',  ( -198.0356074513804572, -10.87444709759729911, 10.87444709759714812 ) ) ;
#2512 = ORIENTED_EDGE ( 'NONE', *, *, #10872, .F. ) ;
#2513 = CARTESIAN_POINT ( 'NONE',  ( 199.9999999999999432, 14.14213562373090838, 14.14213562373092437 ) ) ;
#2514 = CARTESIAN_POINT ( 'NONE',  ( 190.0000000000000000, -66.50000000000001421, -66.50000000000005684 ) ) ;
#2515 = CONTEXT_DEPENDENT_SHAPE_REPRESENTATION ( #22956, #22295 ) ;
#2516 = CARTESIAN_POINT ( 'NONE',  ( 146.6084372240433993, -3.800685668858652999, 3.800685668858636568 ) ) ;
#2517 = CARTESIAN_POINT ( 'NONE',  ( 16.38602454699831057, -48.74566733939990826, -14.09104119327536786 ) ) ;
#2518 = ORIENTED_EDGE ( 'NONE', *, *, #3123, .F. ) ;
#2519 = CARTESIAN_POINT ( 'NONE',  ( 19.06497207195980792, 14.19242893257840876, 0.000000000000000000 ) ) ;
#2520 = DIRECTION ( 'NONE',  ( 0.000000000000000000, 1.000000000000000000, 0.000000000000000000 ) ) ;
#2521 = CIRCLE ( 'NONE', #5914, 30.00000000000003908 ) ;
#2522 = ORIENTED_EDGE ( 'NONE', *, *, #3703, .F. ) ;
#2523 = CARTESIAN_POINT ( 'NONE',  ( 199.9999999999998863, 12.52392839731578889, -14.30162278802013098 ) ) ;
#2524 = DIRECTION ( 'NONE',  ( 0.000000000000000000, -0.6739498806388345420, -0.7387770694782699321 ) ) ;
#2525 = CARTESIAN_POINT ( 'NONE',  ( -192.9588430854689989, 54.46834944099968823, 2.449293598294708485E-15 ) ) ;
#2526 = CARTESIAN_POINT ( 'NONE',  ( 130.8568914410475372, -24.07718906447255947, 24.07718906447199458 ) ) ;
#2527 = CARTESIAN_POINT ( 'NONE',  ( 199.0117592729713465, 18.59672480091233737, 7.361113620700817428 ) ) ;
#2528 = CARTESIAN_POINT ( 'NONE',  ( -198.0356074513804572, -67.44298959253333692, -10.87444709761016348 ) ) ;
#2529 = CARTESIAN_POINT ( 'NONE',  ( -192.9588430854690273, 39.99999999999980105, 54.46834944098235809 ) ) ;
#2530 = CARTESIAN_POINT ( 'NONE',  ( -213.1075012329537230, 39.99999999999979394, 53.71589010950180665 ) ) ;
#2531 = CARTESIAN_POINT ( 'NONE',  ( 199.9999999999999432, 1.065690307512836407E-13, -20.00000000000010303 ) ) ;
#2532 = CARTESIAN_POINT ( 'NONE',  ( -280.0000000000000000, 19.99999999999996092, -0.000000000000000000 ) ) ;
#2533 = CARTESIAN_POINT ( 'NONE',  ( -598.0968614159205572, 39.17219949141968272, 8.155532079469960394 ) ) ;
#2534 = CARTESIAN_POINT ( 'NONE',  ( -30.26275506840323004, -41.69427246844627888, -40.00000000000002132 ) ) ;
#2535 = CARTESIAN_POINT ( 'NONE',  ( -162.0762913951020607, -1.198031840455708430, 57.76657433537920383 ) ) ;
#2536 = CARTESIAN_POINT ( 'NONE',  ( 110.0479209278586552, -9.419601331808673095, -22.74092928740049402 ) ) ;
#2537 = CARTESIAN_POINT ( 'NONE',  ( -105.2333497862813374, 16.99530394074077222, -13.14348404881843280 ) ) ;
#2538 = CARTESIAN_POINT ( 'NONE',  ( 19.06497207195980792, 40.00000000000059686, -54.19242893257802507 ) ) ;
#2539 = CARTESIAN_POINT ( 'NONE',  ( -259.2033419157646676, 39.99999999999987210, 30.48217210827754542 ) ) ;
#2540 = CARTESIAN_POINT ( 'NONE',  ( 184.8905102610680444, 13.49065550809817715, -43.07788698682574591 ) ) ;
#2541 = DIRECTION ( 'NONE',  ( 0.000000000000000000, -1.000000000000000000, 0.000000000000000000 ) ) ;
#2542 = CARTESIAN_POINT ( 'NONE',  ( 190.0000000000000284, -125.7889608577475400, 2.115966675574909200E-14 ) ) ;
#2543 = CARTESIAN_POINT ( 'NONE',  ( -198.0356074513804572, -67.44298959250878056, 10.87444709758448447 ) ) ;
#2544 = ORIENTED_EDGE ( 'NONE', *, *, #15330, .F. ) ;
#2545 = LINE ( 'NONE', #8794, #12997 ) ;
#2546 = DIRECTION ( 'NONE',  ( 0.000000000000000000, 0.000000000000000000, 1.000000000000000000 ) ) ;
#2547 = CARTESIAN_POINT ( 'NONE',  ( 163.1118516004056573, 27.26290988616876021, -40.00000000000002132 ) ) ;
#2548 = AXIS2_PLACEMENT_3D ( 'NONE', #23606, #16375, #12123 ) ;
#2549 = CARTESIAN_POINT ( 'NONE',  ( -105.2940152837819454, 11.46092073792507193, 18.12276621495183804 ) ) ;
#2550 = CYLINDRICAL_SURFACE ( 'NONE', #10885, 5.000000000000004441 ) ;
#2551 = SHAPE_REPRESENTATION_RELATIONSHIP ( 'NONE' , 'NONE' ,  #3691, #22606 ) ;
#2552 = ORIENTED_EDGE ( 'NONE', *, *, #25597, .F. ) ;
#2553 = VERTEX_POINT ( 'NONE', #8910 ) ;
#2554 = CARTESIAN_POINT ( 'NONE',  ( 199.9999999999999716, -10.82917866272351581, 15.62749623992054637 ) ) ;
#2555 = CARTESIAN_POINT ( 'NONE',  ( 126.3230993689413708, 11.72464299830509482, -28.30579214049042847 ) ) ;
#2556 = CARTESIAN_POINT ( 'NONE',  ( 6.762329110783161568, 18.56720258519183986, 44.82519229650664983 ) ) ;
#2557 = ORIENTED_EDGE ( 'NONE', *, *, #2240, .T. ) ;
#2558 = ORIENTED_EDGE ( 'NONE', *, *, #9614, .T. ) ;
#2559 = PRODUCT_DEFINITION_SHAPE ( 'NONE', 'NONE',  #14914 ) ;
#2560 = CARTESIAN_POINT ( 'NONE',  ( -135.8532207217289738, -34.75652343174615311, 21.81201906317767936 ) ) ;
#2561 = CARTESIAN_POINT ( 'NONE',  ( 199.0234688043258018, -20.00162938710794691, 0.3307560783973806373 ) ) ;
#2562 = CARTESIAN_POINT ( 'NONE',  ( 190.0000000000000284, -82.49999999999990052, 52.49999999999977973 ) ) ;
#2563 = CARTESIAN_POINT ( 'NONE',  ( -213.1075012329537230, -18.58567234101155208, 37.98287015391234434 ) ) ;
#2564 = FACE_OUTER_BOUND ( 'NONE', #16654, .T. ) ;
#2565 = CARTESIAN_POINT ( 'NONE',  ( -86.96347745069645896, 40.00000000000008527, -21.75974354311636461 ) ) ;
#2566 = CIRCLE ( 'NONE', #26311, 69.99999999999994316 ) ;
#2567 = EDGE_CURVE ( 'NONE', #9742, #21974, #6511, .T. ) ;
#2568 = DIRECTION ( 'NONE',  ( 0.000000000000000000, 1.000000000000000000, 0.000000000000000000 ) ) ;
#2569 = CARTESIAN_POINT ( 'NONE',  ( -362.0709805440841365, -4.857225732735059864E-14, 0.000000000000000000 ) ) ;
#2570 = CONICAL_SURFACE ( 'NONE', #19542, 60.00000000000009948, 0.7853981633974479459 ) ;
#2571 = CARTESIAN_POINT ( 'NONE',  ( -100.7734535825088500, 40.00000000000017764, -17.32597176626768487 ) ) ;
#2572 = CARTESIAN_POINT ( 'NONE',  ( -30.26275506840324070, 1.218738420030236455E-14, -1.694272468446259783 ) ) ;
#2573 = CARTESIAN_POINT ( 'NONE',  ( -653.5054087259286462, 37.46094337825315534, 14.03175942970671386 ) ) ;
#2574 = CARTESIAN_POINT ( 'NONE',  ( -87.13361725327074225, -15.19799821270821560, -15.19799821270861884 ) ) ;
#2575 = CARTESIAN_POINT ( 'NONE',  ( 199.0055623607443636, 10.83365079593514757, -16.80863377785637169 ) ) ;
#2576 = CARTESIAN_POINT ( 'NONE',  ( -188.6013476421465782, 13.84412643133159904, 47.09841799633510817 ) ) ;
#2577 = CARTESIAN_POINT ( 'NONE',  ( 91.82158438592156813, -16.11829626348459144, 40.45024623143943643 ) ) ;
#2578 = DIRECTION ( 'NONE',  ( -1.000000000000000000, -1.836970198721030181E-16, -0.000000000000000000 ) ) ;
#2579 = CARTESIAN_POINT ( 'NONE',  ( 163.1118516004056573, 19.27778845539212327, 37.29075403953164169 ) ) ;
#2580 = CYLINDRICAL_SURFACE ( 'NONE', #25729, 4.999999999999962697 ) ;
#2581 = CARTESIAN_POINT ( 'NONE',  ( 146.6084372240433709, 24.48358557860356655, -32.08495691632035118 ) ) ;
#2582 = CARTESIAN_POINT ( 'NONE',  ( -653.4170159849278434, 38.71178713871361765, 22.94860588273028768 ) ) ;
#2583 = CARTESIAN_POINT ( 'NONE',  ( 184.8905102610680444, 20.92133201514447549, 0.000000000000000000 ) ) ;
#2584 = EDGE_CURVE ( 'NONE', #8799, #25674, #25753, .T. ) ;
#2585 = CARTESIAN_POINT ( 'NONE',  ( 163.1118516004056573, -19.27778845538787422, 19.27778845538743724 ) ) ;
#2586 = CARTESIAN_POINT ( 'NONE',  ( -105.3755690713226585, 21.75974354311648185, 40.00000000000002132 ) ) ;
#2587 = CARTESIAN_POINT ( 'NONE',  ( -595.8093182457012063, 42.09229316366772622, 15.94989993472014511 ) ) ;
#2588 = ORIENTED_EDGE ( 'NONE', *, *, #25417, .F. ) ;
#2589 = CARTESIAN_POINT ( 'NONE',  ( 170.2234770963711128, -39.99999999999982947, -15.44714144992858529 ) ) ;
#2590 = CARTESIAN_POINT ( 'NONE',  ( 199.0118983629657237, -7.623092896147099395, -18.48804935406682404 ) ) ;
#2591 = EDGE_CURVE ( 'NONE', #8524, #3196, #14957, .T. ) ;
#2592 = DIRECTION ( 'NONE',  ( 1.000000000000000000, 1.836970198721030427E-16, -0.000000000000000000 ) ) ;
#2593 = ORIENTED_EDGE ( 'NONE', *, *, #19566, .F. ) ;
#2594 = AXIS2_PLACEMENT_3D ( 'NONE', #23312, #23060, #22792 ) ;
#2595 = VERTEX_POINT ( 'NONE', #10778 ) ;
#2596 = CARTESIAN_POINT ( 'NONE',  ( -100.7734535825088500, 17.32597176626808988, 40.00000000000002132 ) ) ;
#2597 = DIRECTION ( 'NONE',  ( 0.000000000000000000, 0.000000000000000000, 1.000000000000000000 ) ) ;
#2598 = ADVANCED_FACE ( 'NONE', ( #23153 ), #20895, .F. ) ;
#2599 = CARTESIAN_POINT ( 'NONE',  ( 98.29820294267329928, 18.47759065023126013, -7.653668647303936368 ) ) ;
#2600 = CARTESIAN_POINT ( 'NONE',  ( -77.65678946166502783, -18.42186864997352913, 12.10857941958507134 ) ) ;
#2601 = DIRECTION ( 'NONE',  ( -1.000000000000000000, -1.836970198721030181E-16, -0.000000000000000000 ) ) ;
#2602 = CARTESIAN_POINT ( 'NONE',  ( 199.9999999999997726, 7.546454185142647653, -17.43816512261951956 ) ) ;
#2603 = CARTESIAN_POINT ( 'NONE',  ( 199.9999999999999147, 4.913383178421502073, -18.36491317384603761 ) ) ;
#2604 = VECTOR ( 'NONE', #11874, 1000.000000000000000 ) ;
#2605 = CARTESIAN_POINT ( 'NONE',  ( -280.0000000000000568, -42.42640687119276066, -14.14213562373147148 ) ) ;
#2606 = CARTESIAN_POINT ( 'NONE',  ( -280.0000000000000000, 14.14213562373078581, 14.14213562373108424 ) ) ;
#2607 = CARTESIAN_POINT ( 'NONE',  ( -100.0993625062911150, 20.55804859447406230, 8.515422543756583806 ) ) ;
#2608 = CARTESIAN_POINT ( 'NONE',  ( -238.4067589809705794, 40.00000000000040501, -40.96449427990138759 ) ) ;
#2609 = CARTESIAN_POINT ( 'NONE',  ( -575.0231298121445889, 75.00000000000000000, 24.99999999999828759 ) ) ;
#2610 = CARTESIAN_POINT ( 'NONE',  ( 21.15737826136109234, 13.91467835516651164, 47.57244852138558144 ) ) ;
#2611 = CARTESIAN_POINT ( 'NONE',  ( 199.9999999999999432, -14.14213562373096345, -14.14213562373104871 ) ) ;
#2612 = CARTESIAN_POINT ( 'NONE',  ( -213.1075012329536946, -37.98287015391263566, 37.98287015391218802 ) ) ;
#2613 = CARTESIAN_POINT ( 'NONE',  ( 199.0063941363436584, 18.94647080546362261, -6.505566240119136090 ) ) ;
#2615 = CARTESIAN_POINT ( 'NONE',  ( 170.2234770963711128, -2.511315425431857630E-14, 15.44714144992816074 ) ) ;
#2614 = CARTESIAN_POINT ( 'NONE',  ( 130.8568914410475088, -52.36146031193413108, -4.207082182990267150 ) ) ;
#2616 = CARTESIAN_POINT ( 'NONE',  ( 44.82887508605028160, 38.96139886172597500, -12.17256213098433548 ) ) ;
#2617 = CARTESIAN_POINT ( 'NONE',  ( 19.06497207195980792, 14.19242893257840876, 0.000000000000000000 ) ) ;
#2618 = CARTESIAN_POINT ( 'NONE',  ( -56.48582580120559982, -6.472252184284282173, 50.09629031063965243 ) ) ;
#2619 = CARTESIAN_POINT ( 'NONE',  ( -30.26275506840324425, 1.694272468446254232, 40.00000000000002132 ) ) ;
#2620 = ORIENTED_EDGE ( 'NONE', *, *, #697, .T. ) ;
#2621 = CARTESIAN_POINT ( 'NONE',  ( -3.406542234095978561, -43.31371932780104572, 17.94112998239678447 ) ) ;
#2622 = VECTOR ( 'NONE', #11998, 1000.000000000000000 ) ;
#2623 = CARTESIAN_POINT ( 'NONE',  ( -280.0000000000000000, 19.99999999999996092, 2.449293598294708485E-15 ) ) ;
#2624 = B_SPLINE_CURVE_WITH_KNOTS ( 'NONE', 3,
 ( #23453, #15575, #3484, #5227, #9088, #25332 ),
 .UNSPECIFIED., .F., .F.,
 ( 4, 2, 4 ),
 ( 0.3689590070116581244, 0.3867117631979620773, 0.4044645193949217288 ),
 .UNSPECIFIED. ) ;
#2625 = ORIENTED_EDGE ( 'NONE', *, *, #7357, .F. ) ;
#2626 = CARTESIAN_POINT ( 'NONE',  ( 35.93739820529123818, -20.78453043059072769, -38.99308227228176094 ) ) ;
#2627 = AXIS2_PLACEMENT_3D ( 'NONE', #12406, #2302, #18529 ) ;
#2628 =( BOUNDED_SURFACE ( )  B_SPLINE_SURFACE ( 3, 2, ( 
 ( #16950, #866, #2870 ),
 ( #25347, #8976, #10840 ),
 ( #4729, #7103, #18957 ),
 ( #738, #23343, #5122 ),
 ( #13226, #7225, #25473 ),
 ( #5240, #13729, #7869 ),
 ( #21854, #19462, #19988 ),
 ( #11868, #13593, #25605 ),
 ( #23977, #1249, #1773 ),
 ( #3763, #15461, #19854 ),
 ( #17586, #9353, #9878 ),
 ( #21594, #9482, #15716 ) ),
 .UNSPECIFIED., .F., .F., .F. ) 
 B_SPLINE_SURFACE_WITH_KNOTS ( ( 4, 2, 2, 2, 2, 4 ),
 ( 3, 3 ),
 ( 0.006022589392326875915, 0.01254516766564483035, 0.01580645680230381017, 0.01906774593896278652, 0.02559032421228074269, 0.03211290248559869887 ),
 ( 0.000000000000000000, 1.000000000000000000 ),
 .UNSPECIFIED. ) 
 GEOMETRIC_REPRESENTATION_ITEM ( )  RATIONAL_B_SPLINE_SURFACE ( (
 ( 1.000000000000000000, 0.9998834880171258988, 1.000000000000000000),
 ( 1.000000000000000000, 0.9998139205011338237, 1.000000000000000000),
 ( 1.000000000000000000, 0.9997315632445886724, 1.000000000000000000),
 ( 1.000000000000000000, 0.9996405464946352959, 1.000000000000000000),
 ( 1.000000000000000000, 0.9996155081776924023, 1.000000000000000000),
 ( 1.000000000000000000, 0.9995814087511104562, 1.000000000000000000),
 ( 1.000000000000000000, 0.9995724100939918921, 1.000000000000000000),
 ( 1.000000000000000000, 0.9995726760936894939, 1.000000000000000000),
 ( 1.000000000000000000, 0.9996103361816741639, 1.000000000000000000),
 ( 1.000000000000000000, 0.9997312749796802844, 1.000000000000000000),
 ( 1.000000000000000000, 0.9998135910914284219, 1.000000000000000000),
 ( 1.000000000000000000, 0.9998834880173383954, 1.000000000000000000) ) ) 
 REPRESENTATION_ITEM ( '' )  SURFACE ( )  );
#2629 = CARTESIAN_POINT ( 'NONE',  ( 4.995406935893294431, -17.50105314357198694, 39.06748935135188816 ) ) ;
#2630 = CARTESIAN_POINT ( 'NONE',  ( -24.53392603781537318, -12.34411287792658563, 39.81639166308519151 ) ) ;
#2631 = B_SPLINE_CURVE_WITH_KNOTS ( 'NONE', 3,
 ( #7303, #5076, #21677, #11177, #15417, #11546 ),
 .UNSPECIFIED., .F., .F.,
 ( 4, 2, 4 ),
 ( -5.999999988291011724E-08, 0.03937727647058182623, 0.07875461294116353761 ),
 .UNSPECIFIED. ) ;
#2632 = CARTESIAN_POINT ( 'NONE',  ( -3.379936260373888501, 17.94397654175175205, -43.32059152999933360 ) ) ;
#2633 = CARTESIAN_POINT ( 'NONE',  ( 199.0262772983307400, -15.97594543884460450, 12.04151787815577102 ) ) ;
#2634 = CARTESIAN_POINT ( 'NONE',  ( -135.8532207217289738, 21.81201906317729566, 34.75652343174635917 ) ) ;
#2635 = CARTESIAN_POINT ( 'NONE',  ( -77.61595200903875025, -21.80829238163389405, 3.459815247604749011 ) ) ;
#2636 = LINE ( 'NONE', #24852, #7070 ) ;
#2637 = CARTESIAN_POINT ( 'NONE',  ( -189.1816166312677581, -17.96744819724865039, 43.37725711903350856 ) ) ;
#2638 = CARTESIAN_POINT ( 'NONE',  ( 0.2972598230769976091, -10.13633138497465147, -10.13633138497482733 ) ) ;
#2639 = EDGE_CURVE ( 'NONE', #19072, #19714, #10510, .T. ) ;
#2640 = CARTESIAN_POINT ( 'NONE',  ( 151.7948205124836250, -4.785054706301671068, 4.785054706301645311 ) ) ;
#2641 = CARTESIAN_POINT ( 'NONE',  ( -198.0356074513804572, -17.40982414986427429, -39.15871834505933435 ) ) ;
#2642 = CARTESIAN_POINT ( 'NONE',  ( 184.8905102610680444, 14.79361573936375507, 14.79361573936398067 ) ) ;
#2643 = AXIS2_PLACEMENT_3D ( 'NONE', #10104, #24350, #6114 ) ;
#2645 = CARTESIAN_POINT ( 'NONE',  ( 151.7948205124836534, 33.06932595376333239, 23.49921654116065284 ) ) ;
#2644 = CARTESIAN_POINT ( 'NONE',  ( -213.1075012329537230, -9.698598906450422774, -9.698598906450550672 ) ) ;
#2646 = CARTESIAN_POINT ( 'NONE',  ( -91.56559293963834989, 12.25131212657428748, 44.31723036834913643 ) ) ;
#2647 = CARTESIAN_POINT ( 'NONE',  ( -162.0762913951020607, -41.69427287692683848, 40.00000000000002132 ) ) ;
#2648 = CARTESIAN_POINT ( 'NONE',  ( -259.2033419157646676, -9.517827891722680178, -40.00000000000002132 ) ) ;
#2649 = CARTESIAN_POINT ( 'NONE',  ( -105.3755690713226727, -2.472783935621397949E-13, 21.75974354311649961 ) ) ;
#2650 = CARTESIAN_POINT ( 'NONE',  ( -198.0356074513804572, 10.87444709759714989, 10.87444709759722450 ) ) ;
#2651 = CARTESIAN_POINT ( 'NONE',  ( -86.86493150571116928, 19.77569912839187083, -7.943527260495796050 ) ) ;
#2652 = CARTESIAN_POINT ( 'NONE',  ( 192.4448373802101173, 42.42640687122089815, -14.14213562370272470 ) ) ;
#2653 = EDGE_CURVE ( 'NONE', #9180, #21913, #21069, .T. ) ;
#2654 = CARTESIAN_POINT ( 'NONE',  ( -166.3490444793987422, 39.29840179260881428, -12.23457652165070186 ) ) ;
#2655 = ORIENTED_EDGE ( 'NONE', *, *, #24117, .T. ) ;
#2656 = CARTESIAN_POINT ( 'NONE',  ( -86.96347745069644475, -15.38646221621796073, 41.18208027870593924 ) ) ;
#2657 = CARTESIAN_POINT ( 'NONE',  ( -94.58414068589586066, 8.590713000693110502, 20.73981583682890317 ) ) ;
#2658 = CARTESIAN_POINT ( 'NONE',  ( 151.7948205124836250, -4.785054706301671068, 4.785054706301645311 ) ) ;
#2659 = CARTESIAN_POINT ( 'NONE',  ( -3.488770945845510063, -43.29206711590405376, -17.93216134257416527 ) ) ;
#2660 = ORIENTED_EDGE ( 'NONE', *, *, #58, .T. ) ;
#2661 = CARTESIAN_POINT ( 'NONE',  ( -94.58366989427186411, -20.91926462023914013, 8.190486896679004758 ) ) ;
#2662 = CARTESIAN_POINT ( 'NONE',  ( -110.0574606394870329, -9.172127818399005150, -18.01698387425555481 ) ) ;
#2663 = CARTESIAN_POINT ( 'NONE',  ( 199.9999999999999147, 7.974356211459238786, -17.24664066343551028 ) ) ;
#2664 = AXIS2_PLACEMENT_3D ( 'NONE', #2981, #19204, #3354 ) ;
#2665 = DIRECTION ( 'NONE',  ( -1.750717563385751092E-16, 0.9530462522498561739, 0.3028247695821851271 ) ) ;
#2666 = CARTESIAN_POINT ( 'NONE',  ( -30.26275506840324070, 41.69427246844628598, 2.449293598294708485E-15 ) ) ;
#2667 = DIRECTION ( 'NONE',  ( 0.000000000000000000, 0.6739498806388349861, 0.7387770694782697101 ) ) ;
#2668 = CARTESIAN_POINT ( 'NONE',  ( 199.0194208361885444, 8.684746017668368623, 18.01861981654000999 ) ) ;
#2669 = CARTESIAN_POINT ( 'NONE',  ( 170.2234770963711128, -39.20704971665404059, 17.36149277826957160 ) ) ;
#2670 = CARTESIAN_POINT ( 'NONE',  ( -280.0000000000000000, -1.237140859393462838E-13, 20.00000000000001421 ) ) ;
#2671 = CARTESIAN_POINT ( 'NONE',  ( 200.0000000000000000, 40.00000000000012790, -19.99999999999996092 ) ) ;
#2672 = EDGE_CURVE ( 'NONE', #17972, #19937, #22628, .T. ) ;
#2673 = CARTESIAN_POINT ( 'NONE',  ( -200.0000000000000284, -82.49999999999991473, -52.49999999999977973 ) ) ;
#2674 = CARTESIAN_POINT ( 'NONE',  ( -192.9588430854689705, -54.46834944099975928, -2.449293598294708485E-15 ) ) ;
#2676 = CARTESIAN_POINT ( 'NONE',  ( -619.9449226945228020, 27.37410191665372494, 29.16662018060867112 ) ) ;
#2675 = CARTESIAN_POINT ( 'NONE',  ( 23.26364522860124140, -13.80713620122686436, -46.84987168986906170 ) ) ;
#2677 = CARTESIAN_POINT ( 'NONE',  ( 136.1360204305621551, -4.966164525587036138, -40.00000000000002132 ) ) ;
#2678 = CARTESIAN_POINT ( 'NONE',  ( -213.1075012329537230, -9.698598906438496314, 66.26714140136188291 ) ) ;
#2679 = CARTESIAN_POINT ( 'NONE',  ( 130.1167162091013267, -12.15076864148440983, -29.33455044752963659 ) ) ;
#2680 = CARTESIAN_POINT ( 'NONE',  ( -110.0685463886750313, 10.00056106073172479, -17.53216629774168567 ) ) ;
#2681 = CARTESIAN_POINT ( 'NONE',  ( 170.2234770963711128, 39.99999999999980105, 24.55285855007229401 ) ) ;
#2682 = CARTESIAN_POINT ( 'NONE',  ( -30.26275506840324425, 39.99999999999987210, 41.69427246844643520 ) ) ;
#2683 = CARTESIAN_POINT ( 'NONE',  ( 199.9999999999999432, -14.14213562373096345, -14.14213562373104871 ) ) ;
#2684 = CYLINDRICAL_SURFACE ( 'NONE', #19005, 5.000000000000004441 ) ;
#2685 = DIRECTION ( 'NONE',  ( 1.000000000000000000, 1.836970198721030181E-16, -0.000000000000000000 ) ) ;
#2686 = CARTESIAN_POINT ( 'NONE',  ( 192.4448373802101173, -42.42640687116490028, -14.14213562375904942 ) ) ;
#2687 = EDGE_CURVE ( 'NONE', #18917, #17669, #16627, .T. ) ;
#2688 = ORIENTED_EDGE ( 'NONE', *, *, #11249, .T. ) ;
#2690 = CARTESIAN_POINT ( 'NONE',  ( 192.4448373802100889, -14.14213562375896061, 14.14213562375865330 ) ) ;
#2689 = CARTESIAN_POINT ( 'NONE',  ( -87.13361725327074225, 15.19799821270847850, -15.19799821270833284 ) ) ;
#2691 = CARTESIAN_POINT ( 'NONE',  ( 154.0339099654741233, 28.18615453125291381, -11.67508747798877344 ) ) ;
#2692 = CARTESIAN_POINT ( 'NONE',  ( 170.2234770963711128, 24.55285855007190676, -40.00000000000002132 ) ) ;
#2693 = CARTESIAN_POINT ( 'NONE',  ( -87.13361725327072804, 5.903697393916396424E-14, -21.49321519333428299 ) ) ;
#2694 = FACE_BOUND ( 'NONE', #25987, .T. ) ;
#2695 =( NAMED_UNIT ( * ) SI_UNIT ( $, .STERADIAN. ) SOLID_ANGLE_UNIT ( ) );
#2696 = ORIENTED_EDGE ( 'NONE', *, *, #3076, .F. ) ;
#2697 = VERTEX_POINT ( 'NONE', #10914 ) ;
#2698 = CARTESIAN_POINT ( 'NONE',  ( 199.9999999999999432, 5.207736135262080346, 18.28309964035191726 ) ) ;
#2699 = DIRECTION ( 'NONE',  ( 0.000000000000000000, 1.000000000000000000, 0.000000000000000000 ) ) ;
#2700 = CARTESIAN_POINT ( 'NONE',  ( 19.44355705751405239, 18.20455056366773405, 43.94967286773182025 ) ) ;
#2701 = ORIENTED_EDGE ( 'NONE', *, *, #10106, .F. ) ;
#2702 = ORIENTED_EDGE ( 'NONE', *, *, #4106, .F. ) ;
#2703 = CARTESIAN_POINT ( 'NONE',  ( -213.1075012329537230, -18.58567234101155208, 37.98287015391234434 ) ) ;
#2704 = CARTESIAN_POINT ( 'NONE',  ( 199.0181825105790665, -16.81808889125263207, -10.83063377519274795 ) ) ;
#2705 = CARTESIAN_POINT ( 'NONE',  ( -105.4293522941591590, -7.324187428699950431, 20.05597878319033356 ) ) ;
#2706 = CARTESIAN_POINT ( 'NONE',  ( -135.8532207217289738, -6.472252184284287502, 50.09629031063965243 ) ) ;
#2707 = CARTESIAN_POINT ( 'NONE',  ( 199.9999999999999432, -14.14213562373096345, -14.14213562373104871 ) ) ;
#2708 = CARTESIAN_POINT ( 'NONE',  ( -238.4067589809705794, 39.99999999999983658, 40.96449428006354765 ) ) ;
#2709 = DIRECTION ( 'NONE',  ( 1.000000000000000000, 0.000000000000000000, 0.000000000000000000 ) ) ;
#2710 = CARTESIAN_POINT ( 'NONE',  ( -86.86493150571121191, -8.366608963954089262, -19.60045294882756295 ) ) ;
#2711 = CARTESIAN_POINT ( 'NONE',  ( -213.1075012329537230, 40.00000000000055422, -53.71589010953623244 ) ) ;
#2712 = CARTESIAN_POINT ( 'NONE',  ( 19.06497207195981147, 1.521599808664285085E-13, -14.19242893257840521 ) ) ;
#2713 = CARTESIAN_POINT ( 'NONE',  ( -656.9835591184084933, 39.99917881009967147, -0.5754573772625048989 ) ) ;
#2714 = DIRECTION ( 'NONE',  ( -1.000000000000000000, 0.000000000000000000, -0.000000000000000000 ) ) ;
#2715 = CARTESIAN_POINT ( 'NONE',  ( 199.0093797572272081, 19.86600527971208763, 2.306481033292959726 ) ) ;
#2716 = CARTESIAN_POINT ( 'NONE',  ( -188.2506440019711818, 13.82466072834903770, 46.97351617221500675 ) ) ;
#2717 = CARTESIAN_POINT ( 'NONE',  ( 19.06497207195981858, -38.31983398719641087, 18.24870850772724040 ) ) ;
#2718 = CARTESIAN_POINT ( 'NONE',  ( 190.0000000000001137, 3.490243377569959927E-14, 0.000000000000000000 ) ) ;
#2719 = CARTESIAN_POINT ( 'NONE',  ( 136.1360204305621551, 24.77266263493108411, 31.79587985999273769 ) ) ;
#2720 = CARTESIAN_POINT ( 'NONE',  ( -77.58208867533490150, 21.99046547477049174, -2.676519792206656589 ) ) ;
#2721 = CARTESIAN_POINT ( 'NONE',  ( -280.0000000000000000, -14.14213562373088706, -14.14213562373108424 ) ) ;
#2722 = CARTESIAN_POINT ( 'NONE',  ( -661.9203515605751136, 44.94993422606702893, 2.443437321343243429 ) ) ;
#2723 = CARTESIAN_POINT ( 'NONE',  ( -208.1127848780265026, -15.00245453012673202, 0.000000000000000000 ) ) ;
#2724 = CARTESIAN_POINT ( 'NONE',  ( -192.9588430854690273, 38.51493924976913519, 18.05360324515490333 ) ) ;
#2725 = CARTESIAN_POINT ( 'NONE',  ( 146.6084372240433993, 34.62501878078308692, 0.000000000000000000 ) ) ;
#2726 = CARTESIAN_POINT ( 'NONE',  ( -595.8013259146971450, 42.09546181640034490, -16.06146874878389141 ) ) ;
#2727 = ORIENTED_EDGE ( 'NONE', *, *, #19780, .T. ) ;
#2728 = CARTESIAN_POINT ( 'NONE',  ( 199.9999999999999432, 2.486775779033024914E-13, -19.99999999999992539 ) ) ;
#2729 = CARTESIAN_POINT ( 'NONE',  ( 199.0053214113103763, 13.24708851623085870, -15.02902163144573500 ) ) ;
#2730 = CARTESIAN_POINT ( 'NONE',  ( -200.0000000000000000, -61.50000000000001421, 66.50000000000005684 ) ) ;
#2731 = ORIENTED_EDGE ( 'NONE', *, *, #5807, .F. ) ;
#2732 = ORIENTED_EDGE ( 'NONE', *, *, #12326, .F. ) ;
#2733 = ORIENTED_EDGE ( 'NONE', *, *, #6809, .T. ) ;
#2734 = CARTESIAN_POINT ( 'NONE',  ( -105.3755690713226585, 18.24025645688349684, 40.00000000000002132 ) ) ;
#2735 = DIRECTION ( 'NONE',  ( 0.000000000000000000, -1.000000000000000000, 0.000000000000000000 ) ) ;
#2736 = CARTESIAN_POINT ( 'NONE',  ( 83.06440094959391729, 24.44702070089013901, -9.006081069718883114 ) ) ;
#2737 = CARTESIAN_POINT ( 'NONE',  ( -210.0000000000000284, -52.49999999999991473, 52.49999999999999289 ) ) ;
#2738 = PRODUCT_RELATED_PRODUCT_CATEGORY ( 'part', '', ( #24865 ) ) ;
#2739 = CARTESIAN_POINT ( 'NONE',  ( 146.6084372240433993, 1.478241399363601114E-13, -34.62501878078305850 ) ) ;
#2740 = CARTESIAN_POINT ( 'NONE',  ( 199.9999999999997726, -2.174764995058875439, -18.87968408895515182 ) ) ;
#2741 = CARTESIAN_POINT ( 'NONE',  ( 200.0000000000000000, -0.6316560126811792131, -18.99370827960111541 ) ) ;
#2742 = CARTESIAN_POINT ( 'NONE',  ( 19.06497207195980792, -18.24870850772710540, -38.31983398719647482 ) ) ;
#2743 = CARTESIAN_POINT ( 'NONE',  ( -86.96347745069644475, 15.38646221621772092, 15.38646221621800336 ) ) ;
#2744 = DIRECTION ( 'NONE',  ( 1.000000000000000000, 0.000000000000000000, 0.000000000000000000 ) ) ;
#2745 = CARTESIAN_POINT ( 'NONE',  ( -100.7734535825088500, 40.00000000000017764, -17.32597176626768487 ) ) ;
#2746 = CARTESIAN_POINT ( 'NONE',  ( -102.4068193528145940, -8.088405365069414543, 20.44188272012834418 ) ) ;
#2747 = CARTESIAN_POINT ( 'NONE',  ( -162.0762913951020892, -1.694272876828353702, 0.000000000000000000 ) ) ;
#2748 = CARTESIAN_POINT ( 'NONE',  ( -135.8532207217289738, 21.81201906317767936, 21.81201906317778239 ) ) ;
#2749 = CARTESIAN_POINT ( 'NONE',  ( 170.2234770963711128, -10.92277846919202666, 10.92277846919193962 ) ) ;
#2750 = CARTESIAN_POINT ( 'NONE',  ( 199.0114847477458397, 18.79655487626452981, 6.828771775710518632 ) ) ;
#2751 = ADVANCED_FACE ( 'NONE', ( #22759 ), #8510, .F. ) ;
#2753 = CARTESIAN_POINT ( 'NONE',  ( 199.9999999999999432, 1.065690307512836407E-13, -20.00000000000010303 ) ) ;
#2752 = CARTESIAN_POINT ( 'NONE',  ( -238.4067589809705794, -27.60227080167029001, -28.96627169325357798 ) ) ;
#2754 = DIRECTION ( 'NONE',  ( 0.000000000000000000, 0.000000000000000000, 1.000000000000000000 ) ) ;
#2755 = CARTESIAN_POINT ( 'NONE',  ( 170.2234770963711128, -45.64576402573183600, 10.92277846919191653 ) ) ;
#2756 = CARTESIAN_POINT ( 'NONE',  ( -91.56559293963834989, -22.67402823373193499, 40.00000000000002132 ) ) ;
#2757 = EDGE_LOOP ( 'NONE', ( #3114, #1049, #11674, #13097 ) ) ;
#2758 = CARTESIAN_POINT ( 'NONE',  ( 3.468680970029910604, -44.56630890487710417, 24.60338114560769185 ) ) ;
#2759 = CARTESIAN_POINT ( 'NONE',  ( -198.0356074513804572, 15.37879056873066830, -40.00000000000002132 ) ) ;
#2760 = VERTEX_POINT ( 'NONE', #2673 ) ;
#2761 = CARTESIAN_POINT ( 'NONE',  ( -87.13361725327075646, -14.71749760135919161, 15.67849882405766770 ) ) ;
#2762 = CARTESIAN_POINT ( 'NONE',  ( -56.48582580120559271, -6.472252184284187138, -6.472252184284199572 ) ) ;
#2763 = CARTESIAN_POINT ( 'NONE',  ( -3.473570583883154317, -17.93385599103746486, 43.29615835920800748 ) ) ;
#2764 = CARTESIAN_POINT ( 'NONE',  ( -259.2033419157646676, 21.55415060305839958, -35.01439189186541512 ) ) ;
#2765 = CARTESIAN_POINT ( 'NONE',  ( 0.000000000000000000, 0.000000000000000000, -75.00000000000000000 ) ) ;
#2766 = CARTESIAN_POINT ( 'NONE',  ( 199.0230409161751197, -19.98726064469808961, -0.8218112272605428981 ) ) ;
#2767 = CARTESIAN_POINT ( 'NONE',  ( 19.06497207195980792, 10.03556273973447155, -10.03556273973422286 ) ) ;
#2768 = CARTESIAN_POINT ( 'NONE',  ( -82.24289765310217604, -20.07413437147977575, 2.209159509587613535 ) ) ;
#2769 = CARTESIAN_POINT ( 'NONE',  ( 107.5473083967386572, -23.99138244111233220, 0.000000000000000000 ) ) ;
#2770 = CARTESIAN_POINT ( 'NONE',  ( -188.3392995398478149, -23.45797413244888929, 43.01688924973637285 ) ) ;
#2771 = CARTESIAN_POINT ( 'NONE',  ( 4.995406935893293543, -10.78321810388990265, -10.78321810389009272 ) ) ;
#2772 = CARTESIAN_POINT ( 'NONE',  ( 146.6084372240433709, 52.76785682606519146, 3.800685668858932775 ) ) ;
#2773 = CARTESIAN_POINT ( 'NONE',  ( -86.96347745069644475, -15.38646221621738164, -41.18208027870615240 ) ) ;
#2774 = DIRECTION ( 'NONE',  ( 1.000000000000000000, 1.836970198721030181E-16, 0.000000000000000000 ) ) ;
#2776 = CARTESIAN_POINT ( 'NONE',  ( -135.8532207217289738, 50.09629031063956006, 6.472252184284782217 ) ) ;
#2775 = CARTESIAN_POINT ( 'NONE',  ( -208.1127848780264742, 17.67593391476678377, -38.89260858015718014 ) ) ;
#2777 = CARTESIAN_POINT ( 'NONE',  ( -213.1075012329537230, 37.98287015391211696, 18.58567234101190735 ) ) ;
#2778 = CARTESIAN_POINT ( 'NONE',  ( -135.8532207217289738, 9.153146818113546246, -0.000000000000000000 ) ) ;
#2779 = CARTESIAN_POINT ( 'NONE',  ( 0.2972598230769930017, 54.33493731733938148, -40.00000000000002132 ) ) ;
#2780 = CARTESIAN_POINT ( 'NONE',  ( -162.0762913951021176, 29.48230308784768638, -27.08623940707612121 ) ) ;
#2781 = CYLINDRICAL_SURFACE ( 'NONE', #11057, 4.999999999999997335 ) ;
#2782 = CARTESIAN_POINT ( 'NONE',  ( -162.0762913951020607, -57.76657433537922515, -1.198031840455874963 ) ) ;
#2783 = DIRECTION ( 'NONE',  ( -1.000000000000000000, 1.836970198721030181E-16, 0.000000000000000000 ) ) ;
#2784 = VERTEX_POINT ( 'NONE', #24888 ) ;
#2785 = CARTESIAN_POINT ( 'NONE',  ( -259.2033419157646676, 21.55415060305830366, 21.55415060305842800 ) ) ;
#2786 = CARTESIAN_POINT ( 'NONE',  ( 210.0000000000000284, 66.50000000000009948, -66.50000000000005684 ) ) ;
#2787 = CARTESIAN_POINT ( 'NONE',  ( -192.9588430854690273, -10.23066800229550388, 66.79921049721887982 ) ) ;
#2788 = CARTESIAN_POINT ( 'NONE',  ( -2.164901439684538076, -47.64638340558528284, -13.92557459409770892 ) ) ;
#2789 = EDGE_LOOP ( 'NONE', ( #9312, #7216, #10203, #17169 ) ) ;
#2790 = CARTESIAN_POINT ( 'NONE',  ( -173.7925187073452946, -41.93431653918364788, 12.78856575065205270 ) ) ;
#2791 = CARTESIAN_POINT ( 'NONE',  ( -110.1017833366170748, -14.28014421838192405, -14.28014421838201820 ) ) ;
#2792 = EDGE_CURVE ( 'NONE', #4564, #9028, #14622, .T. ) ;
#2793 = CARTESIAN_POINT ( 'NONE',  ( 199.9999999999999716, 18.70067531203203970, -3.379044910449504169 ) ) ;
#2794 = CARTESIAN_POINT ( 'NONE',  ( 200.0000000000000000, 75.52305771588345351, -68.47933392563552957 ) ) ;
#2795 = CARTESIAN_POINT ( 'NONE',  ( -162.0762913951020892, 41.69427287692678163, -40.00000000000002132 ) ) ;
#2796 = CARTESIAN_POINT ( 'NONE',  ( 0.2972598230769938343, 10.13633138497486286, -10.13633138497461594 ) ) ;
#2797 = CARTESIAN_POINT ( 'NONE',  ( 199.0206025836015442, 6.413712542583970944, 18.94893284924772203 ) ) ;
#2798 = CIRCLE ( 'NONE', #6593, 5.000000000000004441 ) ;
#2799 = AXIS2_PLACEMENT_3D ( 'NONE', #21130, #9017, #25385 ) ;
#2800 = CARTESIAN_POINT ( 'NONE',  ( 19.06497207195982924, -66.60410523465809263, -10.03556273973493163 ) ) ;
#2801 = CARTESIAN_POINT ( 'NONE',  ( -100.7734535825088358, -8.145438380286941744E-14, 17.32597176626811120 ) ) ;
#2802 = CARTESIAN_POINT ( 'NONE',  ( 200.0000000000000000, 39.99999999999999289, 20.00000000000007105 ) ) ;
#2803 = CARTESIAN_POINT ( 'NONE',  ( -102.2610585947573441, 15.74993999358161112, -15.74993999358146191 ) ) ;
#2804 = CARTESIAN_POINT ( 'NONE',  ( 91.82158438592159655, -22.79471317813468545, -40.00000000000002132 ) ) ;
#2806 = CARTESIAN_POINT ( 'NONE',  ( -622.8837209345899737, 26.70509413432482049, 29.78579685810782252 ) ) ;
#2805 = CARTESIAN_POINT ( 'NONE',  ( 17.24092899317993144, -18.36647614517220006, -44.34059580268279888 ) ) ;
#2807 = CARTESIAN_POINT ( 'NONE',  ( -91.56559293963834989, -17.32597176626812896, -2.449293598294708485E-15 ) ) ;
#2808 = CARTESIAN_POINT ( 'NONE',  ( 200.0000000000000000, 42.42640687119290988, 14.14213562373111976 ) ) ;
#2809 = AXIS2_PLACEMENT_3D ( 'NONE', #1003, #18966, #22694 ) ;
#2810 = CARTESIAN_POINT ( 'NONE',  ( -138.9613198120156881, 10.11110880661586719, 29.42718893709540851 ) ) ;
#2811 = CARTESIAN_POINT ( 'NONE',  ( -126.6834156230552679, -11.16464796290101802, 24.04426801068220598 ) ) ;
#2812 = CARTESIAN_POINT ( 'NONE',  ( -238.4067589809705794, -40.00000000000005684, -0.9644942799830014124 ) ) ;
#2813 = PRODUCT_DEFINITION_FORMATION_WITH_SPECIFIED_SOURCE ( 'ANY', '', #15879, .NOT_KNOWN. ) ;
#2814 = CARTESIAN_POINT ( 'NONE',  ( 192.4448373802100889, -14.14213562375876698, -14.14213562375885047 ) ) ;
#2815 = CARTESIAN_POINT ( 'NONE',  ( 180.0000000000000000, 2.292407966645821729E-14, 4.683861624749757595E-30 ) ) ;
#2816 = CARTESIAN_POINT ( 'NONE',  ( -100.0753760173619185, -8.894334231739314589, -20.41987330121788702 ) ) ;
#2817 = CARTESIAN_POINT ( 'NONE',  ( 151.7948205124836534, 23.49921654116009506, 33.06932595376371609 ) ) ;
#2818 = VERTEX_POINT ( 'NONE', #540 ) ;
#2820 = CARTESIAN_POINT ( 'NONE',  ( -7.769366557094080861, 41.90323276218152415, -22.72119856430118645 ) ) ;
#2819 = CARTESIAN_POINT ( 'NONE',  ( -77.58523997990613452, -2.778549811635243838, -21.97336465817913975 ) ) ;
#2821 = CARTESIAN_POINT ( 'NONE',  ( 104.1600437297061603, 20.63676802888582884, -8.548029202070297927 ) ) ;
#2822 = CARTESIAN_POINT ( 'NONE',  ( 0.2972598230770130412, -54.33493731733936016, -2.449293598294708485E-15 ) ) ;
#2823 = CARTESIAN_POINT ( 'NONE',  ( 170.0000000000000284, -15.47746304364901171, -19.80854622259142417 ) ) ;
#2824 = CARTESIAN_POINT ( 'NONE',  ( -188.4701769959784770, 43.05504096897865907, -23.48627020870706161 ) ) ;
#2825 = ORIENTED_EDGE ( 'NONE', *, *, #22824, .F. ) ;
#2826 = ORIENTED_EDGE ( 'NONE', *, *, #15195, .T. ) ;
#2827 = CIRCLE ( 'NONE', #6201, 14.99999999999999467 ) ;
#2828 = DIRECTION ( 'NONE',  ( 1.000000000000000000, 0.000000000000000000, 0.000000000000000000 ) ) ;
#2829 = CARTESIAN_POINT ( 'NONE',  ( -86.86578273022558960, 8.153770686795043687, -19.68494377654074157 ) ) ;
#2830 = ORIENTED_EDGE ( 'NONE', *, *, #4790, .T. ) ;
#2831 = EDGE_CURVE ( 'NONE', #18337, #9825, #12145, .T. ) ;
#2832 = EDGE_LOOP ( 'NONE', ( #20393, #22553, #11090, #13813 ) ) ;
#2833 = CARTESIAN_POINT ( 'NONE',  ( 170.2234770963711128, -45.64576402573183600, 10.92277846919191653 ) ) ;
#2834 = CARTESIAN_POINT ( 'NONE',  ( 199.0145894657785846, -12.18649378798404470, -15.86093292504746621 ) ) ;
#2835 = CARTESIAN_POINT ( 'NONE',  ( -114.6097568999503125, -5.809233881211882888, 21.20070836100120815 ) ) ;
#2836 = EDGE_CURVE ( 'NONE', #4035, #6176, #5428, .T. ) ;
#2837 = CARTESIAN_POINT ( 'NONE',  ( 200.0000000000000000, -42.42640687119293119, 14.14213562373082134 ) ) ;
#2838 = CARTESIAN_POINT ( 'NONE',  ( -238.4067589809705794, 0.6820004457912757223, 0.6820004457913219076 ) ) ;
#2839 = CARTESIAN_POINT ( 'NONE',  ( -162.0762913951020892, 39.99999999999985079, 41.69427287692695216 ) ) ;
#2840 = CARTESIAN_POINT ( 'NONE',  ( -192.1167141818823154, -24.15421809699817501, 43.95739236919496307 ) ) ;
#2841 = EDGE_CURVE ( 'NONE', #7865, #20847, #25329, .T. ) ;
#2842 = EDGE_CURVE ( 'NONE', #5576, #15935, #17400, .T. ) ;
#2843 = CARTESIAN_POINT ( 'NONE',  ( -200.0000000000000000, -10.02640517461745517, 53.44529986889241968 ) ) ;
#2844 = CARTESIAN_POINT ( 'NONE',  ( -91.56559293963834989, -39.99999999999985789, -17.32597176626853042 ) ) ;
#2845 = CARTESIAN_POINT ( 'NONE',  ( 130.8568914410475088, 39.99999999999969447, 34.05028731879830417 ) ) ;
#2846 = CARTESIAN_POINT ( 'NONE',  ( -77.63478802649954957, 18.14812407464349064, 12.54968118178400083 ) ) ;
#2847 = CARTESIAN_POINT ( 'NONE',  ( -87.02160625236410851, 10.86264740421045083, 18.50711184548089960 ) ) ;
#2848 = CARTESIAN_POINT ( 'NONE',  ( 199.0060751070798233, 18.35498561216385482, -7.937441424495496278 ) ) ;
#2849 = CARTESIAN_POINT ( 'NONE',  ( -188.6013476421563553, 23.51433506916966110, 43.09288642756894205 ) ) ;
#2850 = CARTESIAN_POINT ( 'NONE',  ( 170.2234770963711128, 17.36149277826980253, 17.36149277827007253 ) ) ;
#2851 = CARTESIAN_POINT ( 'NONE',  ( -198.0012400611978194, -49.19397081476451206, 14.15884001207462184 ) ) ;
#2852 = CARTESIAN_POINT ( 'NONE',  ( -162.0762913951020607, -1.198031840455708430, 57.76657433537920383 ) ) ;
#2853 = CARTESIAN_POINT ( 'NONE',  ( -87.13348102040650645, -16.17099723934745015, 14.22374190074250855 ) ) ;
#2854 = CARTESIAN_POINT ( 'NONE',  ( -56.48582580120558561, 6.472252184284607246, -50.09629031063960269 ) ) ;
#2855 = CARTESIAN_POINT ( 'NONE',  ( -200.0000000000000000, 44.96258949770069790, -22.85346793133681942 ) ) ;
#2856 = CARTESIAN_POINT ( 'NONE',  ( -162.0762913951021176, -1.694272876828353702, 40.00000000000002132 ) ) ;
#2857 = CIRCLE ( 'NONE', #22396, 15.00000000000000000 ) ;
#2858 = ORIENTED_EDGE ( 'NONE', *, *, #9722, .F. ) ;
#2859 = CARTESIAN_POINT ( 'NONE',  ( -105.3755690713226585, 41.18208027870575449, 15.38646221621837107 ) ) ;
#2860 = CARTESIAN_POINT ( 'NONE',  ( 146.6084372240433709, 34.62501878078307982, 40.00000000000002132 ) ) ;
#2861 = CARTESIAN_POINT ( 'NONE',  ( -603.9616649909638681, 36.45097493161564728, 26.45255915120217693 ) ) ;
#2862 = VERTEX_POINT ( 'NONE', #15654 ) ;
#2863 = CARTESIAN_POINT ( 'NONE',  ( -162.0762913951021176, -40.00000000000003553, -1.694272876828743168 ) ) ;
#2864 = DIRECTION ( 'NONE',  ( 0.000000000000000000, 1.000000000000000000, 0.000000000000000000 ) ) ;
#2865 = DIRECTION ( 'NONE',  ( 0.000000000000000000, 0.6739498806388346530, 0.7387770694782699321 ) ) ;
#2866 = EDGE_LOOP ( 'NONE', ( #15413, #13992, #1635, #20909 ) ) ;
#2867 = ORIENTED_EDGE ( 'NONE', *, *, #19308, .F. ) ;
#2868 = ORIENTED_EDGE ( 'NONE', *, *, #18344, .F. ) ;
#2869 = CARTESIAN_POINT ( 'NONE',  ( 192.4448373802100889, 19.99999999996064304, 2.449293598294708485E-15 ) ) ;
#2870 = CARTESIAN_POINT ( 'NONE',  ( -105.4741150117382773, -19.60045294982706920, -8.366608964594435704 ) ) ;
#2871 = B_SPLINE_CURVE_WITH_KNOTS ( 'NONE', 3,
 ( #11575, #19442, #3601, #11710, #15823, #13832, #21967, #2145, #18096, #273, #8120, #11844, #6260, #16365, #26104, #10255, #7842, #16237, #18364, #7980, #16098, #9854, #22377, #20238, #18222, #10382 ),
 .UNSPECIFIED., .F., .F.,
 ( 4, 2, 1, 2, 2, 2, 2, 2, 2, 2, 2, 1, 2, 4 ),
 ( -5.999999999281531560E-08, 0.0004354487530732486806, 0.0008709575061464901744, 0.001741975012292972837, 0.003484010024585937945, 0.006968080049171867726, 0.01045215007375779881, 0.01393622009834372642, 0.02090436014751559032, 0.02438843017210151967, 0.02613046518439449128, 0.02700148269054098230, 0.02743699144361422607, 0.02787250019668746984 ),
 .UNSPECIFIED. ) ;
#2872 = CARTESIAN_POINT ( 'NONE',  ( -110.0723150831393582, -19.55249150545847314, -5.015078513992241582 ) ) ;
#2873 = DIRECTION ( 'NONE',  ( -0.000000000000000000, 1.000000000000000000, -0.000000000000000000 ) ) ;
#2874 = CARTESIAN_POINT ( 'NONE',  ( 199.9999999999997726, 10.29466221862743680, -15.97248499526360987 ) ) ;
#2875 = CARTESIAN_POINT ( 'NONE',  ( 199.9999999999999147, -6.120187099840395106, -17.99310556315726117 ) ) ;
#2876 = CARTESIAN_POINT ( 'NONE',  ( 4.995406935893294431, -17.50105314357144337, -39.06748935135212264 ) ) ;
#2877 = CARTESIAN_POINT ( 'NONE',  ( 0.2972598230769976091, -10.13633138497465147, -10.13633138497482733 ) ) ;
#2878 = CARTESIAN_POINT ( 'NONE',  ( -77.78698662148927667, -19.58754019070067542, -9.956326400803837018 ) ) ;
#2879 = CARTESIAN_POINT ( 'NONE',  ( -208.1127848780265026, 5.403397259664334602E-13, -55.00245453012672670 ) ) ;
#2880 = CARTESIAN_POINT ( 'NONE',  ( -200.0000000000000000, -66.50000000000001421, -66.50000000000005684 ) ) ;
#2881 = CARTESIAN_POINT ( 'NONE',  ( 14.38125909742181285, -15.17850393972633505, 0.000000000000000000 ) ) ;
#2882 = CARTESIAN_POINT ( 'NONE',  ( -100.7734535825088500, 16.03295912088683295, 40.53558337403684675 ) ) ;
#2883 = CARTESIAN_POINT ( 'NONE',  ( 199.0060844782017000, 18.36908416490651064, -7.898827608825804703 ) ) ;
#2885 = CARTESIAN_POINT ( 'NONE',  ( -91.56559293963836410, 40.00000000000008527, -22.67402823373177867 ) ) ;
#2884 = CARTESIAN_POINT ( 'NONE',  ( 170.2234770963711128, -17.36149277826940462, -39.20704971665412586 ) ) ;
#2886 = CARTESIAN_POINT ( 'NONE',  ( 184.8905102610680444, -20.92133201514440799, -40.00000000000002132 ) ) ;
#2887 = CARTESIAN_POINT ( 'NONE',  ( 184.8905102610680444, -43.07788698682576722, 13.49065550809799063 ) ) ;
#2888 = CARTESIAN_POINT ( 'NONE',  ( -135.8532207217289738, 30.84685318188643421, 40.00000000000002132 ) ) ;
#2889 = VERTEX_POINT ( 'NONE', #13163 ) ;
#2890 = CARTESIAN_POINT ( 'NONE',  ( 9.028290303213244883, -44.88859993224341594, 18.59346688786898483 ) ) ;
#2891 = CARTESIAN_POINT ( 'NONE',  ( 146.6084372240433709, 5.374981219217002781, -40.00000000000002132 ) ) ;
#2892 = LINE ( 'NONE', #15368, #5991 ) ;
#2893 = CARTESIAN_POINT ( 'NONE',  ( 19.06497207195981147, 38.31983398719620482, 38.31983398719633271 ) ) ;
#2894 = CARTESIAN_POINT ( 'NONE',  ( 170.2234770963711128, 1.169953928977015745E-13, -24.55285855007187124 ) ) ;
#2895 = CARTESIAN_POINT ( 'NONE',  ( -77.72572481383096488, 21.21966553434844727, -5.751841496721930014 ) ) ;
#2896 = B_SPLINE_CURVE_WITH_KNOTS ( 'NONE', 3,
 ( #23764, #9667, #21521, #11391, #17771, #13779 ),
 .UNSPECIFIED., .F., .F.,
 ( 4, 2, 4 ),
 ( 3.570546400823084320E-15, 0.03937634048171164552, 0.07875268096341971058 ),
 .UNSPECIFIED. ) ;
#2897 = CARTESIAN_POINT ( 'NONE',  ( 23.09931156284629949, -13.81622350327199378, -46.91113948292964864 ) ) ;
#2898 = CARTESIAN_POINT ( 'NONE',  ( 199.0254590212676078, -18.72437106667806717, 7.049340093992902290 ) ) ;
#2899 = EDGE_CURVE ( 'NONE', #2983, #16736, #10016, .T. ) ;
#2900 = CARTESIAN_POINT ( 'NONE',  ( -280.0000000000000568, 42.42640687119265408, 14.14213562373147504 ) ) ;
#2901 = CARTESIAN_POINT ( 'NONE',  ( -87.12800209209292746, 1.368681197224306478, 21.45652401693913092 ) ) ;
#2902 = CARTESIAN_POINT ( 'NONE',  ( -188.3120606736018772, -23.45204117844399860, 43.00889065702907033 ) ) ;
#2903 = CARTESIAN_POINT ( 'NONE',  ( -259.2033419157646676, 6.730120644403426944, 6.730120644403592145 ) ) ;
#2904 = CARTESIAN_POINT ( 'NONE',  ( -208.1127848780264742, 17.67593391476624021, 38.89260858015742883 ) ) ;
#2905 = CARTESIAN_POINT ( 'NONE',  ( 130.8568914410475372, -24.07718906447255947, 24.07718906447199458 ) ) ;
#2906 = CARTESIAN_POINT ( 'NONE',  ( -30.26275506840325136, 27.08623969584614244, -29.48230279907770779 ) ) ;
#2908 = CARTESIAN_POINT ( 'NONE',  ( 200.0000000000000000, 14.14213562373041455, 42.42640687119311593 ) ) ;
#2907 = CARTESIAN_POINT ( 'NONE',  ( 184.8905102610680444, 14.79361573936375507, 14.79361573936398067 ) ) ;
#2909 = CARTESIAN_POINT ( 'NONE',  ( -213.1075012329537230, 9.698598906438871126, -66.26714140136179765 ) ) ;
#2910 = CARTESIAN_POINT ( 'NONE',  ( -208.1127848780264742, 15.00245453012665742, -40.00000000000002132 ) ) ;
#2911 = CARTESIAN_POINT ( 'NONE',  ( 91.82158438592158234, 44.40256751092336884, -12.16597498400043342 ) ) ;
#2912 = FACE_OUTER_BOUND ( 'NONE', #21555, .T. ) ;
#2913 = CARTESIAN_POINT ( 'NONE',  ( -135.8532207217289738, -50.09629031063973770, 6.472252184283735943 ) ) ;
#2914 = CARTESIAN_POINT ( 'NONE',  ( -188.9001212172966007, 43.30535683045355455, -17.93766612258001913 ) ) ;
#2915 = VERTEX_POINT ( 'NONE', #23778 ) ;
#2916 = CARTESIAN_POINT ( 'NONE',  ( 170.2234770963711128, -17.36149277826995885, 39.20704971665388427 ) ) ;
#2917 = CARTESIAN_POINT ( 'NONE',  ( -77.55640685885761343, -16.62871490253266771, -14.66974043287744323 ) ) ;
#2918 = CARTESIAN_POINT ( 'NONE',  ( -162.0762913951021176, 27.08623940707598265, 29.48230308784781428 ) ) ;
#2919 = DIRECTION ( 'NONE',  ( 1.000000000000000000, 1.836970198721030181E-16, 0.000000000000000000 ) ) ;
#2920 = ORIENTED_EDGE ( 'NONE', *, *, #20292, .T. ) ;
#2921 = CARTESIAN_POINT ( 'NONE',  ( -188.2652133075326049, -42.99509596150239332, 23.44262061655336993 ) ) ;
#2922 = CARTESIAN_POINT ( 'NONE',  ( 199.9999999999999147, -6.121038220875967717, -17.99280653461927315 ) ) ;
#2923 = CARTESIAN_POINT ( 'NONE',  ( 190.0000000000000000, 71.50000000000009948, 66.50000000000005684 ) ) ;
#2924 = CARTESIAN_POINT ( 'NONE',  ( 4.995406935893288214, 15.24977328854832770, 0.000000000000000000 ) ) ;
#2925 = CARTESIAN_POINT ( 'NONE',  ( 180.0000000000000284, -125.7889608577475684, -82.49999999999998579 ) ) ;
#2926 = CARTESIAN_POINT ( 'NONE',  ( 199.0173417939125784, 12.16728005963107329, 15.88742495833056800 ) ) ;
#2927 = CARTESIAN_POINT ( 'NONE',  ( 91.82158438592156813, -16.11829626348459144, 40.45024623143943643 ) ) ;
#2928 = CARTESIAN_POINT ( 'NONE',  ( 136.1360204305621551, -40.00000000000001421, 4.966164525586921563 ) ) ;
#2929 = CARTESIAN_POINT ( 'NONE',  ( 4.995406935893290878, -5.232665749138292703E-14, 15.24977328854832592 ) ) ;
#2930 = CARTESIAN_POINT ( 'NONE',  ( -2.654373026594475160, 47.46285323120928723, -13.89837698318162218 ) ) ;
#2931 = CARTESIAN_POINT ( 'NONE',  ( 14.38125909742181285, -15.17850393972633505, -40.00000000000002132 ) ) ;
#2933 = CARTESIAN_POINT ( 'NONE',  ( 57.59792236341147031, 1.722363176415065089, -1.722363176415036445 ) ) ;
#2932 = CARTESIAN_POINT ( 'NONE',  ( 23.46661716383010088, -13.79413593526223103, -46.77475180958838052 ) ) ;
#2934 = CARTESIAN_POINT ( 'NONE',  ( 0.2972598230769983307, -14.33493731733933352, 40.00000000000002132 ) ) ;
#2935 = CARTESIAN_POINT ( 'NONE',  ( 57.59792236341146321, 40.00000000000000711, 2.435789363418579434 ) ) ;
#2936 = CARTESIAN_POINT ( 'NONE',  ( -110.1017491837771303, 13.37584907585219440, -15.18340520632207102 ) ) ;
#2937 = CARTESIAN_POINT ( 'NONE',  ( -198.0356074513804572, -39.99999999999948130, -55.37879056874863437 ) ) ;
#2938 = CARTESIAN_POINT ( 'NONE',  ( -238.4067589809705794, 0.6820004457912757223, 0.6820004457913219076 ) ) ;
#2939 = CARTESIAN_POINT ( 'NONE',  ( 155.4806860510508670, -27.66458559364820857, -11.45904655032044239 ) ) ;
#2940 = CARTESIAN_POINT ( 'NONE',  ( -100.7734535825088358, -16.03295912088728770, 16.03295912088687913 ) ) ;
#2941 = CARTESIAN_POINT ( 'NONE',  ( 57.59792236341147031, 30.00663442387683588, 26.56190807104703211 ) ) ;
#2942 = ORIENTED_EDGE ( 'NONE', *, *, #9722, .T. ) ;
#2944 = CARTESIAN_POINT ( 'NONE',  ( -5.866564133099172018, 46.35727274689134703, -13.69896896866313796 ) ) ;
#2943 = CARTESIAN_POINT ( 'NONE',  ( -135.8532207217289738, 6.472252184284096543, 6.472252184284234211 ) ) ;
#2945 = CARTESIAN_POINT ( 'NONE',  ( 169.9999999999999716, 22.62041470344888339, -9.369682556672254137 ) ) ;
#2946 = CARTESIAN_POINT ( 'NONE',  ( -30.26275506840324425, -1.694272468446265334, 40.00000000000002132 ) ) ;
#2947 = AXIS2_PLACEMENT_3D ( 'NONE', #6165, #26280, #1916 ) ;
#2948 = CARTESIAN_POINT ( 'NONE',  ( -190.0144222802854586, 47.57278142029252166, -13.91469272132485280 ) ) ;
#2949 = CARTESIAN_POINT ( 'NONE',  ( 0.000000000000000000, 0.000000000000000000, 0.000000000000000000 ) ) ;
#2950 = EDGE_LOOP ( 'NONE', ( #17042, #10599, #1432, #9437 ) ) ;
#2951 = EDGE_LOOP ( 'NONE', ( #2702, #19675, #20637, #14350 ) ) ;
#2952 = CARTESIAN_POINT ( 'NONE',  ( 199.9999999999999716, -11.08296553609489798, 15.44857252758585631 ) ) ;
#2953 = CARTESIAN_POINT ( 'NONE',  ( 170.0000000000000853, 9.369682556672316309, -22.62041470344884075 ) ) ;
#2954 = CARTESIAN_POINT ( 'NONE',  ( -198.0012401002533409, 44.79720214428365921, -24.77357857137243613 ) ) ;
#2955 = VERTEX_POINT ( 'NONE', #11160 ) ;
#2956 = CARTESIAN_POINT ( 'NONE',  ( 199.0186803405091780, -17.32754287553631301, -9.995805879000721816 ) ) ;
#2957 = LINE ( 'NONE', #11067, #16649 ) ;
#2958 = CARTESIAN_POINT ( 'NONE',  ( -198.0356074513804572, 10.87444709758468875, 67.44298959250869530 ) ) ;
#2959 = CARTESIAN_POINT ( 'NONE',  ( -83.21262154144073975, 13.72187187061437541, 33.12752917118392304 ) ) ;
#2960 = CARTESIAN_POINT ( 'NONE',  ( -30.26275506840324425, 39.99999999999987210, 41.69427246844643520 ) ) ;
#2961 = CARTESIAN_POINT ( 'NONE',  ( -199.9999999999999432, -48.59548038928831204, 14.89048929005521416 ) ) ;
#2962 = LINE ( 'NONE', #21056, #3828 ) ;
#2963 = CARTESIAN_POINT ( 'NONE',  ( -208.1127848780264742, -39.99999999999990763, -15.00245453012711394 ) ) ;
#2964 = CARTESIAN_POINT ( 'NONE',  ( 130.8568914410475088, 40.00000000000011369, -5.949712681206269949 ) ) ;
#2965 = CARTESIAN_POINT ( 'NONE',  ( 190.0000000000000000, -71.50000000000002842, -66.50000000000005684 ) ) ;
#2966 = FACE_OUTER_BOUND ( 'NONE', #1995, .T. ) ;
#2967 = CARTESIAN_POINT ( 'NONE',  ( -199.9999999999999716, 14.87399974031265337, -48.57705986237285600 ) ) ;
#2968 = CARTESIAN_POINT ( 'NONE',  ( 130.8568914410475372, 24.07718906447243867, -24.07718906447216156 ) ) ;
#2969 = CARTESIAN_POINT ( 'NONE',  ( 146.5090579137181805, 29.94463907179409290, 12.40347562390452651 ) ) ;
#2970 = ADVANCED_FACE ( 'NONE', ( #25664 ), #17526, .T. ) ;
#2971 = VECTOR ( 'NONE', #12257, 1000.000000000000000 ) ;
#2972 = DIRECTION ( 'NONE',  ( -1.303213150798907793E-16, 1.000000000000000000, -1.682156097916904081E-16 ) ) ;
#2973 = CARTESIAN_POINT ( 'NONE',  ( 136.1360204305621266, 53.05693388239316022, 3.511608612530967566 ) ) ;
#2974 = CARTESIAN_POINT ( 'NONE',  ( -77.70606139385991185, 21.32448501951759923, -5.419212411896500825 ) ) ;
#2975 = CARTESIAN_POINT ( 'NONE',  ( -280.0000000000000568, -14.14213562373137556, 42.42640687119276066 ) ) ;
#2976 = CARTESIAN_POINT ( 'NONE',  ( -645.5897708877611194, 33.84656210914351959, -29.66564330929828230 ) ) ;
#2977 = CARTESIAN_POINT ( 'NONE',  ( 1.564253033640323531, 24.39614062124472937, 44.28527310957323238 ) ) ;
#2978 = ORIENTED_EDGE ( 'NONE', *, *, #9553, .T. ) ;
#2979 = CARTESIAN_POINT ( 'NONE',  ( 4.995406935893286438, 67.35176059880245703, -10.78321810387767066 ) ) ;
#2980 = ADVANCED_FACE ( 'NONE', ( #9043 ), #15154, .F. ) ;
#2981 = CARTESIAN_POINT ( 'NONE',  ( -716.9846540392142060, -66.50000000000001421, 66.50000000000005684 ) ) ;
#2982 = CARTESIAN_POINT ( 'NONE',  ( -596.9048215538962268, 41.27960141593418797, -18.03334258849684701 ) ) ;
#2983 = VERTEX_POINT ( 'NONE', #7410 ) ;
#2984 = CARTESIAN_POINT ( 'NONE',  ( -238.4067589809705794, -40.00000000000005684, -0.9644942799830014124 ) ) ;
#2985 = EDGE_CURVE ( 'NONE', #23734, #20976, #1059, .T. ) ;
#2986 = CARTESIAN_POINT ( 'NONE',  ( 199.0053211804427633, 14.13331159297750617, -14.14343255912447361 ) ) ;
#2987 = ADVANCED_FACE ( 'NONE', ( #7162 ), #15524, .T. ) ;
#2988 = CARTESIAN_POINT ( 'NONE',  ( 0.000000000000000000, 0.000000000000000000, 0.000000000000000000 ) ) ;
#2989 = VERTEX_POINT ( 'NONE', #5300 ) ;
#2990 = ORIENTED_EDGE ( 'NONE', *, *, #13522, .F. ) ;
#2991 = ORIENTED_EDGE ( 'NONE', *, *, #24197, .T. ) ;
#2992 = CARTESIAN_POINT ( 'NONE',  ( 199.9999999999999432, 19.99999999999996092, 2.449293598294708485E-15 ) ) ;
#2993 = PRODUCT_DEFINITION_CONTEXT ( 'detailed design', #22452, 'design' ) ;
#2994 = PRESENTATION_STYLE_ASSIGNMENT (( #16819 ) ) ;
#2995 = CIRCLE ( 'NONE', #13180, 15.00000000000000355 ) ;
#2996 = LINE ( 'NONE', #20826, #10015 ) ;
#2997 = CARTESIAN_POINT ( 'NONE',  ( 170.2234770963711128, 1.169953928977015745E-13, -24.55285855007187124 ) ) ;
#2998 = CARTESIAN_POINT ( 'NONE',  ( 200.0000000000000284, -14.89093438834758842, -11.81132417993805639 ) ) ;
#2999 = CARTESIAN_POINT ( 'NONE',  ( 151.7948205124836250, -23.49921654116371883, 23.49921654116317526 ) ) ;
#3000 = CARTESIAN_POINT ( 'NONE',  ( -56.48582580120559271, 6.472252184284121412, 6.472252184284244869 ) ) ;
#3001 = EDGE_CURVE ( 'NONE', #3196, #9833, #7031, .T. ) ;
#3002 = CARTESIAN_POINT ( 'NONE',  ( -105.3844635030161641, -19.12027419152980556, -9.640654680272803034 ) ) ;
#3003 = CARTESIAN_POINT ( 'NONE',  ( 136.1360204305621551, -39.99999999999994316, -4.966164525587488221 ) ) ;
#3004 = CARTESIAN_POINT ( 'NONE',  ( 192.4448373802101173, -14.14213562370342281, 42.42640687122062104 ) ) ;
#3005 = CARTESIAN_POINT ( 'NONE',  ( 170.2234770963711128, 24.55285855007190676, -40.00000000000002132 ) ) ;
#3006 = CARTESIAN_POINT ( 'NONE',  ( -30.26275506840323359, -1.198031551616339341, 57.76657404653985139 ) ) ;
#3007 = CARTESIAN_POINT ( 'NONE',  ( 199.0094106630088220, 19.89429631425563372, 2.408647560944259691 ) ) ;
#3008 = AXIS2_PLACEMENT_3D ( 'NONE', #5611, #15208, #23458 ) ;
#3010 = CARTESIAN_POINT ( 'NONE',  ( -259.2033419157646676, 40.00000000000000711, -9.517827891722491884 ) ) ;
#3009 = CARTESIAN_POINT ( 'NONE',  ( 170.2234770963711128, -45.64576402573167258, -10.92277846919254891 ) ) ;
#3011 = CARTESIAN_POINT ( 'NONE',  ( 91.82158438592158234, -17.20528682183298486, 0.000000000000000000 ) ) ;
#3012 = CARTESIAN_POINT ( 'NONE',  ( 146.6084372240433709, -52.76785682606516303, 3.800685668858563737 ) ) ;
#3013 = EDGE_CURVE ( 'NONE', #5580, #5450, #16402, .T. ) ;
#3014 = CARTESIAN_POINT ( 'NONE',  ( -259.2033419157646676, -9.517827891722680178, 40.00000000000002132 ) ) ;
#3015 = EDGE_LOOP ( 'NONE', ( #9374, #9694, #24059, #25401, #24348, #5735 ) ) ;
#3016 = CARTESIAN_POINT ( 'NONE',  ( 22.72189371636510202, -47.04833883279060558, 13.83659596078687493 ) ) ;
#3017 = CARTESIAN_POINT ( 'NONE',  ( 130.8568914410475088, -34.05028731879786363, -40.00000000000002132 ) ) ;
#3018 = CARTESIAN_POINT ( 'NONE',  ( 169.9999999999999716, -22.62041470344880523, -9.369682556672316309 ) ) ;
#3019 = CARTESIAN_POINT ( 'NONE',  ( 151.7948205124836250, 4.785054706301690608, 4.785054706301682614 ) ) ;
#3020 = DIRECTION ( 'NONE',  ( 0.000000000000000000, 0.000000000000000000, 1.000000000000000000 ) ) ;
#3021 = CARTESIAN_POINT ( 'NONE',  ( -86.91081356576945893, 20.06298749293320682, -7.308700132831655871 ) ) ;
#3022 = AXIS2_PLACEMENT_3D ( 'NONE', #23693, #13325, #5473 ) ;
#3023 = CARTESIAN_POINT ( 'NONE',  ( 199.0053211798077086, 14.13837298227953987, -14.13837298578013701 ) ) ;
#3024 = CARTESIAN_POINT ( 'NONE',  ( 200.0000000000001421, -10.70065846580424207, 15.71346033962178446 ) ) ;
#3025 = CARTESIAN_POINT ( 'NONE',  ( 163.1118516004056573, 9.006482792073693844, 47.56205970284970164 ) ) ;
#3026 = CARTESIAN_POINT ( 'NONE',  ( 146.6084372240433993, -34.62501878078303008, 0.000000000000000000 ) ) ;
#3027 = CARTESIAN_POINT ( 'NONE',  ( 151.7948205124836250, -3.202120068677277203E-13, 33.23291073765553705 ) ) ;
#3028 = CARTESIAN_POINT ( 'NONE',  ( -259.2033419157646676, 35.01439189186528722, 21.55415060305857011 ) ) ;
#3029 = FACE_OUTER_BOUND ( 'NONE', #3584, .T. ) ;
#3030 = CARTESIAN_POINT ( 'NONE',  ( 0.000000000000000000, 9.184850993605148733E-15, 75.00000000000000000 ) ) ;
#3032 = CARTESIAN_POINT ( 'NONE',  ( 146.6084372240433993, 3.800685668858732935, -3.800685668858610367 ) ) ;
#3031 = CARTESIAN_POINT ( 'NONE',  ( 199.9999999999999432, 14.14213562373093680, 14.14213562373114641 ) ) ;
#3033 = CARTESIAN_POINT ( 'NONE',  ( -162.0762913951020892, 1.198031840456041497, -57.76657433537918251 ) ) ;
#3034 = CARTESIAN_POINT ( 'NONE',  ( 200.0000000000000000, -20.00000000000006750, -40.00000000000002132 ) ) ;
#3035 = CARTESIAN_POINT ( 'NONE',  ( -86.96347745069644475, -15.38646221621786125, -15.38646221621789856 ) ) ;
#3036 = DIRECTION ( 'NONE',  ( 0.000000000000000000, 0.000000000000000000, 1.000000000000000000 ) ) ;
#3037 = CARTESIAN_POINT ( 'NONE',  ( -192.9588430854690273, -66.79921049721887982, -10.23066800229569040 ) ) ;
#3038 = VECTOR ( 'NONE', #12658, 1000.000000000000000 ) ;
#3039 = CARTESIAN_POINT ( 'NONE',  ( -121.8425418703243110, 22.74408241228373484, -9.420907402774027162 ) ) ;
#3040 = VERTEX_POINT ( 'NONE', #22202 ) ;
#3041 = CARTESIAN_POINT ( 'NONE',  ( 0.2972598230770011618, 10.13633138497462305, 66.70487387989858519 ) ) ;
#3042 = CIRCLE ( 'NONE', #25569, 5.000000000000004441 ) ;
#3043 = DIRECTION ( 'NONE',  ( 0.000000000000000000, 0.000000000000000000, 1.000000000000000000 ) ) ;
#3044 = CARTESIAN_POINT ( 'NONE',  ( -3.534370630407282832, -43.27979241395900090, -17.92707699455385750 ) ) ;
#3045 = EDGE_LOOP ( 'NONE', ( #5456, #12790, #12055, #22189 ) ) ;
#3046 = CARTESIAN_POINT ( 'NONE',  ( -114.4388184736424705, -20.16431396440406232, 8.352332320010008360 ) ) ;
#3047 = CARTESIAN_POINT ( 'NONE',  ( 199.9999999999999147, 0.2978356717867484682, -19.00168788844713319 ) ) ;
#3048 = CARTESIAN_POINT ( 'NONE',  ( 25.88393124174758597, -13.61573025394965164, 45.90075965688545523 ) ) ;
#3049 = DIRECTION ( 'NONE',  ( -1.000000000000000000, -0.000000000000000000, -0.000000000000000000 ) ) ;
#3050 = CARTESIAN_POINT ( 'NONE',  ( 199.0082178062215803, 19.99654772287713911, -0.6402344634765599896 ) ) ;
#3051 = AXIS2_PLACEMENT_3D ( 'NONE', #24614, #22620, #12897 ) ;
#3052 = ADVANCED_FACE ( 'NONE', ( #24186 ), #26266, .T. ) ;
#3053 = CARTESIAN_POINT ( 'NONE',  ( -105.3755690713226585, -41.18208027870611687, 15.38646221621750954 ) ) ;
#3054 = CARTESIAN_POINT ( 'NONE',  ( -280.0000000000000000, 1.839446121267387017E-14, -20.00000000000001421 ) ) ;
#3055 = DIRECTION ( 'NONE',  ( -1.000000000000000000, 0.000000000000000000, -0.000000000000000000 ) ) ;
#3056 = PRODUCT_RELATED_PRODUCT_CATEGORY ( 'part', '', ( #10623 ) ) ;
#3057 = CARTESIAN_POINT ( 'NONE',  ( -210.0000000000000284, 0.000000000000000000, 0.000000000000000000 ) ) ;
#3058 = CARTESIAN_POINT ( 'NONE',  ( -280.0000000000000000, -20.00000000000006750, -2.449293598294708485E-15 ) ) ;
#3060 = CARTESIAN_POINT ( 'NONE',  ( -599.0758207628625769, 38.45631679711321738, 11.01587919049791076 ) ) ;
#3059 = CARTESIAN_POINT ( 'NONE',  ( 23.36462152323027297, -13.80148662728946896, -46.81175967489690493 ) ) ;
#3061 = CARTESIAN_POINT ( 'NONE',  ( 136.1360204305621266, 35.03383547441298163, 40.00000000000002132 ) ) ;
#3062 = EDGE_CURVE ( 'NONE', #2595, #17934, #24018, .T. ) ;
#3063 = CARTESIAN_POINT ( 'NONE',  ( -198.0356074513804572, -10.87444709759729911, 10.87444709759714812 ) ) ;
#3064 = CARTESIAN_POINT ( 'NONE',  ( -30.26275506840325136, 40.00000000000003553, -1.694272468445841007 ) ) ;
#3065 = CARTESIAN_POINT ( 'NONE',  ( -110.0368417077424681, 7.992411109430601179, -18.51665893310733324 ) ) ;
#3066 = CARTESIAN_POINT ( 'NONE',  ( -192.9588430854690273, -39.99999999999948841, -54.46834944098263520 ) ) ;
#3067 = CARTESIAN_POINT ( 'NONE',  ( 199.0258313909553749, -8.851116586292111066, 17.94317422212728630 ) ) ;
#3068 = CARTESIAN_POINT ( 'NONE',  ( -716.9846540392142060, 66.50000000000009948, -66.50000000000005684 ) ) ;
#3069 = CARTESIAN_POINT ( 'NONE',  ( -213.1075012329537230, 37.98287015391211696, 18.58567234101190735 ) ) ;
#3070 = CARTESIAN_POINT ( 'NONE',  ( -91.56559293963836410, 44.31723036834890905, 12.25131212657507795 ) ) ;
#3071 = EDGE_CURVE ( 'NONE', #10709, #25674, #16221, .T. ) ;
#3072 = ORIENTED_EDGE ( 'NONE', *, *, #11755, .F. ) ;
#3074 = CARTESIAN_POINT ( 'NONE',  ( -2.004660104950324762, 43.67474423979815867, -18.09067139733604179 ) ) ;
#3073 = CYLINDRICAL_SURFACE ( 'NONE', #6053, 5.000000000000004441 ) ;
#3075 = CARTESIAN_POINT ( 'NONE',  ( 57.59792236341148453, -37.56421063658185489, 40.00000000000002132 ) ) ;
#3076 = EDGE_CURVE ( 'NONE', #23087, #10307, #2081, .T. ) ;
#3077 = CARTESIAN_POINT ( 'NONE',  ( -190.5535326093529704, 43.70552662393590282, -18.10342187829310134 ) ) ;
#3078 = DIRECTION ( 'NONE',  ( 1.000000000000000000, 3.673940397442060361E-16, -1.282749433769087757E-30 ) ) ;
#3079 = ORIENTED_EDGE ( 'NONE', *, *, #23863, .T. ) ;
#3080 = EDGE_LOOP ( 'NONE', ( #9441, #19397, #23709, #22220 ) ) ;
#3081 = AXIS2_PLACEMENT_3D ( 'NONE', #17412, #7552, #23664 ) ;
#3082 = CARTESIAN_POINT ( 'NONE',  ( 200.0000000000000000, -69.99999999999985789, 0.000000000000000000 ) ) ;
#3083 = FACE_OUTER_BOUND ( 'NONE', #3494, .T. ) ;
#3084 = CARTESIAN_POINT ( 'NONE',  ( 160.7895100360958622, 1.290018736498604486E-13, -28.48799984206441138 ) ) ;
#3085 = EDGE_LOOP ( 'NONE', ( #20124, #5286, #15365, #2593 ) ) ;
#3086 = CARTESIAN_POINT ( 'NONE',  ( 199.0263606093525652, -14.93202714917829965, 13.31409215216611663 ) ) ;
#3087 = DIRECTION ( 'NONE',  ( -1.000000000000000000, 0.000000000000000000, 0.000000000000000000 ) ) ;
#3088 = CARTESIAN_POINT ( 'NONE',  ( -100.7734535825088500, -16.03295912088716335, 40.53558337403673306 ) ) ;
#3089 = CARTESIAN_POINT ( 'NONE',  ( -192.9588430854689989, 10.23066800230742679, 10.23066800230749607 ) ) ;
#3090 = CARTESIAN_POINT ( 'NONE',  ( 151.7948205124836534, 40.00000000000017053, -33.23291073765538783 ) ) ;
#3091 = CARTESIAN_POINT ( 'NONE',  ( 210.0000000000000284, 66.50000000000009948, -66.50000000000005684 ) ) ;
#3092 = CARTESIAN_POINT ( 'NONE',  ( -716.9846540392142060, -82.49999999999991473, -52.49999999999977973 ) ) ;
#3093 = CARTESIAN_POINT ( 'NONE',  ( -280.0000000000000568, -39.99999999999987210, -20.00000000000043343 ) ) ;
#3094 = CARTESIAN_POINT ( 'NONE',  ( -105.3755690713226727, 1.741486606973311632E-13, -18.24025645688352881 ) ) ;
#3095 = CARTESIAN_POINT ( 'NONE',  ( -114.4364955367319965, -20.04994829327483075, 8.644468109212210649 ) ) ;
#3096 = CARTESIAN_POINT ( 'NONE',  ( 91.82158438592158234, 12.16597498397773869, -12.16597498397759303 ) ) ;
#3097 = CARTESIAN_POINT ( 'NONE',  ( -200.0000000000000000, 71.50000000000009948, -66.50000000000005684 ) ) ;
#3098 = CARTESIAN_POINT ( 'NONE',  ( 167.0466155511619775, 23.44215416552593823, 9.710058186601706609 ) ) ;
#3099 = CARTESIAN_POINT ( 'NONE',  ( -189.4799703873392787, -47.39666448643377805, 13.88847319136879221 ) ) ;
#3100 = DIRECTION ( 'NONE',  ( 0.000000000000000000, 1.000000000000000000, 0.000000000000000000 ) ) ;
#3101 = CARTESIAN_POINT ( 'NONE',  ( -82.23724611271893536, -13.84097227486369874, 14.71983334136218602 ) ) ;
#3102 = CARTESIAN_POINT ( 'NONE',  ( 0.2972598230770153171, -66.70487387989849992, -10.13633138497533004 ) ) ;
#3103 = CARTESIAN_POINT ( 'NONE',  ( -638.5875168204022430, 30.55437902294503161, -33.04080401100450359 ) ) ;
#3104 = CARTESIAN_POINT ( 'NONE',  ( -77.55640685876518603, 15.64922766773203122, 15.64922766773211471 ) ) ;
#3105 = ORIENTED_EDGE ( 'NONE', *, *, #16287, .F. ) ;
#3106 = CARTESIAN_POINT ( 'NONE',  ( -135.8532207217289738, -6.472252184283586729, -50.09629031063973770 ) ) ;
#3107 = CARTESIAN_POINT ( 'NONE',  ( -315.0000000000000568, -4.857225732735059864E-14, 21.53474504356810115 ) ) ;
#3108 = CARTESIAN_POINT ( 'NONE',  ( -617.0039382655427289, 29.98920333220143419, 33.55165781079447385 ) ) ;
#3109 = ORIENTED_EDGE ( 'NONE', *, *, #9480, .F. ) ;
#3110 = CARTESIAN_POINT ( 'NONE',  ( 91.82158438592159655, -40.00000000000017764, 17.20528682183258340 ) ) ;
#3111 = CARTESIAN_POINT ( 'NONE',  ( 199.0230723762332161, -19.99042835476056368, -0.7383407320838223376 ) ) ;
#3112 = CARTESIAN_POINT ( 'NONE',  ( 17.75917276260962652, -44.20478326162357519, 24.33671690504831986 ) ) ;
#3113 = VERTEX_POINT ( 'NONE', #16438 ) ;
#3114 = ORIENTED_EDGE ( 'NONE', *, *, #15003, .T. ) ;
#3115 = CARTESIAN_POINT ( 'NONE',  ( -259.2033419157646676, 30.48217210827734647, 40.00000000000002132 ) ) ;
#3116 = CARTESIAN_POINT ( 'NONE',  ( 19.06497207195981147, -10.03556273973439517, 10.03556273973429214 ) ) ;
#3117 = CARTESIAN_POINT ( 'NONE',  ( 0.000000000000000000, 0.000000000000000000, -44.99999999999997158 ) ) ;
#3118 = EDGE_CURVE ( 'NONE', #3897, #22348, #16821, .T. ) ;
#3119 = PRODUCT_DEFINITION_CONTEXT ( 'detailed design', #23780, 'design' ) ;
#3120 = DIRECTION ( 'NONE',  ( 0.000000000000000000, 0.000000000000000000, 1.000000000000000000 ) ) ;
#3121 = CARTESIAN_POINT ( 'NONE',  ( -259.2033419157646676, -40.00000000000003553, -9.517827891722768996 ) ) ;
#3122 = CARTESIAN_POINT ( 'NONE',  ( 199.9999999999999716, -17.78976893299991247, -6.695511796223322598 ) ) ;
#3123 = EDGE_CURVE ( 'NONE', #21007, #20921, #20037, .T. ) ;
#3124 = CARTESIAN_POINT ( 'NONE',  ( -82.24286370861491946, 12.41698901658174137, 15.97557204291290134 ) ) ;
#3125 = CARTESIAN_POINT ( 'NONE',  ( -40.07203023092246497, -11.15662918578760632, -34.25109662816847589 ) ) ;
#3126 = CARTESIAN_POINT ( 'NONE',  ( 163.1118516004056573, 19.27778845538753316, 19.27778845538783870 ) ) ;
#3127 = CARTESIAN_POINT ( 'NONE',  ( -93.01806789315402568, 20.64606681690898782, 8.551880885224901974 ) ) ;
#3128 = CARTESIAN_POINT ( 'NONE',  ( 170.2234770963711128, -39.99999999999982947, -15.44714144992858529 ) ) ;
#3129 = CYLINDRICAL_SURFACE ( 'NONE', #16804, 6.000000000000019540 ) ;
#3130 = CARTESIAN_POINT ( 'NONE',  ( 19.06497207195982924, -54.19242893257843008, -40.00000000000002132 ) ) ;
#3131 = CARTESIAN_POINT ( 'NONE',  ( 163.1118516004056573, -9.006482792069636645, 9.006482792069567367 ) ) ;
#3132 = B_SPLINE_CURVE_WITH_KNOTS ( 'NONE', 3,
 ( #11253, #9647, #7634, #20030, #7906, #20159, #9911, #18285, #15883, #10316, #18017, #16025, #4211, #10181, #18422, #10048, #16297, #7768, #24295, #5789, #22434, #1940, #18154, #71, #1808, #26166, #12301, #200, #11907, #8307, #22298, #20428, #6185, #22167, #14165, #2074, #24009, #21886, #1675, #26301, #4074, #24150, #26031, #6313, #5927, #3942, #14034, #13896, #8044, #12039, #22030, #16432, #19890, #16160, #3663, #6063, #3803, #12176, #20297, #9780, #2207, #8180, #24421, #24558, #14300, #11771, #17882, #8848, #338, #16828, #12844, #4868, #2875, #10983, #744, #12565, #14962, #16691, #21095, #4734, #20960, #2332, #10575, #8442, #2741, #19093, #12972, #16958, #873, #14433, #8713, #23097, #22562, #6577, #2603, #24824, #18690, #12433, #18559, #25096, #8982, #6843, #17089, #10845, #25221, #4341, #16561, #24690, #20561, #10445, #20699, #12701, #6446, #14696, #14562 ),
 .UNSPECIFIED., .F., .F.,
 ( 4, 2, 1, 2, 2, 2, 2, 2, 1, 2, 2, 2, 2, 2, 2, 1, 2, 2, 2, 2, 2, 1, 2, 2, 2, 2, 2, 2, 2, 2, 2, 2, 2, 2, 1, 2, 2, 2, 2, 2, 2, 2, 2, 2, 2, 2, 2, 1, 2, 2, 2, 2, 2, 1, 2, 2, 2, 2, 2, 2, 4 ),
 ( 0.000000000000000000, 0.01562500000000010061, 0.02343750000000014572, 0.02734375000000015613, 0.03125000000000015959, 0.04687500000000018041, 0.05468750000000021511, 0.06250000000000024980, 0.07031250000000029143, 0.07421875000000027756, 0.07812500000000027756, 0.09375000000000033307, 0.1015625000000003608, 0.1093750000000003886, 0.1250000000000004441, 0.1328125000000004718, 0.1367187500000004718, 0.1406250000000004718, 0.1562500000000004996, 0.1640625000000005274, 0.1718750000000005551, 0.1796875000000005829, 0.1835937500000006106, 0.1875000000000006106, 0.2031250000000007494, 0.2109375000000008049, 0.2187500000000008604, 0.2265625000000009159, 0.2343750000000009437, 0.2421875000000009992, 0.2500000000000010547, 0.2656250000000012768, 0.2734375000000013878, 0.2812500000000014988, 0.2890625000000015543, 0.2929687500000015543, 0.2968750000000015543, 0.3125000000000014988, 0.3203125000000014433, 0.3281250000000013878, 0.3359375000000013323, 0.3437500000000012768, 0.3515625000000012212, 0.3593750000000011657, 0.3671875000000011102, 0.3750000000000009992, 0.3906250000000009437, 0.3984375000000008882, 0.4023437500000008882, 0.4062500000000008327, 0.4218750000000006661, 0.4296875000000005551, 0.4375000000000004441, 0.4453125000000003886, 0.4492187500000003331, 0.4531250000000003331, 0.4609375000000002220, 0.4687500000000001665, 0.4765625000000001110, 0.4843750000000000555, 0.5000000000000000000 ),
 .UNSPECIFIED. ) ;
#3133 = CARTESIAN_POINT ( 'NONE',  ( -91.56559293963834989, -17.32597176626812185, -40.00000000000002132 ) ) ;
#3135 = CARTESIAN_POINT ( 'NONE',  ( -86.96347745069644475, 5.999880687339585546E-14, -21.75974354311649961 ) ) ;
#3134 = CARTESIAN_POINT ( 'NONE',  ( -3.971463587453694988, -43.02522237043177000, -23.46415232635092707 ) ) ;
#3136 = CARTESIAN_POINT ( 'NONE',  ( -91.56559293963834989, -22.67402823373193499, 0.000000000000000000 ) ) ;
#3137 = CARTESIAN_POINT ( 'NONE',  ( -135.8532207217289738, 21.81201906317767936, 21.81201906317778239 ) ) ;
#3138 = CARTESIAN_POINT ( 'NONE',  ( 163.1118516004056573, 12.73709011382477918, 40.00000000000002132 ) ) ;
#3139 = VERTEX_POINT ( 'NONE', #12045 ) ;
#3140 = CARTESIAN_POINT ( 'NONE',  ( 22.31419732600847539, -43.29699898481722187, 17.93420418956550222 ) ) ;
#3141 = DIRECTION ( 'NONE',  ( -0.01051738777840945799, 0.9307051272558533039, 0.3656191333259035670 ) ) ;
#3142 = EDGE_CURVE ( 'NONE', #22654, #26074, #22271, .T. ) ;
#3143 = CARTESIAN_POINT ( 'NONE',  ( 91.82158438592158234, -12.16597498400057198, 44.40256751092329779 ) ) ;
#3144 = CARTESIAN_POINT ( 'NONE',  ( -91.56559293963834989, 6.234561990864368500E-14, -22.67402823373191723 ) ) ;
#3145 = CARTESIAN_POINT ( 'NONE',  ( 200.0000000000000284, -82.49999999999991473, -52.49999999999977973 ) ) ;
#3146 = EDGE_CURVE ( 'NONE', #26122, #19577, #26173, .T. ) ;
#3147 = CARTESIAN_POINT ( 'NONE',  ( -77.90255099906865155, 8.644468104261473940, -20.04994828523921058 ) ) ;
#3148 = CARTESIAN_POINT ( 'NONE',  ( 199.9999999999999716, 1.225499021177249404, 18.97167928969624384 ) ) ;
#3149 = ADVANCED_FACE ( 'NONE', ( #9918 ), #11915, .F. ) ;
#3150 = CARTESIAN_POINT ( 'NONE',  ( -648.4009115869816924, 34.03803227582063329, -21.01344779086421255 ) ) ;
#3151 = EDGE_CURVE ( 'NONE', #1593, #6964, #20646, .T. ) ;
#3152 = DIRECTION ( 'NONE',  ( 0.000000000000000000, 1.000000000000000000, 0.000000000000000000 ) ) ;
#3153 = CARTESIAN_POINT ( 'NONE',  ( 163.1118516004056573, 9.006482792073693844, 47.56205970284970164 ) ) ;
#3154 = CARTESIAN_POINT ( 'NONE',  ( 200.0000000000000000, 42.42640687119310172, -14.14213562373052646 ) ) ;
#3155 = CARTESIAN_POINT ( 'NONE',  ( 200.0000000000000000, 14.14213562373083022, 42.42640687119289566 ) ) ;
#3156 = CARTESIAN_POINT ( 'NONE',  ( 19.06497207195980792, 10.03556273973447155, -10.03556273973422286 ) ) ;
#3157 = DIRECTION ( 'NONE',  ( 1.000000000000000000, -0.000000000000000000, -0.000000000000000000 ) ) ;
#3159 = CARTESIAN_POINT ( 'NONE',  ( 151.7948205124836534, -51.78348778862529400, -4.785054706299085581 ) ) ;
#3158 = CARTESIAN_POINT ( 'NONE',  ( 184.8905102610680444, 43.07788698682591644, -13.49065550809769221 ) ) ;
#3160 = CARTESIAN_POINT ( 'NONE',  ( -135.8532207217289738, 21.81201906317798134, -21.81201906317747685 ) ) ;
#3161 = CARTESIAN_POINT ( 'NONE',  ( 14.38125909742180752, 15.17850393972634038, -40.00000000000002132 ) ) ;
#3162 = FACE_BOUND ( 'NONE', #7335, .T. ) ;
#3163 =( BOUNDED_CURVE ( )  B_SPLINE_CURVE ( 3, ( #17693, #21446, #11326, #21832 ),
 .UNSPECIFIED., .F., .F. ) 
 B_SPLINE_CURVE_WITH_KNOTS ( ( 4, 4 ),
 ( 0.03952673792116803697, 0.04745072232834487980 ),
 .UNSPECIFIED. ) 
 CURVE ( )  GEOMETRIC_REPRESENTATION_ITEM ( )  RATIONAL_B_SPLINE_CURVE ( ( 0.5000000000000000000, 0.4999999999999885647, 0.5065943549827448544, 0.5197830649482689802 ) ) 
 REPRESENTATION_ITEM ( '' )  );
#3164 = CARTESIAN_POINT ( 'NONE',  ( -56.48582580120559271, 2.158176344243877536E-14, -9.153146818113587102 ) ) ;
#3165 = CARTESIAN_POINT ( 'NONE',  ( 4.995406935893297984, -39.06748935135205869, 17.50105314357158193 ) ) ;
#3166 = CARTESIAN_POINT ( 'NONE',  ( -188.8531444083254485, 43.29283928523322800, -17.93248118558230431 ) ) ;
#3167 = VERTEX_POINT ( 'NONE', #14039 ) ;
#3168 = CARTESIAN_POINT ( 'NONE',  ( -91.56559293963834989, 40.53558337403677569, -16.03295912088699993 ) ) ;
#3169 = CARTESIAN_POINT ( 'NONE',  ( 210.0000000000000284, 75.52305771588345351, -68.47933392563552957 ) ) ;
#3170 = CARTESIAN_POINT ( 'NONE',  ( 15.76057515043981638, 18.44716516375474313, 44.53539632574958063 ) ) ;
#3171 = CARTESIAN_POINT ( 'NONE',  ( -4.421177063219556835, -46.85829989839349707, -13.80119274858244793 ) ) ;
#3172 = EDGE_LOOP ( 'NONE', ( #6273, #9609 ) ) ;
#3173 = CARTESIAN_POINT ( 'NONE',  ( -166.7090608783924210, -37.06260950138378973, 15.35183551239266997 ) ) ;
#3174 = CARTESIAN_POINT ( 'NONE',  ( 199.9999999999999147, -4.475453068641236598, -18.46865746885900705 ) ) ;
#3175 = CARTESIAN_POINT ( 'NONE',  ( 23.30336656375548188, -23.35569295765331788, 42.87878279885809718 ) ) ;
#3176 = CARTESIAN_POINT ( 'NONE',  ( 98.29820294267324243, 7.653668647304287198, -18.47759065023114999 ) ) ;
#3177 = CARTESIAN_POINT ( 'NONE',  ( 199.0073806320087613, 3.093635517344801578, -19.75563546371214230 ) ) ;
#3178 = CARTESIAN_POINT ( 'NONE',  ( 130.1167162091013267, -29.33455044752969343, 12.15076864148434943 ) ) ;
#3179 = CARTESIAN_POINT ( 'NONE',  ( 57.59792236341147031, 39.99999999999990763, 37.56421063658199699 ) ) ;
#3180 = CARTESIAN_POINT ( 'NONE',  ( -370.0000000000001137, -4.857225732735059864E-14, 0.000000000000000000 ) ) ;
#3181 = CARTESIAN_POINT ( 'NONE',  ( -200.0000000000000000, -18.14877749763631343, -46.38610861938597907 ) ) ;
#3182 = CARTESIAN_POINT ( 'NONE',  ( -238.4067589809705510, -40.96449427998265946, -2.449293598294708485E-15 ) ) ;
#3184 = CARTESIAN_POINT ( 'NONE',  ( -598.2148974052754511, 39.08565501426862454, -8.517844816818030296 ) ) ;
#3183 = CARTESIAN_POINT ( 'NONE',  ( 23.58679727197023368, -13.78527791281898374, -46.73132340480074021 ) ) ;
#3185 = CARTESIAN_POINT ( 'NONE',  ( 184.8905102610680444, -19.07866798485554938, 40.00000000000002132 ) ) ;
#3186 = CARTESIAN_POINT ( 'NONE',  ( -213.1075012329537230, -9.698598906450557777, 9.698598906450415669 ) ) ;
#3187 = CARTESIAN_POINT ( 'NONE',  ( 91.82158438592156813, 40.00000000000027711, -22.79471317813428044 ) ) ;
#3188 = CARTESIAN_POINT ( 'NONE',  ( 192.4448373802101173, -39.99999999999977973, -19.99999999996102673 ) ) ;
#3189 = CARTESIAN_POINT ( 'NONE',  ( 125.5822694977128435, -28.05278406097506050, -11.61984362037969554 ) ) ;
#3190 = ORIENTED_EDGE ( 'NONE', *, *, #8835, .T. ) ;
#3192 = CARTESIAN_POINT ( 'NONE',  ( -3.615356597029523389, 43.25798660799116391, -17.91804473398302733 ) ) ;
#3191 = CARTESIAN_POINT ( 'NONE',  ( -215.0000000000000284, 66.50000000000001421, -66.50000000000005684 ) ) ;
#3193 = CARTESIAN_POINT ( 'NONE',  ( -238.4067589809705794, -0.9644942799826263791, 40.00000000000002132 ) ) ;
#3194 = FILL_AREA_STYLE ('',( #23544 ) ) ;
#3195 = CARTESIAN_POINT ( 'NONE',  ( -191.2489946134048182, 43.85245824700246686, -18.16428294930772580 ) ) ;
#3196 = VERTEX_POINT ( 'NONE', #20835 ) ;
#3197 = EDGE_LOOP ( 'NONE', ( #8537, #5709, #360, #14901, #14125, #8295, #1175 ) ) ;
#3198 = CARTESIAN_POINT ( 'NONE',  ( 130.8568914410475372, 24.07718906447243867, -24.07718906447216156 ) ) ;
#3199 = CARTESIAN_POINT ( 'NONE',  ( 90.71510531243710318, -21.27078368575422118, -8.810647086396985017 ) ) ;
#3200 = ORIENTED_EDGE ( 'NONE', *, *, #9955, .T. ) ;
#3201 = VERTEX_POINT ( 'NONE', #22834 ) ;
#3202 = CARTESIAN_POINT ( 'NONE',  ( 199.0263771353516233, -14.14574067859894413, 14.14574067859863682 ) ) ;
#3203 = CIRCLE ( 'NONE', #231, 5.000000000000039080 ) ;
#3204 = VECTOR ( 'NONE', #2442, 1000.000000000000000 ) ;
#3205 = CARTESIAN_POINT ( 'NONE',  ( -163.5815439468655939, 18.59457101073966712, -35.61501074489178365 ) ) ;
#3206 = CARTESIAN_POINT ( 'NONE',  ( -135.8532207217289738, 50.09629031063965243, -6.472252184284084109 ) ) ;
#3207 = CARTESIAN_POINT ( 'NONE',  ( -129.2303573025683079, -24.84170326008768370, -11.67678754045152800 ) ) ;
#3208 = CARTESIAN_POINT ( 'NONE',  ( -280.0000000000000568, -40.00000000000000000, -20.00000000000015277 ) ) ;
#3209 = CARTESIAN_POINT ( 'NONE',  ( -351.0000000000000568, -4.857225732735059864E-14, 0.000000000000000000 ) ) ;
#3210 = DIRECTION ( 'NONE',  ( 1.000000000000000000, 1.836970198721030181E-16, 0.000000000000000000 ) ) ;
#3211 = EDGE_CURVE ( 'NONE', #7311, #5206, #7063, .T. ) ;
#3212 = CARTESIAN_POINT ( 'NONE',  ( 170.2234770963711128, -40.00000000000024158, 24.55285855007145202 ) ) ;
#3213 = CARTESIAN_POINT ( 'NONE',  ( 192.4448373802100889, -20.00000000003938538, 0.000000000000000000 ) ) ;
#3214 = CARTESIAN_POINT ( 'NONE',  ( 91.82158438592158234, 2.580785920671402147E-13, -22.79471317813470321 ) ) ;
#3215 = DIRECTION ( 'NONE',  ( 0.3301743753966839834, 0.000000000000000000, -0.9439199552035171248 ) ) ;
#3216 = CARTESIAN_POINT ( 'NONE',  ( -208.1127848780264742, -38.89260858015728672, -17.67593391476669851 ) ) ;
#3217 = CARTESIAN_POINT ( 'NONE',  ( 192.4448373802100889, 1.051811698935164031E-13, -20.00000000003942091 ) ) ;
#3218 = CARTESIAN_POINT ( 'NONE',  ( -199.0731274800458834, 18.57195892579281704, 44.83667511838283559 ) ) ;
#3219 = CARTESIAN_POINT ( 'NONE',  ( 121.8740240556053323, 26.81399039734613865, 11.10671848392282079 ) ) ;
#3220 = CARTESIAN_POINT ( 'NONE',  ( -77.72892396114366420, 19.09609284692255571, -10.88898768916570603 ) ) ;
#3221 = CARTESIAN_POINT ( 'NONE',  ( -91.56559293963836410, 16.03295912088714203, -16.03295912088699282 ) ) ;
#3222 = CARTESIAN_POINT ( 'NONE',  ( -87.10570614285154534, -13.14378919784947364, 16.99508527299667193 ) ) ;
#3223 = CARTESIAN_POINT ( 'NONE',  ( -91.56559293963834989, -44.31723036834903695, 12.25131212657476709 ) ) ;
#3224 = AXIS2_PLACEMENT_3D ( 'NONE', #4997, #18960, #3120 ) ;
#3225 = AXIS2_PLACEMENT_3D ( 'NONE', #18624, #4927, #14497 ) ;
#3226 = CARTESIAN_POINT ( 'NONE',  ( -91.56559293963836410, -12.25131212657524138, 44.31723036834888774 ) ) ;
#3227 = CARTESIAN_POINT ( 'NONE',  ( -151.4802930569921955, -16.17241674341475033, -31.86309827676130624 ) ) ;
#3228 = DIRECTION ( 'NONE',  ( -1.000000000000000000, 0.000000000000000000, 0.000000000000000000 ) ) ;
#3229 = EDGE_LOOP ( 'NONE', ( #13277, #22786, #5608, #7278, #3262, #6501 ) ) ;
#3230 = CARTESIAN_POINT ( 'NONE',  ( -91.56559293963834989, 12.25131212657497848, -12.25131212657469426 ) ) ;
#3231 = CARTESIAN_POINT ( 'NONE',  ( 180.0000000000000000, -66.50000000000001421, 66.50000000000005684 ) ) ;
#3232 = CARTESIAN_POINT ( 'NONE',  ( -16.41654234116891686, 12.95560590050290806, -42.70586891546086861 ) ) ;
#3233 = EDGE_LOOP ( 'NONE', ( #18372, #13913, #1559, #22423 ) ) ;
#3234 = CARTESIAN_POINT ( 'NONE',  ( 163.1118516004056573, -40.00000000000027711, 27.26290988616830546 ) ) ;
#3235 = CARTESIAN_POINT ( 'NONE',  ( 199.0255658961882830, -18.53135165341859292, 7.535237739358464637 ) ) ;
#3236 = DIRECTION ( 'NONE',  ( -1.000000000000000000, -1.836970198721030181E-16, 0.000000000000000000 ) ) ;
#3237 = CIRCLE ( 'NONE', #18086, 19.53474504356812602 ) ;
#3238 = ORIENTED_EDGE ( 'NONE', *, *, #25270, .F. ) ;
#3239 = VERTEX_POINT ( 'NONE', #4611 ) ;
#3240 = CARTESIAN_POINT ( 'NONE',  ( 57.59792236341147031, 1.722363176415065089, -1.722363176415036445 ) ) ;
#3241 = CARTESIAN_POINT ( 'NONE',  ( -280.0000000000000568, 40.00000000000004263, -19.99999999999987210 ) ) ;
#3242 = DIRECTION ( 'NONE',  ( 1.000000000000000000, 1.836970198721030427E-16, -0.000000000000000000 ) ) ;
#3243 = CLOSED_SHELL ( 'NONE', ( #11757, #22727, #20867, #12476, #10434, #24263, #18492, #1529, #17565, #25370, #17208, #15951, #19396, #10881, #11280, #23525, #18081, #23913, #20057, #3963, #2165, #20870, #12486, #18771, #24445, #5556, #12232, #14264, #14679, #12482, #25042, #20355, #2970, #9287, #20548, #2172, #2987, #2751, #2340, #16882, #17246, #24951, #21636, #15474, #13245, #14824, #11974, #22263, #19247, #1045, #5863, #291, #2482, #7282, #5025, #6375, #9946, #4875, #5328, #14432, #8067, #4219, #9376, #10598, #17893, #12575, #9237, #14345, #24209, #24635, #22975 ) ) ;
#3244 = DIRECTION ( 'NONE',  ( 0.000000000000000000, 0.000000000000000000, -1.000000000000000000 ) ) ;
#3245 = CARTESIAN_POINT ( 'NONE',  ( -100.7734535825088500, -39.99999999999995737, -22.67402823373205578 ) ) ;
#3246 = CARTESIAN_POINT ( 'NONE',  ( 200.0000000000001137, -7.564955314186367907, -17.43543124971759539 ) ) ;
#3247 = DIRECTION ( 'NONE',  ( 0.000000000000000000, 1.000000000000000000, 0.000000000000000000 ) ) ;
#3248 = CARTESIAN_POINT ( 'NONE',  ( 146.6084372240433993, -24.48358557860353457, 24.48358557860296258 ) ) ;
#3249 = CARTESIAN_POINT ( 'NONE',  ( 130.8568914410475088, 24.07718906446937623, -32.49135343045455215 ) ) ;
#3250 = CARTESIAN_POINT ( 'NONE',  ( -77.56366795221720167, -22.09173432935364190, 1.395416561028956393 ) ) ;
#3251 = CARTESIAN_POINT ( 'NONE',  ( 91.82158438592158234, 2.580785920671402147E-13, -22.79471317813470321 ) ) ;
#3252 = CARTESIAN_POINT ( 'NONE',  ( -105.2054292635177006, -21.49321519473982889, -1.366713675288041330 ) ) ;
#3253 = CARTESIAN_POINT ( 'NONE',  ( -213.1075012329537230, -13.71589010951915810, 0.000000000000000000 ) ) ;
#3254 = CARTESIAN_POINT ( 'NONE',  ( 130.8568914410475088, -5.949712681206664300, -40.00000000000002132 ) ) ;
#3255 = CARTESIAN_POINT ( 'NONE',  ( 130.8568914410475088, 52.36146031193420924, 4.207082182989907437 ) ) ;
#3256 = CARTESIAN_POINT ( 'NONE',  ( -91.56559293963836410, 22.67402823373190301, -40.00000000000002132 ) ) ;
#3258 = CARTESIAN_POINT ( 'NONE',  ( -716.9846540392142060, -82.49999999999991473, 52.49999999999977263 ) ) ;
#3257 = CARTESIAN_POINT ( 'NONE',  ( -105.2054292635175585, -2.444554031225951202E-13, 21.49321519473985020 ) ) ;
#3259 = FACE_OUTER_BOUND ( 'NONE', #17549, .T. ) ;
#3260 = CARTESIAN_POINT ( 'NONE',  ( 91.82158438592158234, 16.11829626346139577, 16.11829626346143840 ) ) ;
#3261 = CARTESIAN_POINT ( 'NONE',  ( 170.2234770963711128, 15.44714144992818738, 40.00000000000002132 ) ) ;
#3262 = ORIENTED_EDGE ( 'NONE', *, *, #9386, .F. ) ;
#3263 = CARTESIAN_POINT ( 'NONE',  ( 27.00968939605193953, -41.97305875717999157, 17.38581019152067597 ) ) ;
#3264 = B_SPLINE_CURVE_WITH_KNOTS ( 'NONE', 3,
 ( #15275, #15520, #25925, #17916, #5430, #7666, #15778, #7159, #5181, #3178, #26201, #16462, #16191, #13925, #22196, #11935, #6217, #14462, #24584, #2233, #3833, #14064, #4104, #22328, #99, #18181, #18316, #12204, #20062, #18048, #22593, #20187, #227, #8341 ),
 .UNSPECIFIED., .F., .F.,
 ( 4, 2, 2, 2, 2, 2, 2, 2, 2, 2, 2, 2, 2, 2, 2, 2, 4 ),
 ( -5.298243351207237208E-05, 0.01887868273877487887, 0.02834451532491835332, 0.03071097347145420459, 0.03307743161799005932, 0.03544388976452591405, 0.03781034791106176185, 0.04254326420413346438, 0.04727618049720517385, 0.04964263864374102164, 0.05200909679027687638, 0.05674201308334866217, 0.05910847122988456548, 0.06029170030315254142, 0.06147492937642052430, 0.06620784566949247663, 0.07567367825563638128 ),
 .UNSPECIFIED. ) ;
#3265 =( BOUNDED_SURFACE ( )  B_SPLINE_SURFACE ( 3, 2, ( 
 ( #3095, #842, #15060 ),
 ( #11076, #15314, #25447 ),
 ( #4969, #7199, #11321 ),
 ( #19437, #1224, #9583 ),
 ( #7449, #7975, #14104 ),
 ( #19563, #15818, #20099 ),
 ( #3340, #9849, #17688 ),
 ( #15563, #11704, #7576 ),
 ( #25967, #7707, #9980 ),
 ( #1355, #11441, #9454 ),
 ( #11570, #19689, #19825 ),
 ( #3734, #1741, #23813 ),
 ( #25831, #23688, #26240 ),
 ( #17560, #3873, #23945 ),
 ( #1611, #5723, #13701 ),
 ( #18089, #25698, #5466 ) ),
 .UNSPECIFIED., .F., .F., .F. ) 
 B_SPLINE_SURFACE_WITH_KNOTS ( ( 4, 2, 2, 2, 2, 2, 2, 4 ),
 ( 3, 3 ),
 ( 0.04143342415526168887, 0.04844520228007725970, 0.05195109134248504512, 0.05545698040489283054, 0.06246875852970840137, 0.06422170306091229408, 0.06597464759211618679, 0.06948053665452397221 ),
 ( 0.000000000000000000, 1.000000000000000000 ),
 .UNSPECIFIED. ) 
 GEOMETRIC_REPRESENTATION_ITEM ( )  RATIONAL_B_SPLINE_SURFACE ( (
 ( 1.000000000000000000, 0.9541700777564554592, 1.000000000000000000),
 ( 1.000000000000000000, 0.9520170179160407642, 1.000000000000000000),
 ( 1.000000000000000000, 0.9503264940267092120, 1.000000000000000000),
 ( 1.000000000000000000, 0.9485966650357087193, 1.000000000000000000),
 ( 1.000000000000000000, 0.9481601953989508003, 1.000000000000000000),
 ( 1.000000000000000000, 0.9475786562869455976, 1.000000000000000000),
 ( 1.000000000000000000, 0.9474333041665753408, 1.000000000000000000),
 ( 1.000000000000000000, 0.9474385324112287732, 1.000000000000000000),
 ( 1.000000000000000000, 0.9480205960586695069, 1.000000000000000000),
 ( 1.000000000000000000, 0.9494433550395400268, 1.000000000000000000),
 ( 1.000000000000000000, 0.9497628485351724548, 1.000000000000000000),
 ( 1.000000000000000000, 0.9504717112746540186, 1.000000000000000000),
 ( 1.000000000000000000, 0.9508623530685325065, 1.000000000000000000),
 ( 1.000000000000000000, 0.9521262215761925329, 1.000000000000000000),
 ( 1.000000000000000000, 0.9530922057189646912, 1.000000000000000000),
 ( 1.000000000000000000, 0.9541700777564678937, 1.000000000000000000) ) ) 
 REPRESENTATION_ITEM ( '' )  SURFACE ( )  );
#3266 = EDGE_CURVE ( 'NONE', #24713, #12692, #16837, .T. ) ;
#3267 = PLANE ( 'NONE',  #7250 ) ;
#3268 = AXIS2_PLACEMENT_3D ( 'NONE', #24504, #16507, #2541 ) ;
#3269 = CARTESIAN_POINT ( 'NONE',  ( 184.8905102610680444, -43.07788698682576722, 13.49065550809799063 ) ) ;
#3270 = CARTESIAN_POINT ( 'NONE',  ( -190.0000000000000000, 61.50000000000009948, -66.50000000000005684 ) ) ;
#3271 = CARTESIAN_POINT ( 'NONE',  ( 190.0000000000000000, -71.50000000000002842, 66.50000000000005684 ) ) ;
#3272 = CIRCLE ( 'NONE', #18137, 5.000000000000004441 ) ;
#3273 = CARTESIAN_POINT ( 'NONE',  ( -47.45115950045327224, 14.84795788661607929, -29.80449331798435608 ) ) ;
#3274 = CARTESIAN_POINT ( 'NONE',  ( 199.9999999999999716, 8.673909288817675645, 16.91296503504769078 ) ) ;
#3275 = CARTESIAN_POINT ( 'NONE',  ( -654.7090520960496178, 38.32262798275520055, -11.47173633207906107 ) ) ;
#3276 = CARTESIAN_POINT ( 'NONE',  ( -82.27051431266434633, -5.326770061496585384, -19.46826128364778086 ) ) ;
#3277 = CARTESIAN_POINT ( 'NONE',  ( 19.06497207195980792, 10.03556273973447155, -10.03556273973422286 ) ) ;
#3278 = CARTESIAN_POINT ( 'NONE',  ( 130.8568914410475088, 52.36146031193427319, -4.207082182989173802 ) ) ;
#3279 = CARTESIAN_POINT ( 'NONE',  ( -110.0954903719524935, 20.05999989284160634, -2.400669240794628401 ) ) ;
#3280 = CARTESIAN_POINT ( 'NONE',  ( 14.38125909742180752, 10.73282306404735387, -10.73282306404708919 ) ) ;
#3281 = CARTESIAN_POINT ( 'NONE',  ( 14.38125909742182529, -39.01709431150879936, -39.01709431150948859 ) ) ;
#3283 = CARTESIAN_POINT ( 'NONE',  ( 4.995406935893297984, 10.78321810390233892, -67.35176059882522281 ) ) ;
#3282 = CARTESIAN_POINT ( 'NONE',  ( -192.9588430854689705, -38.51493924976909966, -38.51493924976973915 ) ) ;
#3284 = CARTESIAN_POINT ( 'NONE',  ( -30.26275506840325136, 57.76657404653985139, -1.198031551615314161 ) ) ;
#3285 = CARTESIAN_POINT ( 'NONE',  ( -213.1075012329537230, -9.698598906450557777, 9.698598906450415669 ) ) ;
#3286 = PLANE ( 'NONE',  #16622 ) ;
#3287 = EDGE_CURVE ( 'NONE', #26074, #19299, #4849, .T. ) ;
#3288 = CARTESIAN_POINT ( 'NONE',  ( 14.38125909742181108, -5.035366881890652543E-14, 15.17850393972633682 ) ) ;
#3289 = CARTESIAN_POINT ( 'NONE',  ( 200.0000000000000000, -14.14213562373122457, 42.42640687119282461 ) ) ;
#3290 = ADVANCED_FACE ( 'NONE', ( #17095 ), #16203, .T. ) ;
#3291 = CARTESIAN_POINT ( 'NONE',  ( 170.2234770963711128, 15.44714144992818738, 40.00000000000002132 ) ) ;
#3292 = VERTEX_POINT ( 'NONE', #6692 ) ;
#3293 = CARTESIAN_POINT ( 'NONE',  ( 91.82158438592158234, 16.11829626348434630, -40.45024623143955012 ) ) ;
#3294 = CARTESIAN_POINT ( 'NONE',  ( -103.9474983245022344, -20.15710290851514586, -8.027156558344424653 ) ) ;
#3295 = CARTESIAN_POINT ( 'NONE',  ( 25.62979979007943498, 13.63460241475089951, 45.99287499157590275 ) ) ;
#3296 = CARTESIAN_POINT ( 'NONE',  ( -77.90255099906873681, -20.04994828523928163, -8.644468104261223473 ) ) ;
#3297 = EDGE_CURVE ( 'NONE', #12216, #8800, #5759, .T. ) ;
#3298 = EDGE_CURVE ( 'NONE', #4428, #12165, #2827, .T. ) ;
#3299 = ORIENTED_EDGE ( 'NONE', *, *, #25921, .F. ) ;
#3300 = CARTESIAN_POINT ( 'NONE',  ( -188.2956751479426885, -46.98904240251139441, 13.82790121914922388 ) ) ;
#3301 = CARTESIAN_POINT ( 'NONE',  ( 199.9999999999998579, -2.482523633563583410, -18.84177167654976515 ) ) ;
#3302 = CARTESIAN_POINT ( 'NONE',  ( 22.95085416411796331, -17.86294511971716048, 43.12496437194802468 ) ) ;
#3303 = CARTESIAN_POINT ( 'NONE',  ( 37.37129771754243279, 20.48130208294292842, -38.51719860168416432 ) ) ;
#3304 = CARTESIAN_POINT ( 'NONE',  ( 199.0057363775755448, 17.49143510765091492, -9.692886659233986180 ) ) ;
#3305 = CARTESIAN_POINT ( 'NONE',  ( 190.0000000000001137, 3.490243377569959927E-14, 0.000000000000000000 ) ) ;
#3306 = CARTESIAN_POINT ( 'NONE',  ( -162.0762913951021176, 39.99999999999998579, 1.694272876828463614 ) ) ;
#3307 = CARTESIAN_POINT ( 'NONE',  ( -87.11181979037108647, -2.713702011544433912, 21.35018875643972081 ) ) ;
#3308 =( BOUNDED_SURFACE ( )  B_SPLINE_SURFACE ( 3, 2, ( 
 ( #17755, #18020, #13900 ),
 ( #11633, #13634, #19756 ),
 ( #13505, #23880, #11377 ),
 ( #3806, #1811, #7637 ),
 ( #5792, #3279, #5657 ),
 ( #13763, #19498, #9391 ),
 ( #25638, #15495, #23625 ),
 ( #5405, #21628, #3404 ),
 ( #11505, #19630, #6449 ),
 ( #20162, #26304, #10578 ),
 ( #14436, #2335, #20300 ),
 ( #12179, #12304, #8183 ),
 ( #12042, #1944, #10051 ),
 ( #4344, #20564, #18693 ),
 ( #3945, #6190, #24694 ),
 ( #18158, #6316, #8047 ) ),
 .UNSPECIFIED., .F., .F., .F. ) 
 B_SPLINE_SURFACE_WITH_KNOTS ( ( 4, 2, 2, 2, 2, 2, 2, 4 ),
 ( 3, 3 ),
 ( 0.04143342415524681882, 0.04862317170365706986, 0.05221804547786219192, 0.05401548236496475641, 0.05581291925206731397, 0.06300266680047755807, 0.06659754057468268706, 0.07019241434888781606 ),
 ( 0.000000000000000000, 1.000000000000000000 ),
 .UNSPECIFIED. ) 
 GEOMETRIC_REPRESENTATION_ITEM ( )  RATIONAL_B_SPLINE_SURFACE ( (
 ( 1.000000000000000000, 0.9541700777564458003, 1.000000000000000000),
 ( 1.000000000000000000, 0.9519624585090378233, 1.000000000000000000),
 ( 1.000000000000000000, 0.9502408728421397610, 1.000000000000000000),
 ( 1.000000000000000000, 0.9485093239120891973, 1.000000000000000000),
 ( 1.000000000000000000, 0.9480808157489741816, 1.000000000000000000),
 ( 1.000000000000000000, 0.9476673512789849374, 1.000000000000000000),
 ( 1.000000000000000000, 0.9475676663659571286, 1.000000000000000000),
 ( 1.000000000000000000, 0.9474462208978693400, 1.000000000000000000),
 ( 1.000000000000000000, 0.9474241303505198664, 1.000000000000000000),
 ( 1.000000000000000000, 0.9475034751962024826, 1.000000000000000000),
 ( 1.000000000000000000, 0.9481710333135665580, 1.000000000000000000),
 ( 1.000000000000000000, 0.9500557947230517941, 1.000000000000000000),
 ( 1.000000000000000000, 0.9508368636698915077, 1.000000000000000000),
 ( 1.000000000000000000, 0.9526500836528452032, 1.000000000000000000),
 ( 1.000000000000000000, 0.9536844903836366738, 1.000000000000000000),
 ( 1.000000000000000000, 0.9548353292492207656, 1.000000000000000000) ) ) 
 REPRESENTATION_ITEM ( '' )  SURFACE ( )  );
#3309 = CARTESIAN_POINT ( 'NONE',  ( 18.89824444022306338, 48.20791849611975266, -14.00990882958417671 ) ) ;
#3310 = CARTESIAN_POINT ( 'NONE',  ( -162.0762913951020607, -41.69427287692683848, 40.00000000000002132 ) ) ;
#3312 = CARTESIAN_POINT ( 'NONE',  ( -614.8060072283433328, 29.12309729869464192, -27.42103544326355546 ) ) ;
#3311 = CARTESIAN_POINT ( 'NONE',  ( 37.15749683987841223, -12.76981037570312694, -41.79699086507935135 ) ) ;
#3313 = CARTESIAN_POINT ( 'NONE',  ( -30.26275506840324425, -1.694272468446265334, 40.00000000000002132 ) ) ;
#3314 = CARTESIAN_POINT ( 'NONE',  ( -135.8532207217289738, 9.153146818113546246, -0.000000000000000000 ) ) ;
#3315 = CARTESIAN_POINT ( 'NONE',  ( 170.2234770963711128, -2.259079968736224833E-13, 24.55285855007187124 ) ) ;
#3316 = CARTESIAN_POINT ( 'NONE',  ( 200.0000000000000000, -39.99999999999977973, -20.00000000000034817 ) ) ;
#3317 = CARTESIAN_POINT ( 'NONE',  ( 99.57966121244446356, -18.94872250966755090, -7.848817853148193358 ) ) ;
#3318 = ORIENTED_EDGE ( 'NONE', *, *, #9230, .T. ) ;
#3320 = CARTESIAN_POINT ( 'NONE',  ( 6.011245401515337150, 44.78331514753590881, -18.54985650214099380 ) ) ;
#3319 = PLANE ( 'NONE',  #14956 ) ;
#3321 = CARTESIAN_POINT ( 'NONE',  ( 130.8568914410475372, -5.949712681206667853, -2.449293598294708485E-15 ) ) ;
#3322 = SURFACE_SIDE_STYLE ('',( #13302 ) ) ;
#3323 = CARTESIAN_POINT ( 'NONE',  ( -189.0115211946964848, 43.33403054566065293, -17.94954316430204955 ) ) ;
#3324 = CARTESIAN_POINT ( 'NONE',  ( 0.000000000000000000, 0.000000000000000000, 0.000000000000000000 ) ) ;
#3325 = ORIENTED_EDGE ( 'NONE', *, *, #11896, .T. ) ;
#3326 = ORIENTED_EDGE ( 'NONE', *, *, #14182, .T. ) ;
#3327 = CARTESIAN_POINT ( 'NONE',  ( 163.1118516004056573, 19.27778845538780317, -19.27778845538757224 ) ) ;
#3328 = CARTESIAN_POINT ( 'NONE',  ( -678.9461782662772293, 75.00000000000000000, 30.00000000000158096 ) ) ;
#3329 = EDGE_LOOP ( 'NONE', ( #14913, #4122, #9477, #25461 ) ) ;
#3330 = ORIENTED_EDGE ( 'NONE', *, *, #18880, .T. ) ;
#3331 = CARTESIAN_POINT ( 'NONE',  ( 199.0262110011730954, -16.45735938206000171, 11.37817034370231006 ) ) ;
#3332 = CARTESIAN_POINT ( 'NONE',  ( -210.0000000000000284, 60.27431767988564104, -73.32453023895048716 ) ) ;
#3333 = CARTESIAN_POINT ( 'NONE',  ( -213.1075012329537230, 66.26714140136188291, 9.698598906438215650 ) ) ;
#3334 = CARTESIAN_POINT ( 'NONE',  ( -105.2054292635174733, -1.371496932086386566, -21.49321519473988573 ) ) ;
#3335 = CARTESIAN_POINT ( 'NONE',  ( 170.2234770963711128, 1.169953928977015745E-13, -24.55285855007187124 ) ) ;
#3336 = CARTESIAN_POINT ( 'NONE',  ( -105.3841224671147216, -9.645501175099258973, -19.11844758208756545 ) ) ;
#3337 = CARTESIAN_POINT ( 'NONE',  ( -210.0000000000000284, 0.000000000000000000, -75.00000000000000000 ) ) ;
#3338 = CARTESIAN_POINT ( 'NONE',  ( 184.8905102610680444, -39.99999999999978684, -19.07866798485600768 ) ) ;
#3339 = CARTESIAN_POINT ( 'NONE',  ( 91.82158438592156813, 40.00000000000027711, -22.79471317813428044 ) ) ;
#3340 = CARTESIAN_POINT ( 'NONE',  ( -114.7827252410686754, -16.13252424103086824, 15.16659028666128073 ) ) ;
#3341 = CARTESIAN_POINT ( 'NONE',  ( -213.1075012329537230, -37.98287015391232302, -18.58567234101164800 ) ) ;
#3342 = CARTESIAN_POINT ( 'NONE',  ( 91.82158438592158234, 7.693928927950222250E-14, -17.20528682183300262 ) ) ;
#3343 = CARTESIAN_POINT ( 'NONE',  ( 136.1360204305621266, 24.77266263493138965, -24.77266263493110188 ) ) ;
#3344 = CARTESIAN_POINT ( 'NONE',  ( 149.5797498300189261, 29.41965740490872250, 12.18602109748340290 ) ) ;
#3345 = AXIS2_PLACEMENT_3D ( 'NONE', #7445, #17435, #11438 ) ;
#3346 = CARTESIAN_POINT ( 'NONE',  ( -77.65678946166460150, 18.42186864996805440, -12.10857941959429596 ) ) ;
#3347 = CARTESIAN_POINT ( 'NONE',  ( 130.8568914410475372, 24.07718906447243867, -24.07718906447216156 ) ) ;
#3348 = CARTESIAN_POINT ( 'NONE',  ( 19.06497207195981147, -4.605042221739098431E-14, 14.19242893257840521 ) ) ;
#3349 = CARTESIAN_POINT ( 'NONE',  ( 170.2234770963711128, -45.64576402573183600, 10.92277846919191653 ) ) ;
#3350 = CARTESIAN_POINT ( 'NONE',  ( 91.82158438592159655, -16.11829626346125011, -16.11829626346154853 ) ) ;
#3351 = CARTESIAN_POINT ( 'NONE',  ( -121.8425463773527326, -9.420908034907393258, -22.74408395655231274 ) ) ;
#3352 = ORIENTED_EDGE ( 'NONE', *, *, #17746, .F. ) ;
#3353 = CARTESIAN_POINT ( 'NONE',  ( 57.59792236341147031, -1.722363176414363206, -54.84617931850881689 ) ) ;
#3354 = DIRECTION ( 'NONE',  ( 0.000000000000000000, 0.000000000000000000, 1.000000000000000000 ) ) ;
#3355 = CARTESIAN_POINT ( 'NONE',  ( 200.0000000000000000, -13.44239485489230290, 13.44239485489200803 ) ) ;
#3356 = EDGE_LOOP ( 'NONE', ( #20075, #16422, #24649, #24167 ) ) ;
#3357 = CARTESIAN_POINT ( 'NONE',  ( -192.9588430854689989, 1.161019517985663313E-13, -14.46834944099969533 ) ) ;
#3358 = CARTESIAN_POINT ( 'NONE',  ( 199.0193679503813939, -17.97530889761664596, -8.776769756081623797 ) ) ;
#3359 = CARTESIAN_POINT ( 'NONE',  ( -62.79433447051992090, 11.74096317487346042, 24.94280497462943558 ) ) ;
#3360 = VERTEX_POINT ( 'NONE', #14942 ) ;
#3361 = ORIENTED_EDGE ( 'NONE', *, *, #5308, .F. ) ;
#3362 = CARTESIAN_POINT ( 'NONE',  ( -192.9370379452147972, -48.35015161802368056, -14.03127537977354855 ) ) ;
#3363 = EDGE_CURVE ( 'NONE', #5576, #6112, #18528, .T. ) ;
#3364 = CARTESIAN_POINT ( 'NONE',  ( 136.1360204305621551, 40.00000000000002842, 4.966164525587208445 ) ) ;
#3365 = DIRECTION ( 'NONE',  ( 1.000000000000000000, 0.000000000000000000, 0.000000000000000000 ) ) ;
#3366 = VECTOR ( 'NONE', #1579, 1000.000000000000114 ) ;
#3367 = CARTESIAN_POINT ( 'NONE',  ( -190.0000000000000000, -74.99999999999995737, 0.000000000000000000 ) ) ;
#3368 = CARTESIAN_POINT ( 'NONE',  ( -30.26275506840323359, -40.00000000000017053, 41.69427246844613677 ) ) ;
#3369 = CARTESIAN_POINT ( 'NONE',  ( 199.9999999999998863, -11.82502131081330887, -14.88093782183822888 ) ) ;
#3370 = CARTESIAN_POINT ( 'NONE',  ( -30.26275506840325136, 40.00000000000001421, 1.694272468446399227 ) ) ;
#3372 = EDGE_CURVE ( 'NONE', #12121, #6926, #20388, .T. ) ;
#3371 = B_SPLINE_CURVE_WITH_KNOTS ( 'NONE', 3,
 ( #315, #18533, #4188, #4444, #22540, #8416, #6039, #44, #20138, #12537, #7882, #12410, #24129, #20409 ),
 .UNSPECIFIED., .F., .F.,
 ( 4, 2, 2, 2, 2, 2, 4 ),
 ( 6.938893903907228378E-18, 0.002941681445496991537, 0.004412522168245485571, 0.005883362890993980472, 0.008825044336490969407, 0.01029588505923945650, 0.01176672578198794533 ),
 .UNSPECIFIED. ) ;
#3373 = DIRECTION ( 'NONE',  ( 1.000000000000000000, -1.836970198721030181E-16, 0.000000000000000000 ) ) ;
#3374 = CARTESIAN_POINT ( 'NONE',  ( -7.233308327731263532, -17.51119053152957150, -42.27575367454436872 ) ) ;
#3375 = CARTESIAN_POINT ( 'NONE',  ( 163.1118516004056573, 47.56205970284970164, -9.006482792073828847 ) ) ;
#3376 = DIRECTION ( 'NONE',  ( -1.357111460130038308E-16, 0.7387770694782700431, -0.6739498806388346530 ) ) ;
#3377 = CARTESIAN_POINT ( 'NONE',  ( 184.8905102610680444, 40.00000000000025580, -19.07866798485515503 ) ) ;
#3378 = DIRECTION ( 'NONE',  ( -1.000000000000000000, 0.000000000000000000, 0.000000000000000000 ) ) ;
#3379 = CARTESIAN_POINT ( 'NONE',  ( 0.2972598230769983307, -14.33493731733933352, 40.00000000000002132 ) ) ;
#3380 = CARTESIAN_POINT ( 'NONE',  ( -100.7734535825088500, 22.67402823373189946, -40.00000000000002132 ) ) ;
#3381 = EDGE_CURVE ( 'NONE', #8098, #817, #24818, .T. ) ;
#3382 = CARTESIAN_POINT ( 'NONE',  ( -100.7734535825088500, 16.03295912088713848, -16.03295912088698927 ) ) ;
#3383 = CARTESIAN_POINT ( 'NONE',  ( 0.2972598230769983307, -14.33493731733933352, -40.00000000000002132 ) ) ;
#3385 = CARTESIAN_POINT ( 'NONE',  ( -86.84962968273566730, 19.67999904273991163, 8.151722510992470916 ) ) ;
#3384 = CARTESIAN_POINT ( 'NONE',  ( 20.59039453120236018, -43.61606461192724282, -23.90179120638650900 ) ) ;
#3386 = CARTESIAN_POINT ( 'NONE',  ( -114.6415077203361221, 21.36885048555677358, -5.448690899135370636 ) ) ;
#3387 = CARTESIAN_POINT ( 'NONE',  ( -91.56559293963834989, 40.53558337403677569, -16.03295912088699993 ) ) ;
#3388 = CARTESIAN_POINT ( 'NONE',  ( 57.59792236341147031, 37.56421063658187620, 2.449293598294708485E-15 ) ) ;
#3389 = EDGE_LOOP ( 'NONE', ( #826, #17331, #17714, #7244 ) ) ;
#3390 = AXIS2_PLACEMENT_3D ( 'NONE', #10930, #24638, #6792 ) ;
#3391 = EDGE_CURVE ( 'NONE', #22320, #25804, #8962, .T. ) ;
#3392 = CARTESIAN_POINT ( 'NONE',  ( 44.82887508589845993, -36.15717056698611742, 18.94256811206760105 ) ) ;
#3393 = DIRECTION ( 'NONE',  ( -1.000000000000000000, -1.836970198721030181E-16, -2.465190328815661892E-32 ) ) ;
#3394 = CARTESIAN_POINT ( 'NONE',  ( 136.1360204305621551, -53.05693388239313890, 3.511608612530593199 ) ) ;
#3395 = CARTESIAN_POINT ( 'NONE',  ( -105.3755690713226585, -39.99999999999996447, -21.75974354311664527 ) ) ;
#3396 = CARTESIAN_POINT ( 'NONE',  ( -82.26983156992163515, 19.48351608823322678, -5.272298809006593423 ) ) ;
#3397 = CARTESIAN_POINT ( 'NONE',  ( -259.2033419157646676, -9.517827891722680178, 0.000000000000000000 ) ) ;
#3398 = CYLINDRICAL_SURFACE ( 'NONE', #20716, 74.99999999999991473 ) ;
#3399 = CARTESIAN_POINT ( 'NONE',  ( 200.0000000000000000, 5.800536564436440834, 18.10358378745109320 ) ) ;
#3400 = CARTESIAN_POINT ( 'NONE',  ( 170.0000000000000284, 15.47746304364896019, 19.80854622259152720 ) ) ;
#3401 = CARTESIAN_POINT ( 'NONE',  ( -105.3755690713226727, -15.38646221621807619, 15.38646221621768362 ) ) ;
#3402 = CARTESIAN_POINT ( 'NONE',  ( -208.1127848780264742, -10.60833733270725787, -67.17687982763172272 ) ) ;
#3403 = PRESENTATION_LAYER_ASSIGNMENT (  '', '', ( #442 ) ) ;
#3404 = CARTESIAN_POINT ( 'NONE',  ( -114.7820862557368997, 22.12833180681263556, -0.4894207860022879442 ) ) ;
#3405 = CARTESIAN_POINT ( 'NONE',  ( -86.86493150571057242, 8.366608963945132871, -19.60045294883092382 ) ) ;
#3406 = CARTESIAN_POINT ( 'NONE',  ( -208.1127848780264742, -10.60833733270725787, -67.17687982763172272 ) ) ;
#3408 = CARTESIAN_POINT ( 'NONE',  ( -213.1075012329537230, -18.58567234101102272, -37.98287015391260013 ) ) ;
#3407 = CARTESIAN_POINT ( 'NONE',  ( -162.0762913951020892, -1.198031840315659124, -57.76657433523998009 ) ) ;
#3409 = CARTESIAN_POINT ( 'NONE',  ( -192.9588430854689989, 10.23066800230756712, -10.23066800230735396 ) ) ;
#3410 = FACE_OUTER_BOUND ( 'NONE', #2257, .T. ) ;
#3411 = CARTESIAN_POINT ( 'NONE',  ( 107.5473083967439720, 23.99138244111466989, 0.000000000000000000 ) ) ;
#3412 = CARTESIAN_POINT ( 'NONE',  ( 0.2972598230770103767, -40.00000000000021316, 54.33493731733921805 ) ) ;
#3413 = CARTESIAN_POINT ( 'NONE',  ( -259.2033419157646676, -6.730120644403663199, 6.730120644403451813 ) ) ;
#3414 = CARTESIAN_POINT ( 'NONE',  ( -213.1075012329537230, 53.71589010951910836, 2.449293598294708485E-15 ) ) ;
#3415 = ORIENTED_EDGE ( 'NONE', *, *, #11169, .T. ) ;
#3416 = CARTESIAN_POINT ( 'NONE',  ( -86.96347745069644475, 12.89780903124410472, -43.67073346367977393 ) ) ;
#3417 = CARTESIAN_POINT ( 'NONE',  ( 89.37937299509916045, 21.71466159691463815, 8.994507335784314606 ) ) ;
#3418 = CARTESIAN_POINT ( 'NONE',  ( 90.68848423392005031, 8.814708751053737856, 21.28058941705803164 ) ) ;
#3419 = CARTESIAN_POINT ( 'NONE',  ( -70.30307074936186496, -22.52851052426727207, -10.20829450353408596 ) ) ;
#3420 = ORIENTED_EDGE ( 'NONE', *, *, #7342, .T. ) ;
#3421 = CARTESIAN_POINT ( 'NONE',  ( -195.5009199109952363, -44.52807166370936187, 18.44413118942235386 ) ) ;
#3422 = CARTESIAN_POINT ( 'NONE',  ( 199.9999999999999147, -15.08385563027219156, -11.56407354529143205 ) ) ;
#3423 = CARTESIAN_POINT ( 'NONE',  ( 27.26078259667537296, -17.35591035708258545, 41.90087417143249837 ) ) ;
#3424 = EDGE_CURVE ( 'NONE', #13855, #17045, #25460, .T. ) ;
#3425 = CARTESIAN_POINT ( 'NONE',  ( -626.9846540392142060, 75.00000000000000000, 34.99999999999999289 ) ) ;
#3426 = CARTESIAN_POINT ( 'NONE',  ( 199.0066333181452478, 19.18530965003537858, -5.635992787424102701 ) ) ;
#3427 = EDGE_CURVE ( 'NONE', #24064, #13093, #257, .T. ) ;
#3428 = FACE_OUTER_BOUND ( 'NONE', #4333, .T. ) ;
#3429 = CARTESIAN_POINT ( 'NONE',  ( 200.0000000000000000, 40.00000000000012790, -19.99999999999996092 ) ) ;
#3430 = CARTESIAN_POINT ( 'NONE',  ( -82.24286369198219404, -2.516305986770045688, 20.07657290678962170 ) ) ;
#3431 = CARTESIAN_POINT ( 'NONE',  ( -200.0000000000001421, -14.17215463606902404, -49.28189405767602693 ) ) ;
#3432 = CARTESIAN_POINT ( 'NONE',  ( 14.38125909742181285, -15.17850393972633505, 40.00000000000002132 ) ) ;
#3433 = AXIS2_PLACEMENT_3D ( 'NONE', #12831, #16813, #20951 ) ;
#3435 = CARTESIAN_POINT ( 'NONE',  ( -622.8776819133570370, 26.70401283558588901, -29.78701626806179092 ) ) ;
#3434 = CYLINDRICAL_SURFACE ( 'NONE', #13021, 29.99999999999999645 ) ;
#3436 = EDGE_CURVE ( 'NONE', #23332, #16255, #7824, .T. ) ;
#3437 = CARTESIAN_POINT ( 'NONE',  ( -192.9588430854689989, -14.46834944099973086, 0.000000000000000000 ) ) ;
#3438 = CARTESIAN_POINT ( 'NONE',  ( -259.2033419157646676, -30.48217210827743884, -40.00000000000002132 ) ) ;
#3439 = AXIS2_PLACEMENT_3D ( 'NONE', #18849, #2227, #25239 ) ;
#3440 = CARTESIAN_POINT ( 'NONE',  ( 192.4448373802100889, -20.00000000003938538, 0.000000000000000000 ) ) ;
#3441 = CARTESIAN_POINT ( 'NONE',  ( 199.9999999999999432, -1.727494763561684666E-13, 20.00000000000010303 ) ) ;
#3442 = AXIS2_PLACEMENT_3D ( 'NONE', #9692, #3450, #25808 ) ;
#3443 = PLANE ( 'NONE',  #15673 ) ;
#3444 = AXIS2_PLACEMENT_3D ( 'NONE', #3731, #1473, #7571 ) ;
#3445 = CARTESIAN_POINT ( 'NONE',  ( 132.4329763957084936, -29.78197873630821491, -12.33609950688606105 ) ) ;
#3446 = VERTEX_POINT ( 'NONE', #7334 ) ;
#3448 = CARTESIAN_POINT ( 'NONE',  ( -2.557884977113219716, 43.43882039326797440, -23.77085849411954044 ) ) ;
#3447 = CARTESIAN_POINT ( 'NONE',  ( 98.29820294267355507, 10.58389073156783233, -16.98253775143902544 ) ) ;
#3449 = CARTESIAN_POINT ( 'NONE',  ( -280.0000000000000568, 19.99999999999996092, 40.00000000000002132 ) ) ;
#3450 = DIRECTION ( 'NONE',  ( -1.000000000000000000, -1.836970198721030181E-16, 0.000000000000000000 ) ) ;
#3451 = DIRECTION ( 'NONE',  ( 0.000000000000000000, 0.000000000000000000, 1.000000000000000000 ) ) ;
#3452 = EDGE_LOOP ( 'NONE', ( #17676, #18778 ) ) ;
#3453 = ORIENTED_EDGE ( 'NONE', *, *, #11657, .F. ) ;
#3454 = CARTESIAN_POINT ( 'NONE',  ( -162.0762913951020892, -1.198031840385783919, 1.198031840385741731 ) ) ;
#3455 = DIRECTION ( 'NONE',  ( 1.000000000000000000, 1.836970198721030427E-16, -0.000000000000000000 ) ) ;
#3456 = ORIENTED_EDGE ( 'NONE', *, *, #21627, .T. ) ;
#3457 = CARTESIAN_POINT ( 'NONE',  ( -103.9474983244994490, 8.027156558344955783, -20.15710290851550113 ) ) ;
#3458 = EDGE_LOOP ( 'NONE', ( #25215, #16114, #9669, #11794 ) ) ;
#3459 = CARTESIAN_POINT ( 'NONE',  ( 200.0000000000000853, -13.44239485489230290, 13.44239485489200803 ) ) ;
#3460 = CIRCLE ( 'NONE', #18320, 69.99999999999994316 ) ;
#3461 = CARTESIAN_POINT ( 'NONE',  ( 169.9999999999999432, 22.62041470344884075, 9.369682556672378482 ) ) ;
#3462 = CARTESIAN_POINT ( 'NONE',  ( -56.48582580120559982, 50.09629031063966664, -6.472252184284094767 ) ) ;
#3463 = CARTESIAN_POINT ( 'NONE',  ( -210.0000000000000284, 82.50000000000008527, -52.49999999999978684 ) ) ;
#3464 =( BOUNDED_CURVE ( )  B_SPLINE_CURVE ( 3, ( #22414, #8556, #16672, #20411 ),
 .UNSPECIFIED., .F., .F. ) 
 B_SPLINE_CURVE_WITH_KNOTS ( ( 4, 4 ),
 ( 0.007854122480096750389, 0.01576650722528986220 ),
 .UNSPECIFIED. ) 
 CURVE ( )  GEOMETRIC_REPRESENTATION_ITEM ( )  RATIONAL_B_SPLINE_CURVE ( ( 0.9999999999999497069, 0.8893928793063790028, 0.7971366613349945007, 0.7232313460858209586 ) ) 
 REPRESENTATION_ITEM ( '' )  );
#3465 = CARTESIAN_POINT ( 'NONE',  ( -91.56559293963834989, 6.234561990864368500E-14, -22.67402823373191723 ) ) ;
#3466 = DIRECTION ( 'NONE',  ( 0.000000000000000000, 0.000000000000000000, -1.000000000000000000 ) ) ;
#3467 = CARTESIAN_POINT ( 'NONE',  ( -189.9999999999999716, 82.50000000000008527, -52.49999999999977973 ) ) ;
#3468 = CARTESIAN_POINT ( 'NONE',  ( -65.65555754753384576, 11.16466304451119207, -24.04429191298344293 ) ) ;
#3469 = CARTESIAN_POINT ( 'NONE',  ( -162.0762913951020892, -1.202636532414034422E-14, -1.694272876828323948 ) ) ;
#3470 = CARTESIAN_POINT ( 'NONE',  ( -162.0762913951020892, -39.99999999999961631, -41.69427287692722928 ) ) ;
#3471 = CARTESIAN_POINT ( 'NONE',  ( -200.0000000000000853, -46.19968414209463958, -18.59955921182009320 ) ) ;
#3472 = CARTESIAN_POINT ( 'NONE',  ( 130.8568914410475088, -4.207082182989324792, -52.36146031193423056 ) ) ;
#3473 = CARTESIAN_POINT ( 'NONE',  ( -199.9999999999999716, 16.85576820966628375, -47.13392792188996339 ) ) ;
#3474 = EDGE_CURVE ( 'NONE', #16387, #11522, #2624, .T. ) ;
#3475 = CARTESIAN_POINT ( 'NONE',  ( 14.38125909742183062, -67.30136555898262429, 10.73282306405838682 ) ) ;
#3476 = CARTESIAN_POINT ( 'NONE',  ( 98.29820294267314296, 18.47759065023127079, 7.653668647304074923 ) ) ;
#3477 = DIRECTION ( 'NONE',  ( 0.000000000000000000, 0.000000000000000000, -1.000000000000000000 ) ) ;
#3478 = FACE_OUTER_BOUND ( 'NONE', #10035, .T. ) ;
#3479 = CARTESIAN_POINT ( 'NONE',  ( -192.9588430854689989, -8.596193650988133061E-14, 14.46834944099969533 ) ) ;
#3480 = CARTESIAN_POINT ( 'NONE',  ( 136.1360204305621551, -24.77266263493126885, 31.79587985999256006 ) ) ;
#3481 = AXIS2_PLACEMENT_3D ( 'NONE', #7276, #3549, #15638 ) ;
#3482 = CARTESIAN_POINT ( 'NONE',  ( 146.6084372240433709, -32.08495691632075619, 24.48358557860298035 ) ) ;
#3483 = CARTESIAN_POINT ( 'NONE',  ( -151.4802930569721582, -11.09498731348586809, -33.96623840869666111 ) ) ;
#3484 = CARTESIAN_POINT ( 'NONE',  ( -99.21568817060989431, 16.03295912088691821, 16.03295912088721309 ) ) ;
#3485 = ORIENTED_EDGE ( 'NONE', *, *, #16965, .T. ) ;
#3486 = CARTESIAN_POINT ( 'NONE',  ( -192.9588430854689989, 38.51493924976983152, -38.51493924976893624 ) ) ;
#3487 = CARTESIAN_POINT ( 'NONE',  ( -397.9898987322331436, 69.99999999999990052, 0.000000000000000000 ) ) ;
#3488 = DIRECTION ( 'NONE',  ( 0.000000000000000000, 1.000000000000000000, 0.000000000000000000 ) ) ;
#3489 = CARTESIAN_POINT ( 'NONE',  ( -82.23726319249651340, -1.560758868889668476E-13, 20.19517362732914734 ) ) ;
#3490 = EDGE_LOOP ( 'NONE', ( #23899, #8227, #21798, #19049, #6930, #1071, #22614, #7062, #14089, #10565, #17173, #6596, #1301, #5112, #2291, #13494 ) ) ;
#3491 = CARTESIAN_POINT ( 'NONE',  ( 130.8568914410475372, -3.326198072800416995E-13, 34.05028731879788495 ) ) ;
#3492 = CARTESIAN_POINT ( 'NONE',  ( -1.255560987024274322, -23.98612781107772918, 43.73013506549201423 ) ) ;
#3493 = CARTESIAN_POINT ( 'NONE',  ( -65.65550967573656749, 11.16467289560276122, 24.04430752631849799 ) ) ;
#3494 = EDGE_LOOP ( 'NONE', ( #17738, #5415, #9928, #20149, #22246, #12129, #8634 ) ) ;
#3495 = ORIENTED_EDGE ( 'NONE', *, *, #4923, .T. ) ;
#3496 = CARTESIAN_POINT ( 'NONE',  ( 14.38125909742180752, 55.17850393971008316, -40.00000000000002132 ) ) ;
#3497 = CARTESIAN_POINT ( 'NONE',  ( -280.0000000000000568, -14.14213562373078226, -42.42640687119295251 ) ) ;
#3498 = CARTESIAN_POINT ( 'NONE',  ( -280.0000000000000568, 39.99999999999990763, 20.00000000000015987 ) ) ;
#3499 = CARTESIAN_POINT ( 'NONE',  ( -114.7826396787322665, -15.64922767586156915, -15.64922767586183383 ) ) ;
#3500 = AXIS2_PLACEMENT_3D ( 'NONE', #9344, #7214, #17198 ) ;
#3501 = DIRECTION ( 'NONE',  ( 1.000000000000000000, 1.836970198721030181E-16, 0.000000000000000000 ) ) ;
#3502 = CARTESIAN_POINT ( 'NONE',  ( 136.1360204305621551, 39.99999999999968026, 35.03383547441337953 ) ) ;
#3503 = CARTESIAN_POINT ( 'NONE',  ( 192.4448373802101173, -40.00000000000005684, 19.99999999996046185 ) ) ;
#3504 = CARTESIAN_POINT ( 'NONE',  ( 200.0000000000001705, -16.91021041590709473, -8.683373960011902426 ) ) ;
#3505 = CARTESIAN_POINT ( 'NONE',  ( 91.82158438592156813, 40.00000000000009948, -17.20528682183286051 ) ) ;
#3506 = CARTESIAN_POINT ( 'NONE',  ( -190.0000000000001705, 69.99999999999994316, 0.000000000000000000 ) ) ;
#3507 = CARTESIAN_POINT ( 'NONE',  ( -105.3755690713226727, -15.38646221621807619, 15.38646221621768362 ) ) ;
#3508 = CARTESIAN_POINT ( 'NONE',  ( -192.9588430854690273, -10.23066800231931239, -66.79921049724377724 ) ) ;
#3509 = CARTESIAN_POINT ( 'NONE',  ( 136.1360204305621266, -24.77266263493151044, 24.77266263493093135 ) ) ;
#3510 = CARTESIAN_POINT ( 'NONE',  ( -259.2033419157646676, -1.473088368616265084E-13, 9.517827891722632216 ) ) ;
#3511 = CARTESIAN_POINT ( 'NONE',  ( 150.0000000000000284, -125.7889608577475116, 82.50000000000001421 ) ) ;
#3512 = CARTESIAN_POINT ( 'NONE',  ( 4.995406935893293543, -15.24977328854832592, 0.000000000000000000 ) ) ;
#3513 = CARTESIAN_POINT ( 'NONE',  ( -192.9588430854690273, -54.46834944101725284, -40.00000000000002132 ) ) ;
#3514 = CARTESIAN_POINT ( 'NONE',  ( 57.59792236341147031, 1.722363176415065089, -1.722363176415036445 ) ) ;
#3515 = CARTESIAN_POINT ( 'NONE',  ( 19.06497207195981503, -14.19242893257840166, 0.000000000000000000 ) ) ;
#3516 = CARTESIAN_POINT ( 'NONE',  ( 7.307793593482452721, -44.91153572052488840, -24.85783611765727485 ) ) ;
#3517 = CARTESIAN_POINT ( 'NONE',  ( -259.2033419157646676, 39.99999999999987921, 9.517827891723049660 ) ) ;
#3518 = CARTESIAN_POINT ( 'NONE',  ( -100.7734535825088358, 12.25131212657480440, 12.25131212657487012 ) ) ;
#3519 = CARTESIAN_POINT ( 'NONE',  ( -162.0762913951020892, 41.69427287682832173, 2.449293598294708485E-15 ) ) ;
#3520 = ORIENTED_EDGE ( 'NONE', *, *, #10207, .F. ) ;
#3521 = CARTESIAN_POINT ( 'NONE',  ( 23.40652632867992367, -42.84715492600945197, 23.33303889678550647 ) ) ;
#3522 = CYLINDRICAL_SURFACE ( 'NONE', #17630, 5.000000000000004441 ) ;
#3523 = CARTESIAN_POINT ( 'NONE',  ( 192.4448373802100889, 14.14213562370310662, 14.14213562370312438 ) ) ;
#3524 = CARTESIAN_POINT ( 'NONE',  ( 14.38125909742181818, -1.924622159709266762E-13, 55.17850393972636880 ) ) ;
#3525 = CARTESIAN_POINT ( 'NONE',  ( -135.8532207217289738, -6.472252184284280396, 6.472252184284099208 ) ) ;
#3526 = CARTESIAN_POINT ( 'NONE',  ( -192.9588430854690273, 14.46834944099966336, -40.00000000000002132 ) ) ;
#3527 = CARTESIAN_POINT ( 'NONE',  ( -716.9846540392142060, 52.49999999999986500, 82.49999999999998579 ) ) ;
#3528 = CARTESIAN_POINT ( 'NONE',  ( 200.0000000000000284, 12.51656570147539327, 14.30544205704861760 ) ) ;
#3529 = CARTESIAN_POINT ( 'NONE',  ( -87.02115643441359794, 5.416235655370554625, -20.76466217920002677 ) ) ;
#3530 = CARTESIAN_POINT ( 'NONE',  ( -56.48582580120559271, -6.472252184284276844, 6.472252184284108978 ) ) ;
#3531 = CARTESIAN_POINT ( 'NONE',  ( -162.0762913951020892, -29.48230308784744125, -29.48230308784792442 ) ) ;
#3532 = EDGE_CURVE ( 'NONE', #21182, #3446, #21578, .T. ) ;
#3533 = CARTESIAN_POINT ( 'NONE',  ( -77.55640685876512919, -22.13135000837101884, -1.398618882111774653 ) ) ;
#3534 = CARTESIAN_POINT ( 'NONE',  ( -86.90968602919654984, 19.36074508458825605, -9.002619558036901282 ) ) ;
#3535 = CARTESIAN_POINT ( 'NONE',  ( 151.7948205124835681, 51.78348778862544322, -4.785054706298002891 ) ) ;
#3537 = CARTESIAN_POINT ( 'NONE',  ( -192.9588430854690273, 10.23066800229588758, -66.79921049721882298 ) ) ;
#3536 = CARTESIAN_POINT ( 'NONE',  ( 146.6084372240433709, 52.76785682606523409, -3.800685668858194255 ) ) ;
#3538 = CARTESIAN_POINT ( 'NONE',  ( 146.6084372240433709, -24.48358557860284179, -32.08495691632087699 ) ) ;
#3539 = FACE_OUTER_BOUND ( 'NONE', #4304, .T. ) ;
#3540 = CARTESIAN_POINT ( 'NONE',  ( 91.82158438592158234, -12.16597498397761967, -12.16597498397768007 ) ) ;
#3542 = CARTESIAN_POINT ( 'NONE',  ( -135.8532207217289738, -40.00000000000001421, -9.153146818113709671 ) ) ;
#3541 = CARTESIAN_POINT ( 'NONE',  ( -91.56559293963834989, -16.03295912088728414, 16.03295912088688269 ) ) ;
#3543 = CARTESIAN_POINT ( 'NONE',  ( -30.26275506840323359, -1.198031551616339341, 57.76657404653985139 ) ) ;
#3544 = CARTESIAN_POINT ( 'NONE',  ( -91.56559293963836410, 16.03295912088692177, 16.03295912088721664 ) ) ;
#3545 = CARTESIAN_POINT ( 'NONE',  ( -280.0000000000000568, 19.99999999999995737, 40.00000000000002132 ) ) ;
#3546 = ORIENTED_EDGE ( 'NONE', *, *, #19780, .F. ) ;
#3547 = CARTESIAN_POINT ( 'NONE',  ( -192.9588430854689989, 10.23066800230742679, 10.23066800230749607 ) ) ;
#3548 = CARTESIAN_POINT ( 'NONE',  ( -317.0000000000000568, -4.857225732735059864E-14, 0.000000000000000000 ) ) ;
#3549 = DIRECTION ( 'NONE',  ( -1.303213150798907793E-16, 1.000000000000000000, -1.682156097916904081E-16 ) ) ;
#3550 = CARTESIAN_POINT ( 'NONE',  ( 57.59792236341147031, -2.435789363418150444, 0.000000000000000000 ) ) ;
#3551 = ORIENTED_EDGE ( 'NONE', *, *, #21174, .T. ) ;
#3552 = CARTESIAN_POINT ( 'NONE',  ( -189.2667466962258231, -43.39859272266359369, 17.97628569363223505 ) ) ;
#3553 = CARTESIAN_POINT ( 'NONE',  ( 200.0000000000002274, -18.85575486854367355, -2.482946933799725642 ) ) ;
#3554 = CARTESIAN_POINT ( 'NONE',  ( 98.29820294267315717, -7.653668647304114891, 18.47759065023121039 ) ) ;
#3555 = CARTESIAN_POINT ( 'NONE',  ( 23.10188454848542605, 13.81611343686443405, -46.91040837924335705 ) ) ;
#3556 = CARTESIAN_POINT ( 'NONE',  ( 199.0060750228415429, 7.941611777091910795, -18.35102805502410561 ) ) ;
#3557 = CARTESIAN_POINT ( 'NONE',  ( -626.9846540392142060, 75.00000000000000000, -60.00000000000000000 ) ) ;
#3558 = CARTESIAN_POINT ( 'NONE',  ( 136.1360204305621551, 40.00000000000002842, 4.966164525587208445 ) ) ;
#3559 = CARTESIAN_POINT ( 'NONE',  ( -82.23726319249655603, -1.556969561919214781E-13, 20.19517362732914734 ) ) ;
#3560 = CARTESIAN_POINT ( 'NONE',  ( -200.0000000000000000, -20.93268228684324939, -45.36622447512537093 ) ) ;
#3561 = CARTESIAN_POINT ( 'NONE',  ( -280.0000000000000568, -20.00000000000007105, 40.00000000000002132 ) ) ;
#3563 = DIRECTION ( 'NONE',  ( 0.000000000000000000, 0.000000000000000000, 1.000000000000000000 ) ) ;
#3562 = CARTESIAN_POINT ( 'NONE',  ( -184.9730489280194945, 13.59277546670732661, -45.83721239347746490 ) ) ;
#3564 = LINE ( 'NONE', #25933, #6385 ) ;
#3565 = CARTESIAN_POINT ( 'NONE',  ( 57.59792236341147031, 2.435789363418171760, 0.000000000000000000 ) ) ;
#3566 = CARTESIAN_POINT ( 'NONE',  ( 19.06497207195980792, 14.19242893257840876, 0.000000000000000000 ) ) ;
#3567 = CARTESIAN_POINT ( 'NONE',  ( 19.06497207195982924, -39.99999999999945288, -54.19242893257885640 ) ) ;
#3568 = CARTESIAN_POINT ( 'NONE',  ( 0.2972598230769957217, 1.502051041545559470E-13, -14.33493731733933352 ) ) ;
#3569 = PRODUCT_DEFINITION_SHAPE ( 'NONE', 'NONE',  #6229 ) ;
#3570 = CARTESIAN_POINT ( 'NONE',  ( -213.1075012329537230, 18.58567234101174037, -37.98287015391222354 ) ) ;
#3571 = VERTEX_POINT ( 'NONE', #11332 ) ;
#3572 = DIRECTION ( 'NONE',  ( 0.01051738792034368278, 0.3995761383040613568, 0.9166396752537755432 ) ) ;
#3573 = CARTESIAN_POINT ( 'NONE',  ( 4.995406935893293543, -15.24977328854832592, 0.000000000000000000 ) ) ;
#3574 = CARTESIAN_POINT ( 'NONE',  ( 151.7948205124836250, -23.49921654116371883, 23.49921654116317526 ) ) ;
#3575 = CARTESIAN_POINT ( 'NONE',  ( -198.0012400611977057, 49.19397081476455469, -14.15884001207452592 ) ) ;
#3576 = ITEM_DEFINED_TRANSFORMATION ( 'NONE', 'NONE', #9988,  #21058 ) ;
#3577 = VERTEX_POINT ( 'NONE', #13331 ) ;
#3578 = VERTEX_POINT ( 'NONE', #23331 ) ;
#3579 = FACE_OUTER_BOUND ( 'NONE', #18647, .T. ) ;
#3580 = CARTESIAN_POINT ( 'NONE',  ( 22.79879570922434695, -43.16776802602853280, -17.88067497375694970 ) ) ;
#3581 = ORIENTED_EDGE ( 'NONE', *, *, #17434, .T. ) ;
#3582 = CARTESIAN_POINT ( 'NONE',  ( -105.3755690713226585, 18.24025645688350750, -40.00000000000002132 ) ) ;
#3583 = CARTESIAN_POINT ( 'NONE',  ( -280.0000000000000000, -10.00000000000005151, -6.902532920683853297E-30 ) ) ;
#3584 = EDGE_LOOP ( 'NONE', ( #7054, #10530, #26087, #25050 ) ) ;
#3585 = CARTESIAN_POINT ( 'NONE',  ( 200.0000000000005684, -1.253076495463282924, 18.97792690268338234 ) ) ;
#3586 = DIRECTION ( 'NONE',  ( 0.000000000000000000, -0.3656393565213487129, 0.9307566067252244224 ) ) ;
#3587 = CARTESIAN_POINT ( 'NONE',  ( -280.0000000000000000, 14.14213562373088351, 14.14213562373098654 ) ) ;
#3588 = DIRECTION ( 'NONE',  ( -1.000000000000000000, -1.836970198721030181E-16, -0.000000000000000000 ) ) ;
#3589 = CARTESIAN_POINT ( 'NONE',  ( -259.2033419157646676, -1.438356298054549103E-14, -9.517827891722632216 ) ) ;
#3590 = CARTESIAN_POINT ( 'NONE',  ( -30.26275506840324070, 1.198031551616724366, -57.76657404653984429 ) ) ;
#3591 = CARTESIAN_POINT ( 'NONE',  ( -612.0709805440841365, -1.322736627157470569E-16, 0.000000000000000000 ) ) ;
#3592 = FACE_OUTER_BOUND ( 'NONE', #26047, .T. ) ;
#3593 = DIRECTION ( 'NONE',  ( 0.000000000000000000, 0.000000000000000000, 1.000000000000000000 ) ) ;
#3594 = CARTESIAN_POINT ( 'NONE',  ( -100.7734535825088500, -39.99999999999986500, -17.32597176626853397 ) ) ;
#3595 = CARTESIAN_POINT ( 'NONE',  ( -199.9999999999999432, -44.86773131993655994, -24.32899771311787518 ) ) ;
#3596 = B_SPLINE_CURVE_WITH_KNOTS ( 'NONE', 3,
 ( #3257, #25875, #9248, #26016, #7619, #11753, #23605, #15734 ),
 .UNSPECIFIED., .F., .F.,
 ( 4, 2, 2, 4 ),
 ( 0.008473926332009199328, 0.01052499632800952059, 0.01257606632400984359, 0.01667820631601048265 ),
 .UNSPECIFIED. ) ;
#3597 = CARTESIAN_POINT ( 'NONE',  ( -162.0762913951021176, -29.48230308784755493, -27.08623940707632372 ) ) ;
#3598 = CARTESIAN_POINT ( 'NONE',  ( -208.1127848780265026, -15.00245453012673202, 0.000000000000000000 ) ) ;
#3599 = CARTESIAN_POINT ( 'NONE',  ( -259.2033419157646676, -21.55415060305854524, 21.55415060305827524 ) ) ;
#3600 = DIRECTION ( 'NONE',  ( -0.01051738777840956381, -0.9166396752739809362, -0.3995761382614453905 ) ) ;
#3601 = CARTESIAN_POINT ( 'NONE',  ( -3.763361371728476623, -47.08953757622906267, 13.84281709279670380 ) ) ;
#3602 = CARTESIAN_POINT ( 'NONE',  ( -280.0000000000000568, 39.99999999999976552, 20.00000000000043343 ) ) ;
#3603 = CARTESIAN_POINT ( 'NONE',  ( -162.0762913951020892, -3.568845385355699554E-14, 1.694272876828323948 ) ) ;
#3604 = CARTESIAN_POINT ( 'NONE',  ( 146.6084372240433709, -24.48358557860329299, 32.08495691632052882 ) ) ;
#3605 = CARTESIAN_POINT ( 'NONE',  ( 0.2972598230769976091, -10.13633138497465147, -10.13633138497482733 ) ) ;
#3606 = CARTESIAN_POINT ( 'NONE',  ( -189.1288815661887099, -23.62384257861826597, -43.24061771117260378 ) ) ;
#3607 = CARTESIAN_POINT ( 'NONE',  ( -91.56559293963836410, -12.25131212657462321, -44.31723036834905827 ) ) ;
#3608 = ORIENTED_EDGE ( 'NONE', *, *, #2296, .T. ) ;
#3609 = CARTESIAN_POINT ( 'NONE',  ( -162.0762913951020892, 1.198031840456041497, -57.76657433537918251 ) ) ;
#3610 = CARTESIAN_POINT ( 'NONE',  ( -238.4067589809705794, -0.9644942799826263791, -40.00000000000002132 ) ) ;
#3611 = EDGE_CURVE ( 'NONE', #16217, #18680, #15942, .T. ) ;
#3612 = CARTESIAN_POINT ( 'NONE',  ( -4.039451493210489907, 13.82811171175507603, -46.99046209229789639 ) ) ;
#3613 = CARTESIAN_POINT ( 'NONE',  ( -86.96347745069644475, -15.38646221621738164, -41.18208027870615240 ) ) ;
#3614 = DIRECTION ( 'NONE',  ( -1.303213150798907793E-16, 1.000000000000000000, -1.682156097916904081E-16 ) ) ;
#3615 = ORIENTED_EDGE ( 'NONE', *, *, #8737, .F. ) ;
#3616 = AXIS2_PLACEMENT_3D ( 'NONE', #19733, #23355, #5132 ) ;
#3617 = CARTESIAN_POINT ( 'NONE',  ( 151.7948205124836250, -3.202120068677277203E-13, 33.23291073765553705 ) ) ;
#3618 = CARTESIAN_POINT ( 'NONE',  ( 199.0253302299943812, -18.92118621875344786, 6.501515187515664707 ) ) ;
#3619 = EDGE_CURVE ( 'NONE', #15141, #22947, #10886, .T. ) ;
#3620 = CARTESIAN_POINT ( 'NONE',  ( -17.28139728211933956, 20.85871090886837109, 39.07633224434955821 ) ) ;
#3621 = ORIENTED_EDGE ( 'NONE', *, *, #5241, .F. ) ;
#3622 = ORIENTED_EDGE ( 'NONE', *, *, #11647, .T. ) ;
#3623 = CARTESIAN_POINT ( 'NONE',  ( 130.8568914410475372, 5.949712681206715814, 2.449293598294708485E-15 ) ) ;
#3624 = CARTESIAN_POINT ( 'NONE',  ( 14.38125909742181285, -10.73282306404727393, 10.73282306404716380 ) ) ;
#3625 = CARTESIAN_POINT ( 'NONE',  ( -30.26275506840324425, 39.99999999999987210, 41.69427246844643520 ) ) ;
#3626 = EDGE_CURVE ( 'NONE', #17304, #7651, #19784, .T. ) ;
#3627 = EDGE_CURVE ( 'NONE', #10094, #6927, #8937, .T. ) ;
#3628 = CARTESIAN_POINT ( 'NONE',  ( -86.86493150571118349, -19.60045294882770506, 8.366608963953762412 ) ) ;
#3629 =( GEOMETRIC_REPRESENTATION_CONTEXT ( 3 ) GLOBAL_UNCERTAINTY_ASSIGNED_CONTEXT ( ( #21784 ) ) GLOBAL_UNIT_ASSIGNED_CONTEXT ( ( #17040, #24777, #825 ) ) REPRESENTATION_CONTEXT ( 'NONE', 'WORKASPACE' ) );
#3630 = PLANE ( 'NONE',  #18958 ) ;
#3631 = CARTESIAN_POINT ( 'NONE',  ( -56.48582580120559271, -1.062504017861011783E-13, 9.153146818113587102 ) ) ;
#3632 = CARTESIAN_POINT ( 'NONE',  ( 200.0000000000000853, -13.44239485489230290, 13.44239485489200803 ) ) ;
#3633 = CIRCLE ( 'NONE', #4066, 14.99999999999999822 ) ;
#3634 = CIRCLE ( 'NONE', #22755, 14.99999999999999822 ) ;
#3635 = DIRECTION ( 'NONE',  ( 0.000000000000000000, 0.000000000000000000, 1.000000000000000000 ) ) ;
#3636 = CARTESIAN_POINT ( 'NONE',  ( -4.112199523540028601, -13.82298295336114791, -46.96527782736897905 ) ) ;
#3637 = CARTESIAN_POINT ( 'NONE',  ( 200.0000000000000000, 42.42640687119310172, -14.14213562373052646 ) ) ;
#3638 = DIRECTION ( 'NONE',  ( -1.000000000000000000, -1.836970198721030181E-16, 0.000000000000000000 ) ) ;
#3639 = CARTESIAN_POINT ( 'NONE',  ( 130.8568914410475088, -4.207082182989324792, -52.36146031193423056 ) ) ;
#3640 = CARTESIAN_POINT ( 'NONE',  ( -135.8532207217289738, -40.00000000000014211, 9.153146818113153671 ) ) ;
#3641 = CARTESIAN_POINT ( 'NONE',  ( -716.9846540392142060, -66.50000000000001421, -71.50000000000005684 ) ) ;
#3642 = CARTESIAN_POINT ( 'NONE',  ( 130.8568914410475372, 34.05028731879791337, 0.000000000000000000 ) ) ;
#3643 = CARTESIAN_POINT ( 'NONE',  ( -198.0356074513804572, -55.37879056874826489, 40.00000000000002132 ) ) ;
#3644 = AXIS2_PLACEMENT_3D ( 'NONE', #26029, #19888, #19624 ) ;
#3645 = CARTESIAN_POINT ( 'NONE',  ( 151.7948205124835681, 51.78348778862537927, 4.785054706298732086 ) ) ;
#3646 = AXIS2_PLACEMENT_3D ( 'NONE', #3911, #15850, #6030 ) ;
#3647 = CARTESIAN_POINT ( 'NONE',  ( -135.8532207217289454, -30.84685318188648750, -40.00000000000002132 ) ) ;
#3648 = CARTESIAN_POINT ( 'NONE',  ( 146.6084372240433993, -24.48358557860353457, 24.48358557860296258 ) ) ;
#3649 = CARTESIAN_POINT ( 'NONE',  ( 57.59792236341147031, -1.493297263419786540E-14, 2.435789363418160658 ) ) ;
#3650 = CARTESIAN_POINT ( 'NONE',  ( -213.1075012329537230, 37.98287015391228749, 37.98287015391245802 ) ) ;
#3651 = CARTESIAN_POINT ( 'NONE',  ( -192.9588430854690273, 54.46834944098218756, -40.00000000000002132 ) ) ;
#3652 = ORIENTED_EDGE ( 'NONE', *, *, #13762, .T. ) ;
#3653 = CARTESIAN_POINT ( 'NONE',  ( -626.9846540392097722, 75.00000000000000000, 59.99999999999999289 ) ) ;
#3654 = AXIS2_PLACEMENT_3D ( 'NONE', #4347, #5933, #18024 ) ;
#3655 = CARTESIAN_POINT ( 'NONE',  ( -200.0000000000000853, -24.82633483071228753, -44.86878812508721381 ) ) ;
#3656 = CARTESIAN_POINT ( 'NONE',  ( -30.26275506840325136, 29.48230279907798135, -27.08623969584585112 ) ) ;
#3657 = CARTESIAN_POINT ( 'NONE',  ( -208.1127848780265026, -2.327190355601776466E-13, 55.00245453012672670 ) ) ;
#3658 = CARTESIAN_POINT ( 'NONE',  ( -208.1127848780265026, 10.60833733269551615, -10.60833733269529766 ) ) ;
#3659 = CARTESIAN_POINT ( 'NONE',  ( 136.1360204305621266, -3.419521671106983309E-13, 35.03383547441296741 ) ) ;
#3660 = CARTESIAN_POINT ( 'NONE',  ( -91.56559293963834989, -22.67402823373193499, 0.000000000000000000 ) ) ;
#3661 = CARTESIAN_POINT ( 'NONE',  ( 180.0000000000000000, -35.78896085774750446, -65.91016826501511616 ) ) ;
#3662 = CARTESIAN_POINT ( 'NONE',  ( 199.9999999999998579, -4.480715147297966716, 18.47471730767352938 ) ) ;
#3663 = CARTESIAN_POINT ( 'NONE',  ( 199.9999999999999716, -14.29283438936585604, -12.53096660533077689 ) ) ;
#3664 = CARTESIAN_POINT ( 'NONE',  ( -192.9588430854689989, 38.51493924976983152, -38.51493924976893624 ) ) ;
#3665 = CARTESIAN_POINT ( 'NONE',  ( -86.96347745069643054, 15.38646221621821297, -41.18208027870583265 ) ) ;
#3666 = CARTESIAN_POINT ( 'NONE',  ( 130.8568914410475372, 24.07718906447243867, -24.07718906447216156 ) ) ;
#3667 = LINE ( 'NONE', #5931, #9143 ) ;
#3668 = CARTESIAN_POINT ( 'NONE',  ( 163.1118516004056573, 47.56205970284970164, -9.006482792073828847 ) ) ;
#3669 = VECTOR ( 'NONE', #5582, 999.9999999999998863 ) ;
#3671 = CARTESIAN_POINT ( 'NONE',  ( 14.38125909742181285, -17.55144818341421598, -39.01709431150935359 ) ) ;
#3670 = CARTESIAN_POINT ( 'NONE',  ( 57.59792236341147031, 30.00663442387720181, -26.56190807104661289 ) ) ;
#3672 = CARTESIAN_POINT ( 'NONE',  ( 130.8568914410475088, -52.36146031193413108, -4.207082182990267150 ) ) ;
#3673 = DIRECTION ( 'NONE',  ( 0.000000000000000000, -1.000000000000000000, 0.000000000000000000 ) ) ;
#3674 = CARTESIAN_POINT ( 'NONE',  ( -215.0000000000000284, 66.50000000000001421, -66.50000000000005684 ) ) ;
#3676 = CARTESIAN_POINT ( 'NONE',  ( 130.8568914410475372, 1.429239637432775288E-13, -34.05028731879788495 ) ) ;
#3675 = CARTESIAN_POINT ( 'NONE',  ( 14.38125909742180220, 39.01709431150892016, 17.55144818341517166 ) ) ;
#3677 = CARTESIAN_POINT ( 'NONE',  ( -56.48582580120559982, 34.75652343174597547, 21.81201906317791384 ) ) ;
#3678 = CARTESIAN_POINT ( 'NONE',  ( -280.0000000000000000, -14.14213562373118549, 14.14213562373078936 ) ) ;
#3679 = CARTESIAN_POINT ( 'NONE',  ( -86.96347745069644475, -21.75974354311652093, 40.00000000000002132 ) ) ;
#3680 = ORIENTED_EDGE ( 'NONE', *, *, #8682, .T. ) ;
#3681 = CARTESIAN_POINT ( 'NONE',  ( 19.06497207195980792, 66.60410523465817789, 10.03556273973446800 ) ) ;
#3682 = VECTOR ( 'NONE', #18497, 1000.000000000000000 ) ;
#3683 = CIRCLE ( 'NONE', #8352, 15.00000000000000178 ) ;
#3684 = DIRECTION ( 'NONE',  ( 0.000000000000000000, 0.000000000000000000, 1.000000000000000000 ) ) ;
#3685 = CARTESIAN_POINT ( 'NONE',  ( -213.1075012329537230, 13.71589010951907994, 0.000000000000000000 ) ) ;
#3686 = ORIENTED_EDGE ( 'NONE', *, *, #9254, .T. ) ;
#3687 = CARTESIAN_POINT ( 'NONE',  ( -190.0144222803064338, -43.47820992357731029, 23.79986276082939156 ) ) ;
#3688 = CARTESIAN_POINT ( 'NONE',  ( -295.0000000000000568, -4.857225732735059864E-14, 0.000000000000000000 ) ) ;
#3689 = EDGE_CURVE ( 'NONE', #10975, #23552, #25752, .T. ) ;
#3690 = CARTESIAN_POINT ( 'NONE',  ( -3.434479974377895761, -17.93814274724460844, 43.30650750418254802 ) ) ;
#3691 = SHAPE_REPRESENTATION ( 'Coupling rod', ( #21058 ), #2358 ) ;
#3692 = CARTESIAN_POINT ( 'NONE',  ( 23.84827734669535459, 13.76599369847180121, -46.63681169410599381 ) ) ;
#3693 = CARTESIAN_POINT ( 'NONE',  ( 199.0058097323984327, 9.278912463403225175, -17.71230630396810213 ) ) ;
#3694 = DIRECTION ( 'NONE',  ( 1.000000000000000000, 1.836970198721030427E-16, -0.000000000000000000 ) ) ;
#3695 = DIRECTION ( 'NONE',  ( 1.000000000000000000, 0.000000000000000000, 0.000000000000000000 ) ) ;
#3696 = CIRCLE ( 'NONE', #4514, 15.00000000000000355 ) ;
#3697 = CARTESIAN_POINT ( 'NONE',  ( -208.1127848780264742, 10.60833733268383483, -67.17687982760675425 ) ) ;
#3698 = CARTESIAN_POINT ( 'NONE',  ( 0.2972598230769983307, -14.33493731733933352, 40.00000000000002132 ) ) ;
#3700 = CARTESIAN_POINT ( 'NONE',  ( -601.1755229097230995, 36.95942061122438105, -15.32481103596387406 ) ) ;
#3699 = DIRECTION ( 'NONE',  ( -1.000000000000000000, 0.000000000000000000, 0.000000000000000000 ) ) ;
#3701 = CARTESIAN_POINT ( 'NONE',  ( 4.995406935893293543, -15.24977328854832592, 0.000000000000000000 ) ) ;
#3703 = EDGE_CURVE ( 'NONE', #8862, #19485, #1752, .T. ) ;
#3702 = B_SPLINE_CURVE_WITH_KNOTS ( 'NONE', 3,
 ( #7612, #19999, #5377, #23722, #13604, #1785, #25613, #7358 ),
 .UNSPECIFIED., .F., .F.,
 ( 4, 2, 2, 4 ),
 ( 0.008396858476685838471, 0.01250098582283842678, 0.01455304949591472267, 0.01660511316899102030 ),
 .UNSPECIFIED. ) ;
#3704 = CARTESIAN_POINT ( 'NONE',  ( 130.8568914410475088, 34.05028731879790627, -40.00000000000002132 ) ) ;
#3705 = CARTESIAN_POINT ( 'NONE',  ( -198.0356074513804572, 15.37879056873066830, 40.00000000000002132 ) ) ;
#3706 = CIRCLE ( 'NONE', #16456, 5.000000000000046185 ) ;
#3707 = CARTESIAN_POINT ( 'NONE',  ( 163.1118516004056573, -39.99999999999986500, -12.73709011382517353 ) ) ;
#3708 = CARTESIAN_POINT ( 'NONE',  ( 130.8568914410475372, -3.326198072800416995E-13, 34.05028731879788495 ) ) ;
#3709 = CARTESIAN_POINT ( 'NONE',  ( 146.6084372240433993, 24.48358557860307272, 24.48358557860347418 ) ) ;
#3710 = EDGE_CURVE ( 'NONE', #3578, #3746, #10435, .T. ) ;
#3711 = ORIENTED_EDGE ( 'NONE', *, *, #21113, .T. ) ;
#3712 = CARTESIAN_POINT ( 'NONE',  ( -28.75808802781983076, 35.61482992978302775, -18.59445401971593270 ) ) ;
#3713 = CARTESIAN_POINT ( 'NONE',  ( 151.7948205124836250, 33.23291073765556547, 0.000000000000000000 ) ) ;
#3714 = CARTESIAN_POINT ( 'NONE',  ( -193.0908541284702551, 48.38978395451683667, -14.03723495791108533 ) ) ;
#3715 = APPLICATION_PROTOCOL_DEFINITION ( 'draft international standard', 'automotive_design', 1998, #2056 ) ;
#3716 = ORIENTED_EDGE ( 'NONE', *, *, #5638, .F. ) ;
#3717 = EDGE_LOOP ( 'NONE', ( #394, #9608, #568, #16105 ) ) ;
#3718 = CARTESIAN_POINT ( 'NONE',  ( -259.2033419157646676, -21.55415060305824326, -35.01439189186556433 ) ) ;
#3719 = CARTESIAN_POINT ( 'NONE',  ( 37.37129771728702821, -41.71823991396121301, -12.75330473327949576 ) ) ;
#3720 = ORIENTED_EDGE ( 'NONE', *, *, #1194, .T. ) ;
#3721 = CARTESIAN_POINT ( 'NONE',  ( 14.38125909742180752, 55.17850393971008316, -40.00000000000002132 ) ) ;
#3722 = CARTESIAN_POINT ( 'NONE',  ( -210.0000000000000284, 69.29737539576900929, -75.30386416458597409 ) ) ;
#3723 = VERTEX_POINT ( 'NONE', #7849 ) ;
#3724 = CARTESIAN_POINT ( 'NONE',  ( 199.9999999999998863, 18.69362872516077800, 3.425107952296777114 ) ) ;
#3725 = CARTESIAN_POINT ( 'NONE',  ( -200.0000000000000000, -66.50000000000001421, 66.50000000000005684 ) ) ;
#3726 = CARTESIAN_POINT ( 'NONE',  ( -208.1127848780265026, 38.89260858015724409, 38.89260858015741462 ) ) ;
#3727 = CARTESIAN_POINT ( 'NONE',  ( -188.8753834511964840, -43.29882472894603751, -17.93496043754511859 ) ) ;
#3728 = CARTESIAN_POINT ( 'NONE',  ( 19.06497207195981147, -4.605042221739098431E-14, 14.19242893257840521 ) ) ;
#3729 = CARTESIAN_POINT ( 'NONE',  ( 184.8905102610680444, -20.92133201514440799, 0.000000000000000000 ) ) ;
#3730 = CARTESIAN_POINT ( 'NONE',  ( 57.59792236341147031, 26.56190807104720975, -26.56190807104655249 ) ) ;
#3731 = CARTESIAN_POINT ( 'NONE',  ( -211.2619052429883482, 0.000000000000000000, 0.000000000000000000 ) ) ;
#3732 = CARTESIAN_POINT ( 'NONE',  ( -162.0762913951021176, -40.00000000000005684, 1.694272876828184504 ) ) ;
#3733 = CARTESIAN_POINT ( 'NONE',  ( -100.7734535825088358, -2.560096224687585342E-13, 22.67402823373191723 ) ) ;
#3734 = CARTESIAN_POINT ( 'NONE',  ( -114.6297772182897319, -11.19545617568720886, 18.93772329700642842 ) ) ;
#3735 = CARTESIAN_POINT ( 'NONE',  ( -100.7734535825088358, -12.25131212657493052, 12.25131212657478130 ) ) ;
#3736 = CARTESIAN_POINT ( 'NONE',  ( 0.2972598230769983307, -14.33493731733933352, -40.00000000000002132 ) ) ;
#3737 = CARTESIAN_POINT ( 'NONE',  ( -91.56559293963834989, -40.53558337403669753, -16.03295912088728770 ) ) ;
#3738 = DIRECTION ( 'NONE',  ( 0.000000000000000000, 0.000000000000000000, 1.000000000000000000 ) ) ;
#3739 = FACE_BOUND ( 'NONE', #14612, .T. ) ;
#3740 = CARTESIAN_POINT ( 'NONE',  ( -238.4067589809705794, 39.99999999999999289, -0.9644942799821634161 ) ) ;
#3741 = CARTESIAN_POINT ( 'NONE',  ( -91.56559293963834989, 6.234561990864368500E-14, -22.67402823373191723 ) ) ;
#3742 = CARTESIAN_POINT ( 'NONE',  ( 0.2972598230769959993, 38.42060263243659080, 38.42060263243672580 ) ) ;
#3743 = CARTESIAN_POINT ( 'NONE',  ( -114.7816107152219729, 16.24027016579831795, 15.05025810000610420 ) ) ;
#3744 = CARTESIAN_POINT ( 'NONE',  ( -188.6013942375869590, -13.84412886956378586, -47.09843442133011138 ) ) ;
#3745 = DIRECTION ( 'NONE',  ( 0.000000000000000000, 0.000000000000000000, -1.000000000000000000 ) ) ;
#3746 = VERTEX_POINT ( 'NONE', #11987 ) ;
#3747 = CARTESIAN_POINT ( 'NONE',  ( -100.7734535825088500, -44.31723036834885932, -12.25131212657538171 ) ) ;
#3748 = CARTESIAN_POINT ( 'NONE',  ( 170.2234770963711128, 17.36149277827004411, -17.36149277826983095 ) ) ;
#3749 = CARTESIAN_POINT ( 'NONE',  ( 151.7948205124836250, 33.23291073765556547, 0.000000000000000000 ) ) ;
#3750 = LINE ( 'NONE', #24103, #17009 ) ;
#3751 = CARTESIAN_POINT ( 'NONE',  ( 146.6084372240433709, -52.76785682606510619, -3.800685668859292043 ) ) ;
#3752 = CARTESIAN_POINT ( 'NONE',  ( -200.5022929845069939, -18.58571294254629436, -44.86988025226661847 ) ) ;
#3753 = CARTESIAN_POINT ( 'NONE',  ( -93.12335834970892279, 22.67402823373189946, -0.000000000000000000 ) ) ;
#3754 = ORIENTED_EDGE ( 'NONE', *, *, #8329, .T. ) ;
#3755 = CARTESIAN_POINT ( 'NONE',  ( 199.9999999999999716, 18.51141176942600097, 4.336711825884415283 ) ) ;
#3756 = CARTESIAN_POINT ( 'NONE',  ( -4.039451493210483690, -23.44932283416618191, -43.00522595894033628 ) ) ;
#3757 = CARTESIAN_POINT ( 'NONE',  ( -4.260882601034492900, 23.40615483283669818, 42.93997571557765269 ) ) ;
#3758 = ORIENTED_EDGE ( 'NONE', *, *, #13522, .T. ) ;
#3759 = ORIENTED_EDGE ( 'NONE', *, *, #19081, .F. ) ;
#3760 = CARTESIAN_POINT ( 'NONE',  ( -30.26275506840324070, 1.198031551616013601, 1.198031551616023371 ) ) ;
#3761 = CARTESIAN_POINT ( 'NONE',  ( 199.0074854128475579, 2.768696461275208520, -19.80384161416936806 ) ) ;
#3762 = CARTESIAN_POINT ( 'NONE',  ( -110.0368417077424539, -7.441767003010021142, -18.74474319002755252 ) ) ;
#3763 = CARTESIAN_POINT ( 'NONE',  ( -89.91498783729113597, -20.43892340019855780, -8.087768383230207192 ) ) ;
#3764 = AXIS2_PLACEMENT_3D ( 'NONE', #15560, #13566, #13698 ) ;
#3765 = ADVANCED_FACE ( 'NONE', ( #14118 ), #5143, .T. ) ;
#3766 = CARTESIAN_POINT ( 'NONE',  ( -135.8532207217289738, 21.81201906317798134, -21.81201906317747685 ) ) ;
#3767 = CARTESIAN_POINT ( 'NONE',  ( 91.82158438592158234, -1.633484621919921769E-13, 17.20528682183300262 ) ) ;
#3768 = CARTESIAN_POINT ( 'NONE',  ( 200.0000000000001705, -18.10265802883496278, 5.810802590798905598 ) ) ;
#3769 = CARTESIAN_POINT ( 'NONE',  ( -82.24286375075958233, -20.07657133907689939, -2.516278881350180630 ) ) ;
#3770 = PLANE ( 'NONE',  #13222 ) ;
#3771 = CARTESIAN_POINT ( 'NONE',  ( 199.0206025836015442, 6.413712542583970944, 18.94893284924772203 ) ) ;
#3772 = FACE_OUTER_BOUND ( 'NONE', #17773, .T. ) ;
#3773 = CARTESIAN_POINT ( 'NONE',  ( -1.087763065866631962, -13.97201973055225466, -47.95583523904139156 ) ) ;
#3774 = EDGE_CURVE ( 'NONE', #433, #4824, #19279, .T. ) ;
#3775 = CARTESIAN_POINT ( 'NONE',  ( 199.9999999999999432, -14.14213562373073607, -14.14213562373102206 ) ) ;
#3776 = CARTESIAN_POINT ( 'NONE',  ( -105.4741150117398263, -19.77569912953930498, 7.943527260776862775 ) ) ;
#3777 = CARTESIAN_POINT ( 'NONE',  ( -213.1075012329537230, -66.26714140138676612, 9.698598906462487790 ) ) ;
#3778 = CARTESIAN_POINT ( 'NONE',  ( -100.7734535825088500, -40.00000000000027711, 22.67402823373149801 ) ) ;
#3779 = CARTESIAN_POINT ( 'NONE',  ( -100.7734535825088500, 16.03295912088691821, 16.03295912088721309 ) ) ;
#3780 = CARTESIAN_POINT ( 'NONE',  ( 57.59792236341148453, -37.56421063658185489, 40.00000000000002132 ) ) ;
#3781 = EDGE_CURVE ( 'NONE', #1564, #16348, #23216, .T. ) ;
#3782 = EDGE_CURVE ( 'NONE', #23489, #14320, #20718, .T. ) ;
#3783 = CARTESIAN_POINT ( 'NONE',  ( -280.0000000000000000, 14.14213562373098299, -14.14213562373088706 ) ) ;
#3784 = CARTESIAN_POINT ( 'NONE',  ( 170.2234770963711128, -15.44714144992812699, -40.00000000000002132 ) ) ;
#3785 = CARTESIAN_POINT ( 'NONE',  ( -105.2136831797469654, 16.29138911077802021, 14.02836134671350266 ) ) ;
#3786 = CARTESIAN_POINT ( 'NONE',  ( 199.9999999999999432, -1.727494763561684666E-13, 20.00000000000010303 ) ) ;
#3787 = CARTESIAN_POINT ( 'NONE',  ( -105.3755690713226585, 12.89780903124410472, -43.67073346367977393 ) ) ;
#3788 = CARTESIAN_POINT ( 'NONE',  ( -238.4067589809705794, 0.9644942799825385604, -40.00000000000002132 ) ) ;
#3790 = ORIENTED_EDGE ( 'NONE', *, *, #7999, .T. ) ;
#3789 = AXIS2_PLACEMENT_3D ( 'NONE', #16859, #22989, #21124 ) ;
#3791 = CARTESIAN_POINT ( 'NONE',  ( 22.82148508083520966, -43.16138278736967493, 17.87803012130510183 ) ) ;
#3792 = AXIS2_PLACEMENT_3D ( 'NONE', #2489, #4365, #14585 ) ;
#3793 = SPHERICAL_SURFACE ( 'NONE', #11934, 15.00000000000000000 ) ;
#3794 = CARTESIAN_POINT ( 'NONE',  ( -238.4067589809705794, 57.25054294077225592, 0.6820004458485544596 ) ) ;
#3795 = CARTESIAN_POINT ( 'NONE',  ( -198.0356074513804572, -40.00000000000025580, 55.37879056871310013 ) ) ;
#3796 = CARTESIAN_POINT ( 'NONE',  ( -56.48582580120559271, -6.472252184284276844, 6.472252184284108978 ) ) ;
#3797 = DIRECTION ( 'NONE',  ( -1.000000000000000000, -1.836970198721030181E-16, -0.000000000000000000 ) ) ;
#3798 = CARTESIAN_POINT ( 'NONE',  ( 146.6084372240433709, 5.374981219217002781, -40.00000000000002132 ) ) ;
#3799 = EDGE_CURVE ( 'NONE', #8569, #2955, #7293, .T. ) ;
#3800 = PRODUCT ( 'Pump housing', 'Pump housing', '', ( #2118 ) ) ;
#3801 = CARTESIAN_POINT ( 'NONE',  ( -626.9846540392142060, 75.00000000000000000, 0.000000000000000000 ) ) ;
#3802 = CARTESIAN_POINT ( 'NONE',  ( 199.9999999999999716, 18.70067531203203970, -3.379044910449504169 ) ) ;
#3803 = CARTESIAN_POINT ( 'NONE',  ( 200.0000000000000000, -13.65901895451712811, -13.21854774209566585 ) ) ;
#3804 = CARTESIAN_POINT ( 'NONE',  ( -30.26275506840323715, 29.48230279907829754, -29.48230279907758344 ) ) ;
#3805 = CARTESIAN_POINT ( 'NONE',  ( 192.4448373802100889, -14.14213562370293431, -14.14213562370322030 ) ) ;
#3806 = CARTESIAN_POINT ( 'NONE',  ( -105.2468259004641595, 21.22367899003718961, -3.281783220163879911 ) ) ;
#3807 = CARTESIAN_POINT ( 'NONE',  ( -77.58512834295702021, 17.50146741020782315, -13.57440574225726770 ) ) ;
#3808 = CARTESIAN_POINT ( 'NONE',  ( 91.82158438592156813, -16.11829626348459144, 40.45024623143943643 ) ) ;
#3810 = CARTESIAN_POINT ( 'NONE',  ( -4.039451493210489019, 13.82811171175440812, 46.99046209229809534 ) ) ;
#3809 = CARTESIAN_POINT ( 'NONE',  ( 163.1118516004056573, -9.006482792069506971, -9.006482792069697041 ) ) ;
#3811 = CARTESIAN_POINT ( 'NONE',  ( -208.1127848780264742, -17.67593391476605547, -38.89260858015755673 ) ) ;
#3812 = ADVANCED_FACE ( 'NONE', ( #15407 ), #23532, .T. ) ;
#3813 = DIRECTION ( 'NONE',  ( 1.000000000000000000, 1.836970198721030427E-16, -0.000000000000000000 ) ) ;
#3814 = CARTESIAN_POINT ( 'NONE',  ( 199.0150730930814689, 15.28768747664870453, 12.90128171110900013 ) ) ;
#3815 = AXIS2_PLACEMENT_3D ( 'NONE', #10264, #153, #12651 ) ;
#3817 = CARTESIAN_POINT ( 'NONE',  ( -213.1075012329537230, -40.00000000000025580, 53.71589010953650956 ) ) ;
#3816 = CARTESIAN_POINT ( 'NONE',  ( -105.3755690713226585, 41.18208027870575449, 15.38646221621837107 ) ) ;
#3818 = CARTESIAN_POINT ( 'NONE',  ( -238.4067589809705794, -0.6820004457913680929, 0.6820004457913170226 ) ) ;
#3819 = CARTESIAN_POINT ( 'NONE',  ( 130.8568914410475372, 24.07718906447210472, 24.07718906447249907 ) ) ;
#3820 = CARTESIAN_POINT ( 'NONE',  ( 19.06497207195980792, 54.19242893257844429, 40.00000000000002132 ) ) ;
#3821 = ORIENTED_EDGE ( 'NONE', *, *, #7653, .T. ) ;
#3822 = CARTESIAN_POINT ( 'NONE',  ( 163.1118516004056573, -19.27778845538761132, -19.27778845538770724 ) ) ;
#3823 = B_SPLINE_CURVE_WITH_KNOTS ( 'NONE', 3,
 ( #22877, #4654, #25655, #11276, #1181, #9154, #23144, #5047 ),
 .UNSPECIFIED., .F., .F.,
 ( 4, 2, 2, 4 ),
 ( 0.008471746898050105251, 0.01057975003289800958, 0.01268775316774591218, 0.01690375943744171564 ),
 .UNSPECIFIED. ) ;
#3824 = CARTESIAN_POINT ( 'NONE',  ( 190.0000000000000000, 66.50000000000009948, 66.50000000000005684 ) ) ;
#3825 = CARTESIAN_POINT ( 'NONE',  ( 83.01683444506757326, 9.947410331246418380, 24.01517293248988594 ) ) ;
#3826 = VERTEX_POINT ( 'NONE', #13413 ) ;
#3827 = CARTESIAN_POINT ( 'NONE',  ( -197.6434631108370752, -44.74794079766468258, 18.53520396667546066 ) ) ;
#3828 = VECTOR ( 'NONE', #6939, 1000.000000000000000 ) ;
#3829 = CARTESIAN_POINT ( 'NONE',  ( 199.9999999999999716, -18.76480772196043034, -3.095184993347289026 ) ) ;
#3830 = CARTESIAN_POINT ( 'NONE',  ( 13.28449813595630680, -24.75673736219087928, 44.77439867188066813 ) ) ;
#3831 = CARTESIAN_POINT ( 'NONE',  ( 17.49521241101495406, 18.35049639060493121, -44.30201726252816741 ) ) ;
#3832 = CARTESIAN_POINT ( 'NONE',  ( 199.0093721751683518, -2.288394243462712030, -19.86801947894618792 ) ) ;
#3833 = CARTESIAN_POINT ( 'NONE',  ( 147.2817042152899205, -29.82799917201331752, 12.35516179550115545 ) ) ;
#3834 = DIRECTION ( 'NONE',  ( 0.000000000000000000, 1.000000000000000000, 0.000000000000000000 ) ) ;
#3835 = CARTESIAN_POINT ( 'NONE',  ( 170.2234770963711128, 39.20704971665372796, 17.36149277827039583 ) ) ;
#3836 = CARTESIAN_POINT ( 'NONE',  ( 91.82158438592159655, -22.79471317813468545, -2.449293598294708485E-15 ) ) ;
#3838 = CARTESIAN_POINT ( 'NONE',  ( 200.0000000000000000, 3.673940397442060756E-14, 0.000000000000000000 ) ) ;
#3837 = CARTESIAN_POINT ( 'NONE',  ( -210.0000000000000284, 52.49999999999987210, 82.49999999999998579 ) ) ;
#3839 = CARTESIAN_POINT ( 'NONE',  ( 98.29820294268675696, -5.307337294603860833, -19.44947291833535274 ) ) ;
#3840 = CARTESIAN_POINT ( 'NONE',  ( 4.995406935893293543, -15.24977328854832592, 0.000000000000000000 ) ) ;
#3841 = CARTESIAN_POINT ( 'NONE',  ( -213.1075012329537230, 13.71589010951907994, 0.000000000000000000 ) ) ;
#3842 = CARTESIAN_POINT ( 'NONE',  ( 192.4448373802101173, 40.00000000000026290, -19.99999999996018474 ) ) ;
#3843 = CARTESIAN_POINT ( 'NONE',  ( 163.1118516004056573, 9.006482792069629539, 9.006482792069634868 ) ) ;
#3844 = CARTESIAN_POINT ( 'NONE',  ( -259.2033419157646676, -1.473088368616265084E-13, 9.517827891722632216 ) ) ;
#3845 = CARTESIAN_POINT ( 'NONE',  ( -100.7734535825088500, 16.03295912088691821, 16.03295912088721309 ) ) ;
#3846 = ORIENTED_EDGE ( 'NONE', *, *, #26147, .F. ) ;
#3847 = CARTESIAN_POINT ( 'NONE',  ( -86.86493150571116928, 19.77569912839177846, -7.943527260495974573 ) ) ;
#3848 = CARTESIAN_POINT ( 'NONE',  ( -200.0000000000000000, 52.50000000000007816, -52.49999999999999289 ) ) ;
#3849 = CIRCLE ( 'NONE', #7183, 5.000000000000004441 ) ;
#3850 = CARTESIAN_POINT ( 'NONE',  ( -189.2428547182110776, 47.31876910929169355, -13.87687415872436070 ) ) ;
#3851 = APPLICATION_PROTOCOL_DEFINITION ( 'draft international standard', 'automotive_design', 1998, #16139 ) ;
#3852 = ORIENTED_EDGE ( 'NONE', *, *, #15330, .T. ) ;
#3853 = ORIENTED_EDGE ( 'NONE', *, *, #3071, .T. ) ;
#3854 = CARTESIAN_POINT ( 'NONE',  ( 200.0000000000000000, -14.14213562373062949, -42.42640687119301646 ) ) ;
#3855 = CARTESIAN_POINT ( 'NONE',  ( 22.72611120194082446, -43.18769924474469946, -17.88893075486395645 ) ) ;
#3856 = VERTEX_POINT ( 'NONE', #7413 ) ;
#3857 = CARTESIAN_POINT ( 'NONE',  ( -100.7734535825088500, 17.32597176626809699, -40.00000000000002132 ) ) ;
#3858 = CARTESIAN_POINT ( 'NONE',  ( -89.91498783728933120, -20.43892340021436738, 8.087768383194113397 ) ) ;
#3859 = ORIENTED_EDGE ( 'NONE', *, *, #17434, .F. ) ;
#3860 = CARTESIAN_POINT ( 'NONE',  ( 200.0000000000000568, 5.208214048020466613, 18.28294570233482119 ) ) ;
#3861 = CARTESIAN_POINT ( 'NONE',  ( -83.21262154144251610, -13.72187187061454949, -33.12752917118435647 ) ) ;
#3862 = EDGE_CURVE ( 'NONE', #19937, #8803, #7875, .T. ) ;
#3863 = CARTESIAN_POINT ( 'NONE',  ( -280.0000000000000568, 14.14213562373097943, -42.42640687119285303 ) ) ;
#3864 = CARTESIAN_POINT ( 'NONE',  ( -183.1091233172472812, -41.47045062399658377, -22.43565125812520122 ) ) ;
#3865 = CARTESIAN_POINT ( 'NONE',  ( 146.6084372240433709, -39.99999999999987921, -34.62501878078319351 ) ) ;
#3866 = PRODUCT_RELATED_PRODUCT_CATEGORY ( 'part', '', ( #3800 ) ) ;
#3867 = CARTESIAN_POINT ( 'NONE',  ( -100.7734535825088500, 17.32597176626808988, 40.00000000000002132 ) ) ;
#3868 = CARTESIAN_POINT ( 'NONE',  ( -238.4067589809705794, 0.6820004458491113475, -57.25054294077229144 ) ) ;
#3869 = CARTESIAN_POINT ( 'NONE',  ( 199.0251223662492635, -5.665586242881555101, 19.18612710904600149 ) ) ;
#3870 = VECTOR ( 'NONE', #23818, 1000.000000000000000 ) ;
#3871 = CARTESIAN_POINT ( 'NONE',  ( 146.6084372240433709, -39.99999999999987921, -34.62501878078319351 ) ) ;
#3872 = CARTESIAN_POINT ( 'NONE',  ( 136.1360204305621551, -39.99999999999994316, -4.966164525587488221 ) ) ;
#3873 = CARTESIAN_POINT ( 'NONE',  ( -110.0563856373150315, -9.155970533462395977, 17.99047586674176458 ) ) ;
#3874 = CARTESIAN_POINT ( 'NONE',  ( -105.3755690713226727, -12.89780903124413847, 12.89780903124398037 ) ) ;
#3875 = CARTESIAN_POINT ( 'NONE',  ( 4.995406935893293543, -15.24977328854832592, 0.000000000000000000 ) ) ;
#3876 = EDGE_CURVE ( 'NONE', #9443, #22454, #1446, .T. ) ;
#3877 = CARTESIAN_POINT ( 'NONE',  ( -30.26275506840322294, -57.76657404653985139, 1.198031551615709844 ) ) ;
#3878 = CARTESIAN_POINT ( 'NONE',  ( -626.9846540392142060, 75.00000000000000000, 74.99999999999991473 ) ) ;
#3879 = ADVANCED_FACE ( 'NONE', ( #21791, #7802 ), #23912, .T. ) ;
#3880 = LINE ( 'NONE', #11980, #5565 ) ;
#3881 = CARTESIAN_POINT ( 'NONE',  ( -198.0356074513804572, 1.247057299367198800E-13, -15.37879056873070560 ) ) ;
#3882 = CARTESIAN_POINT ( 'NONE',  ( -208.1127848780264742, -40.00000000000011369, 15.00245453012655439 ) ) ;
#3883 = CARTESIAN_POINT ( 'NONE',  ( -105.3755690713226585, 12.89780903124410472, -43.67073346367977393 ) ) ;
#3884 = CARTESIAN_POINT ( 'NONE',  ( 192.4448373802100889, 14.14213562375873678, 14.14213562375894817 ) ) ;
#3885 = CARTESIAN_POINT ( 'NONE',  ( -188.6013942376020793, -23.51434495930271851, -43.09289976588667770 ) ) ;
#3886 = VECTOR ( 'NONE', #1019, 1000.000000000000000 ) ;
#3887 = CARTESIAN_POINT ( 'NONE',  ( -198.0356074513804572, -10.87444709759729911, 10.87444709759714812 ) ) ;
#3888 = ORIENTED_EDGE ( 'NONE', *, *, #19870, .T. ) ;
#3889 = CARTESIAN_POINT ( 'NONE',  ( -135.8532207217289738, -6.472252184284280396, 6.472252184284099208 ) ) ;
#3890 = LINE ( 'NONE', #8129, #4264 ) ;
#3891 = CARTESIAN_POINT ( 'NONE',  ( 163.1118516004056573, 47.56205970284957374, 9.006482792074494981 ) ) ;
#3892 = LINE ( 'NONE', #5738, #13231 ) ;
#3893 = FILL_AREA_STYLE_COLOUR ( '', #23380 ) ;
#3894 = CARTESIAN_POINT ( 'NONE',  ( 163.1118516004056573, -19.27778845539181063, -37.29075403953176959 ) ) ;
#3895 = B_SPLINE_CURVE_WITH_KNOTS ( 'NONE', 3,
 ( #8163, #26143, #20544, #12286, #18540, #18136, #8423, #8024, #24673, #20414 ),
 .UNSPECIFIED., .F., .F.,
 ( 4, 2, 2, 2, 4 ),
 ( 0.7921542097164072649, 0.8508620842112317728, 0.8814014469398914198, 0.9119408096685510667, 0.9406682828396428775 ),
 .UNSPECIFIED. ) ;
#3896 = CARTESIAN_POINT ( 'NONE',  ( 35.93739780878637902, -38.99308239425781863, 20.78453051019726772 ) ) ;
#3897 = VERTEX_POINT ( 'NONE', #1578 ) ;
#3898 = CIRCLE ( 'NONE', #17049, 5.000000000000004441 ) ;
#3899 = CARTESIAN_POINT ( 'NONE',  ( 199.9999999999999716, 18.84369875136934880, -2.460375794728051790 ) ) ;
#3900 = LINE ( 'NONE', #20389, #10244 ) ;
#3901 = CARTESIAN_POINT ( 'NONE',  ( 1.925538622596562277, 24.44644315487925113, 44.35335385591492496 ) ) ;
#3902 = AXIS2_PLACEMENT_3D ( 'NONE', #12330, #10210, #20458 ) ;
#3903 = ORIENTED_EDGE ( 'NONE', *, *, #22166, .F. ) ;
#3904 = ORIENTED_EDGE ( 'NONE', *, *, #8481, .F. ) ;
#3905 = FACE_OUTER_BOUND ( 'NONE', #15425, .T. ) ;
#3906 = CARTESIAN_POINT ( 'NONE',  ( 199.0059208051008852, 8.690306674284110855, -18.00847358856242408 ) ) ;
#3907 = CARTESIAN_POINT ( 'NONE',  ( -114.7544846451821030, -2.764907549246811591, -21.97700197333382377 ) ) ;
#3908 = CARTESIAN_POINT ( 'NONE',  ( -109.0492076899303555, -25.45044590702468668, -25.45044590702569565 ) ) ;
#3909 = CARTESIAN_POINT ( 'NONE',  ( -726.9846540392142060, 66.50000000000009948, 71.50000000000005684 ) ) ;
#3910 = CARTESIAN_POINT ( 'NONE',  ( 14.38125909742181108, 1.616281842095393922E-13, -15.17850393972633682 ) ) ;
#3911 = CARTESIAN_POINT ( 'NONE',  ( -678.9461782662772293, 75.00000000000000000, 30.00000000000158096 ) ) ;
#3912 = CARTESIAN_POINT ( 'NONE',  ( -77.58456329405633767, -21.97699521662486077, -2.764787398945805386 ) ) ;
#3913 = AXIS2_PLACEMENT_3D ( 'NONE', #9877, #299, #22401 ) ;
#3914 = CARTESIAN_POINT ( 'NONE',  ( -317.0000000000000568, -4.857225732735059864E-14, 0.000000000000000000 ) ) ;
#3915 = CARTESIAN_POINT ( 'NONE',  ( 199.0173417939125784, 12.16728005963107329, 15.88742495833056800 ) ) ;
#3916 = CARTESIAN_POINT ( 'NONE',  ( -142.4595961066947041, 29.46485439465666900, 12.20474230359199908 ) ) ;
#3917 = CARTESIAN_POINT ( 'NONE',  ( -3.675706741948236100, -17.91131112508005074, -43.24173023805411731 ) ) ;
#3918 = CARTESIAN_POINT ( 'NONE',  ( 200.0000000000000000, 14.14213562373142352, -42.42640687119268961 ) ) ;
#3919 = CARTESIAN_POINT ( 'NONE',  ( -110.0574659385135305, 6.253952508993774195, -19.22572883246642306 ) ) ;
#3920 = CARTESIAN_POINT ( 'NONE',  ( -105.3755690713226727, -12.89780903124413847, 12.89780903124398037 ) ) ;
#3921 = CARTESIAN_POINT ( 'NONE',  ( 4.995406935893290878, 1.606505379428369110E-13, -15.24977328854832592 ) ) ;
#3922 = CARTESIAN_POINT ( 'NONE',  ( 199.9999999999999432, 20.00000000000013856, 0.000000000000000000 ) ) ;
#3923 =( REPRESENTATION_RELATIONSHIP ('NONE','NONE', #23888, #21040 ) REPRESENTATION_RELATIONSHIP_WITH_TRANSFORMATION ( #4518 )SHAPE_REPRESENTATION_RELATIONSHIP( ) );
#3924 = CARTESIAN_POINT ( 'NONE',  ( 170.2234770963711128, -15.44714144992813409, 40.00000000000002132 ) ) ;
#3925 = CARTESIAN_POINT ( 'NONE',  ( 150.0000000000000284, -125.7889608577475116, 82.50000000000001421 ) ) ;
#3926 = CARTESIAN_POINT ( 'NONE',  ( 170.2234770963711128, -15.44714144992812876, -2.449293598294708485E-15 ) ) ;
#3927 = CARTESIAN_POINT ( 'NONE',  ( -114.7581397844644187, 13.68781109932255546, 17.42046360869897725 ) ) ;
#3928 = CARTESIAN_POINT ( 'NONE',  ( 136.1360204305621551, 40.00000000000009948, -4.966164525586641787 ) ) ;
#3929 = CARTESIAN_POINT ( 'NONE',  ( 184.8905102610680444, 41.77492675556005253, -14.79361573936377461 ) ) ;
#3930 = CARTESIAN_POINT ( 'NONE',  ( -135.8532207217289738, -9.153146818113595984, 0.000000000000000000 ) ) ;
#3931 = VERTEX_POINT ( 'NONE', #11667 ) ;
#3932 = ADVANCED_FACE ( 'NONE', ( #11290 ), #20441, .T. ) ;
#3933 = CARTESIAN_POINT ( 'NONE',  ( -259.2033419157646676, -9.517827891722680178, 0.000000000000000000 ) ) ;
#3934 = AXIS2_PLACEMENT_3D ( 'NONE', #26310, #8318, #10455 ) ;
#3935 = CARTESIAN_POINT ( 'NONE',  ( -65.65510974524491417, -9.107311025939104354, 24.89665924127723784 ) ) ;
#3936 = CARTESIAN_POINT ( 'NONE',  ( 184.8905102610680444, 41.77492675556005253, -14.79361573936377461 ) ) ;
#3937 = CARTESIAN_POINT ( 'NONE',  ( -280.0000000000000568, -40.00000000000014211, 19.99999999999987210 ) ) ;
#3938 = CARTESIAN_POINT ( 'NONE',  ( 14.38125909742180220, 39.01709431150892016, 17.55144818341517166 ) ) ;
#3939 = CARTESIAN_POINT ( 'NONE',  ( 4.995406935893288214, 15.24977328854832770, 0.000000000000000000 ) ) ;
#3940 = DIRECTION ( 'NONE',  ( 0.000000000000000000, 0.000000000000000000, -1.000000000000000000 ) ) ;
#3941 = CARTESIAN_POINT ( 'NONE',  ( 199.9999999999999432, 18.93973332185608172, 1.567235916626209535 ) ) ;
#3942 = CARTESIAN_POINT ( 'NONE',  ( 199.9999999999999716, -16.61824216245382502, -9.229554904678261451 ) ) ;
#3943 = CARTESIAN_POINT ( 'NONE',  ( -192.9588430854690273, 66.79921049724377724, -10.23066800231904239 ) ) ;
#3944 = CARTESIAN_POINT ( 'NONE',  ( 170.2234770963711128, -39.20704971665404059, 17.36149277826957160 ) ) ;
#3945 = CARTESIAN_POINT ( 'NONE',  ( -105.4536606934774738, 19.90286765811677228, 7.687677726850456139 ) ) ;
#3946 = CARTESIAN_POINT ( 'NONE',  ( -238.4067589809705794, -3.369206980223063916E-14, -0.9644942799825824142 ) ) ;
#3947 = CARTESIAN_POINT ( 'NONE',  ( -208.1127848780264742, -38.89260858015753541, 17.67593391476614784 ) ) ;
#3948 = CARTESIAN_POINT ( 'NONE',  ( -105.3755690713226727, -15.38646221621807619, 15.38646221621768362 ) ) ;
#3949 = CARTESIAN_POINT ( 'NONE',  ( -198.0356074513804572, -17.40982414986427429, -39.15871834505933435 ) ) ;
#3950 = CARTESIAN_POINT ( 'NONE',  ( 170.2234770963711128, -10.92277846919171935, -45.64576402573189995 ) ) ;
#3951 = CARTESIAN_POINT ( 'NONE',  ( 199.0221514193071926, 3.032938341077176414, 19.78261031040590012 ) ) ;
#3953 = CARTESIAN_POINT ( 'NONE',  ( 184.8905102610680444, 1.070102760522089011E-13, -20.92133201514444352 ) ) ;
#3952 = CARTESIAN_POINT ( 'NONE',  ( 4.995406935893290878, 39.06748935135239265, -39.06748935135144762 ) ) ;
#3954 = CARTESIAN_POINT ( 'NONE',  ( -135.8532207217289738, 6.472252184284096543, 6.472252184284234211 ) ) ;
#3955 = CARTESIAN_POINT ( 'NONE',  ( 11.38508063394172609, 44.88728980639542243, -24.83994849155190821 ) ) ;
#3956 = CARTESIAN_POINT ( 'NONE',  ( 163.1118516004056573, 12.73709011382478273, 2.449293598294708485E-15 ) ) ;
#3957 = EDGE_LOOP ( 'NONE', ( #25081, #3495, #786, #25524, #5205, #9062, #4826, #21169 ) ) ;
#3958 = CARTESIAN_POINT ( 'NONE',  ( -280.0000000000000000, -20.00000000000006750, 0.000000000000000000 ) ) ;
#3959 = EDGE_CURVE ( 'NONE', #14912, #15079, #21981, .T. ) ;
#3960 = CARTESIAN_POINT ( 'NONE',  ( 25.86856017011190900, 41.48891248390243902, 17.18527023894284156 ) ) ;
#3961 = LINE ( 'NONE', #16045, #2220 ) ;
#3962 = CARTESIAN_POINT ( 'NONE',  ( 170.2234770963711128, -24.55285855007183926, 0.000000000000000000 ) ) ;
#3963 = ADVANCED_FACE ( 'NONE', ( #3410 ), #25771, .F. ) ;
#3964 = EDGE_LOOP ( 'NONE', ( #23997, #7152, #21523, #24412 ) ) ;
#3965 = CARTESIAN_POINT ( 'NONE',  ( -188.6889827002315769, -43.11787295909560669, 23.53286111060863561 ) ) ;
#3966 = CARTESIAN_POINT ( 'NONE',  ( 199.9999999999998579, -18.00099009291985297, -6.105420735363839668 ) ) ;
#3967 = CARTESIAN_POINT ( 'NONE',  ( -0.6848998193154250957, -13.98809697771007343, 48.06291537634446343 ) ) ;
#3968 = ADVANCED_FACE ( 'NONE', ( #25902 ), #20039, .T. ) ;
#3969 = EDGE_CURVE ( 'NONE', #17794, #23789, #17238, .T. ) ;
#3970 = CARTESIAN_POINT ( 'NONE',  ( 25.88393124175084026, 13.61573025394702974, -45.90075965688677684 ) ) ;
#3971 = CARTESIAN_POINT ( 'NONE',  ( 199.0198127172867828, -18.35326955327933618, -7.958687714023728432 ) ) ;
#3972 = CYLINDRICAL_SURFACE ( 'NONE', #11313, 5.000000000000004441 ) ;
#3973 = CARTESIAN_POINT ( 'NONE',  ( -151.7004448981651024, -13.46262099556660097, 32.50164219284836520 ) ) ;
#3974 = CARTESIAN_POINT ( 'NONE',  ( -208.1127848780265026, 38.89260858015777700, -38.89260858015687461 ) ) ;
#3975 = CARTESIAN_POINT ( 'NONE',  ( 170.2234770963711128, 24.55285855007190676, 40.00000000000002132 ) ) ;
#3977 = CARTESIAN_POINT ( 'NONE',  ( -86.96347745069644475, -15.38646221621807442, 15.38646221621768184 ) ) ;
#3976 = CARTESIAN_POINT ( 'NONE',  ( -192.9370379451515873, 24.26711011076366376, -44.11033005022372322 ) ) ;
#3978 = CARTESIAN_POINT ( 'NONE',  ( 98.29820294267474878, -15.06873823043769534, -13.21553301703162298 ) ) ;
#3979 = CARTESIAN_POINT ( 'NONE',  ( 146.6084372240433993, 34.62501878078308692, 0.000000000000000000 ) ) ;
#3980 = CARTESIAN_POINT ( 'NONE',  ( 14.38125909742180752, 55.17850393972636880, 2.449293598294708485E-15 ) ) ;
#3981 = CARTESIAN_POINT ( 'NONE',  ( -91.56559293963834989, -39.99999999999985789, -17.32597176626853042 ) ) ;
#3982 = CARTESIAN_POINT ( 'NONE',  ( -208.1127848780265026, 38.89260858015724409, 38.89260858015741462 ) ) ;
#3983 = CARTESIAN_POINT ( 'NONE',  ( -190.0000000000000000, 82.50000000000008527, 52.49999999999979394 ) ) ;
#3984 = CARTESIAN_POINT ( 'NONE',  ( -259.2033419157646676, 35.01439189186559275, -21.55415060305807984 ) ) ;
#3985 = ORIENTED_EDGE ( 'NONE', *, *, #21595, .F. ) ;
#3986 = CARTESIAN_POINT ( 'NONE',  ( 163.1118516004056573, -47.56205970284957374, 9.006482792074162802 ) ) ;
#3987 = DIRECTION ( 'NONE',  ( 0.000000000000000000, 1.000000000000000000, 0.000000000000000000 ) ) ;
#3988 = SHAPE_DEFINITION_REPRESENTATION ( #20156, #24774 ) ;
#3989 = ORIENTED_EDGE ( 'NONE', *, *, #9879, .F. ) ;
#3990 = ORIENTED_EDGE ( 'NONE', *, *, #7909, .F. ) ;
#3991 = CARTESIAN_POINT ( 'NONE',  ( 170.2234770963711128, -39.20704971665379190, -17.36149277827012938 ) ) ;
#3992 = CARTESIAN_POINT ( 'NONE',  ( 36.88256715603331060, -39.10885149551745599, -16.19941669847073840 ) ) ;
#3993 = ORIENTED_EDGE ( 'NONE', *, *, #4040, .F. ) ;
#3994 = CARTESIAN_POINT ( 'NONE',  ( 200.0000000000000000, -20.00000000000006750, -40.00000000000002132 ) ) ;
#3995 = CARTESIAN_POINT ( 'NONE',  ( -88.37877758188346888, -20.15391234948233290, 8.026456973548603102 ) ) ;
#3996 = ORIENTED_EDGE ( 'NONE', *, *, #20398, .F. ) ;
#3997 = CARTESIAN_POINT ( 'NONE',  ( 199.9999999999998579, 13.86282612285610938, 13.00154682524819805 ) ) ;
#3998 = DIRECTION ( 'NONE',  ( 0.9352143323240051931, 0.3271292299060145070, 0.1355013636716006220 ) ) ;
#3999 = CARTESIAN_POINT ( 'NONE',  ( -135.8532207217289738, 21.81201906317777883, -34.75652343174605363 ) ) ;
#4000 = CARTESIAN_POINT ( 'NONE',  ( -188.3392995398611163, -47.00482667599626296, -13.83024151208815233 ) ) ;
#4001 = CARTESIAN_POINT ( 'NONE',  ( -162.0762913951021176, -40.00000000000019895, 41.69427287672974813 ) ) ;
#4002 = CARTESIAN_POINT ( 'NONE',  ( -198.0356074513804572, 15.37879056873066830, 40.00000000000002132 ) ) ;
#4003 = CARTESIAN_POINT ( 'NONE',  ( -86.96347745069644475, -15.38646221621738164, -41.18208027870615240 ) ) ;
#4004 = CARTESIAN_POINT ( 'NONE',  ( 199.0220573263155188, 3.250837537642027542, 19.73775173755759127 ) ) ;
#4005 = CARTESIAN_POINT ( 'NONE',  ( 136.1360204305621551, -39.99999999999987921, -35.03383547441310242 ) ) ;
#4006 = CARTESIAN_POINT ( 'NONE',  ( -238.4067589809705794, -1.892706720741712928E-13, 40.96449427998260973 ) ) ;
#4007 = CARTESIAN_POINT ( 'NONE',  ( 130.8568914410475088, -40.00000000000036238, 34.05028731879746573 ) ) ;
#4008 = CARTESIAN_POINT ( 'NONE',  ( 130.8568914410475088, 40.00000000000002842, 5.949712681206834830 ) ) ;
#4009 = CARTESIAN_POINT ( 'NONE',  ( -210.0000000000000284, -82.49999999999990052, 52.49999999999977263 ) ) ;
#4010 = CARTESIAN_POINT ( 'NONE',  ( -86.96347745069643054, -41.18208027870589660, -15.38646221621809040 ) ) ;
#4011 = CARTESIAN_POINT ( 'NONE',  ( -280.0000000000000568, 19.99999999999996092, -40.00000000000002132 ) ) ;
#4012 = CARTESIAN_POINT ( 'NONE',  ( -192.9588430854690273, -66.79921049724377724, 10.23066800231950069 ) ) ;
#4013 = CARTESIAN_POINT ( 'NONE',  ( -99.29480781227071873, -8.934325994365618584, 20.48155342677138790 ) ) ;
#4014 = DIRECTION ( 'NONE',  ( 0.000000000000000000, 0.000000000000000000, -1.000000000000000000 ) ) ;
#4015 = CARTESIAN_POINT ( 'NONE',  ( -208.1127848780265026, 1.189126717069624012E-13, -15.00245453012669472 ) ) ;
#4016 = CARTESIAN_POINT ( 'NONE',  ( 4.995406935893305089, -40.00000000000021316, 55.24977328853194791 ) ) ;
#4017 = CARTESIAN_POINT ( 'NONE',  ( -213.1075012329537230, 66.26714140136188291, 9.698598906438215650 ) ) ;
#4018 = CARTESIAN_POINT ( 'NONE',  ( -114.5325442475739663, 19.70118921568331416, 9.696479999167626929 ) ) ;
#4019 = CARTESIAN_POINT ( 'NONE',  ( -192.6563370915134783, -18.27409561805844618, -44.11756948122080502 ) ) ;
#4020 = DIRECTION ( 'NONE',  ( -1.000000000000000000, 1.836970198721030181E-16, 0.000000000000000000 ) ) ;
#4021 = ORIENTED_EDGE ( 'NONE', *, *, #11906, .T. ) ;
#4022 = CARTESIAN_POINT ( 'NONE',  ( -86.96347745069644475, -15.38646221621807442, 15.38646221621768184 ) ) ;
#4023 = DIRECTION ( 'NONE',  ( 0.000000000000000000, 1.000000000000000000, 0.000000000000000000 ) ) ;
#4024 = CARTESIAN_POINT ( 'NONE',  ( 192.4448373802100889, 20.00000000003945644, 0.000000000000000000 ) ) ;
#4025 =( BOUNDED_SURFACE ( )  B_SPLINE_SURFACE ( 3, 2, ( 
 ( #12270, #3762, #22262 ),
 ( #6026, #17980, #24387 ),
 ( #18518, #12138, #20396 ),
 ( #24653, #20523, #3907 ),
 ( #24252, #2170, #18118 ),
 ( #8403, #12005, #4039 ) ),
 .UNSPECIFIED., .F., .F., .F. ) 
 B_SPLINE_SURFACE_WITH_KNOTS ( ( 4, 2, 4 ),
 ( 3, 3 ),
 ( 0.04143191525983294654, 0.04845780415094015636, 0.05548369304204737312 ),
 ( 0.000000000000000000, 1.000000000000000000 ),
 .UNSPECIFIED. ) 
 GEOMETRIC_REPRESENTATION_ITEM ( )  RATIONAL_B_SPLINE_SURFACE ( (
 ( 1.000000000000000000, 0.9541700777564462443, 1.000000000000000000),
 ( 1.000000000000000000, 0.9520117619553596366, 1.000000000000000000),
 ( 1.000000000000000000, 0.9503155880217531992, 1.000000000000000000),
 ( 1.000000000000000000, 0.9480088211921217090, 1.000000000000000000),
 ( 1.000000000000000000, 0.9474362549813150070, 1.000000000000000000),
 ( 1.000000000000000000, 0.9474350312570024579, 1.000000000000000000) ) ) 
 REPRESENTATION_ITEM ( '' )  SURFACE ( )  );
#4026 = DIRECTION ( 'NONE',  ( 1.000000000000000000, 1.836970198721030181E-16, 0.000000000000000000 ) ) ;
#4027 = CARTESIAN_POINT ( 'NONE',  ( 4.995406935893297984, 10.78321810390233892, -67.35176059882522281 ) ) ;
#4028 =( LENGTH_UNIT ( ) NAMED_UNIT ( * ) SI_UNIT ( .MILLI., .METRE. ) );
#4029 = CARTESIAN_POINT ( 'NONE',  ( -86.95450735007487708, 6.704150134086016344, 20.33657406937396672 ) ) ;
#4030 = ORIENTED_EDGE ( 'NONE', *, *, #25360, .F. ) ;
#4031 = CARTESIAN_POINT ( 'NONE',  ( 199.9999999999999147, 15.61914218176268143, 10.83067004454828641 ) ) ;
#4032 = DIRECTION ( 'NONE',  ( 0.000000000000000000, 0.000000000000000000, 1.000000000000000000 ) ) ;
#4033 = CARTESIAN_POINT ( 'NONE',  ( -17.28139728210405579, 12.88180358344996179, 42.38047544431644553 ) ) ;
#4034 = ORIENTED_EDGE ( 'NONE', *, *, #19887, .F. ) ;
#4035 = VERTEX_POINT ( 'NONE', #19900 ) ;
#4036 = PRODUCT_DEFINITION_SHAPE ( 'NONE', 'NONE',  #8176 ) ;
#4037 = CARTESIAN_POINT ( 'NONE',  ( -30.26275506840324070, 1.694272468446254232, 0.000000000000000000 ) ) ;
#4038 = CARTESIAN_POINT ( 'NONE',  ( 199.0065087001378572, 6.107362818253672998, -19.04251412529381327 ) ) ;
#4039 = CARTESIAN_POINT ( 'NONE',  ( -114.7826396787322665, 2.131776515495824860E-13, -22.13135001986800532 ) ) ;
#4040 = EDGE_CURVE ( 'NONE', #1902, #24441, #21639, .T. ) ;
#4041 = CARTESIAN_POINT ( 'NONE',  ( -105.4741150117391157, -7.943527260750152585, -19.77569912955105025 ) ) ;
#4042 = CARTESIAN_POINT ( 'NONE',  ( 170.2234770963711128, -2.259079968736224833E-13, 24.55285855007187124 ) ) ;
#4043 = CARTESIAN_POINT ( 'NONE',  ( -190.0000000000000000, 52.49999999999987210, -82.49999999999998579 ) ) ;
#4044 = CARTESIAN_POINT ( 'NONE',  ( -82.23726319257784212, -20.19517362734544008, -1.261455835848799056 ) ) ;
#4045 = DIRECTION ( 'NONE',  ( 0.2259624731720088209, 0.000000000000000000, -0.9741360072997964359 ) ) ;
#4046 = CARTESIAN_POINT ( 'NONE',  ( 199.0161420530203600, 13.89456085230456850, 14.38651294782529888 ) ) ;
#4047 = DIRECTION ( 'NONE',  ( 0.9698969544100567441, 0.2249791742613287404, 0.09318942523048100168 ) ) ;
#4048 = CARTESIAN_POINT ( 'NONE',  ( 3.468680970036517319, -24.60338114561098166, -44.56630890487775787 ) ) ;
#4049 = CARTESIAN_POINT ( 'NONE',  ( -30.26275506840322649, -29.48230279907769358, -29.48230279907820162 ) ) ;
#4050 = CARTESIAN_POINT ( 'NONE',  ( -114.5516905196692932, 6.814306831805573950, -20.88874846747904357 ) ) ;
#4051 = CARTESIAN_POINT ( 'NONE',  ( -259.2033419157646676, -21.55415060305854524, 21.55415060305827524 ) ) ;
#4052 = CARTESIAN_POINT ( 'NONE',  ( -210.0000000000000284, -1.836970198721030378E-15, 0.000000000000000000 ) ) ;
#4053 = CARTESIAN_POINT ( 'NONE',  ( -30.26275506840324070, -1.198031551616016266, -1.198031551616031587 ) ) ;
#4054 = CARTESIAN_POINT ( 'NONE',  ( -100.7734535825088500, -17.32597176626813251, 40.00000000000002132 ) ) ;
#4055 = PLANE ( 'NONE',  #1964 ) ;
#4056 = CARTESIAN_POINT ( 'NONE',  ( 184.8905102610680444, -19.07866798485555293, -2.449293598294708485E-15 ) ) ;
#4057 = CARTESIAN_POINT ( 'NONE',  ( -105.2926326438279006, 11.51852324731283161, 18.07795834784788624 ) ) ;
#4058 = CARTESIAN_POINT ( 'NONE',  ( 130.8568914410475088, 40.00000000000011369, -5.949712681206269949 ) ) ;
#4059 = CARTESIAN_POINT ( 'NONE',  ( 163.1118516004056573, 9.006482792074356425, -47.56205970284957374 ) ) ;
#4060 = CARTESIAN_POINT ( 'NONE',  ( 130.8568914410475372, -34.05028731879786363, 0.000000000000000000 ) ) ;
#4061 = ORIENTED_EDGE ( 'NONE', *, *, #25592, .T. ) ;
#4062 = ORIENTED_EDGE ( 'NONE', *, *, #16483, .T. ) ;
#4063 = CARTESIAN_POINT ( 'NONE',  ( 151.7948205124836534, -33.23291073765550863, 40.00000000000002132 ) ) ;
#4064 =( GEOMETRIC_REPRESENTATION_CONTEXT ( 3 ) GLOBAL_UNCERTAINTY_ASSIGNED_CONTEXT ( ( #15216 ) ) GLOBAL_UNIT_ASSIGNED_CONTEXT ( ( #10800, #10528, #18506 ) ) REPRESENTATION_CONTEXT ( 'NONE', 'WORKASPACE' ) );
#4065 = SURFACE_STYLE_FILL_AREA ( #4462 ) ;
#4066 = AXIS2_PLACEMENT_3D ( 'NONE', #15847, #12007, #4432 ) ;
#4067 = CARTESIAN_POINT ( 'NONE',  ( -213.1075012329537230, -40.00000000000025580, 53.71589010953650956 ) ) ;
#4068 = CIRCLE ( 'NONE', #2799, 6.000000000000005329 ) ;
#4069 = CARTESIAN_POINT ( 'NONE',  ( -135.8532207217289738, 50.09629031063956006, 6.472252184284782217 ) ) ;
#4070 = DIRECTION ( 'NONE',  ( -0.01051738777841060291, -0.9307051272558614086, -0.3656191333258823617 ) ) ;
#4071 = CARTESIAN_POINT ( 'NONE',  ( 200.0000000000000000, 52.50000000000007816, 52.49999999999999289 ) ) ;
#4072 = DIRECTION ( 'NONE',  ( -1.000000000000000000, -0.000000000000000000, -0.000000000000000000 ) ) ;
#4073 = CARTESIAN_POINT ( 'NONE',  ( 200.0000000000000853, 16.14603016630555743, -10.01676266068942667 ) ) ;
#4074 = CARTESIAN_POINT ( 'NONE',  ( 199.9999999999998863, -17.79060443684709369, -6.693342262146931176 ) ) ;
#4076 = AXIS2_PLACEMENT_3D ( 'NONE', #23567, #13452, #5342 ) ;
#4075 = CARTESIAN_POINT ( 'NONE',  ( 184.8905102610680444, 13.49065550809826952, -13.49065550809790359 ) ) ;
#4077 = CARTESIAN_POINT ( 'NONE',  ( -280.0000000000000568, -14.14213562373137556, 42.42640687119276066 ) ) ;
#4078 = DIRECTION ( 'NONE',  ( 0.000000000000000000, -0.7071067811865561215, 0.7071067811865389130 ) ) ;
#4079 = CARTESIAN_POINT ( 'NONE',  ( -56.48582580120559271, -1.062504017861011783E-13, 9.153146818113587102 ) ) ;
#4080 = CARTESIAN_POINT ( 'NONE',  ( 130.8568914410475372, -4.207082182992785135, -4.207082182992884611 ) ) ;
#4081 = CARTESIAN_POINT ( 'NONE',  ( 91.82158438592158234, -12.16597498397778843, 12.16597498397750954 ) ) ;
#4082 = CARTESIAN_POINT ( 'NONE',  ( -91.56559293963834989, -16.03295912088706388, -16.03295912088710651 ) ) ;
#4083 = CARTESIAN_POINT ( 'NONE',  ( 136.1360204305621266, 24.77266263493138965, -24.77266263493110188 ) ) ;
#4084 = CARTESIAN_POINT ( 'NONE',  ( 199.0206793870229376, 6.297627498482031072, 19.03991857512456320 ) ) ;
#4086 = CARTESIAN_POINT ( 'NONE',  ( 130.8568914410475088, 40.00000000000002842, 5.949712681206834830 ) ) ;
#4085 = CARTESIAN_POINT ( 'NONE',  ( 14.38125909742181108, 39.01709431150961649, -39.01709431150867147 ) ) ;
#4087 = VECTOR ( 'NONE', #5755, 1000.000000000000114 ) ;
#4088 = CARTESIAN_POINT ( 'NONE',  ( 19.06497207195979726, 38.31983398719604139, 18.24870850772803976 ) ) ;
#4089 = VECTOR ( 'NONE', #2213, 1000.000000000000000 ) ;
#4090 = CARTESIAN_POINT ( 'NONE',  ( 23.37583784646129104, 46.80752016581939046, -13.80085822091003500 ) ) ;
#4091 = CARTESIAN_POINT ( 'NONE',  ( 19.06497207195980792, 54.19242893257843718, 2.449293598294708485E-15 ) ) ;
#4092 = ORIENTED_EDGE ( 'NONE', *, *, #18990, .F. ) ;
#4093 = DIRECTION ( 'NONE',  ( 0.000000000000000000, 0.000000000000000000, 1.000000000000000000 ) ) ;
#4094 = CARTESIAN_POINT ( 'NONE',  ( -16.78454218905211093, -39.63790004368954811, 16.41855578202928356 ) ) ;
#4095 = CARTESIAN_POINT ( 'NONE',  ( -86.96347745069644475, -21.75974354311651737, 0.000000000000000000 ) ) ;
#4096 = EDGE_LOOP ( 'NONE', ( #20816, #186 ) ) ;
#4097 = CARTESIAN_POINT ( 'NONE',  ( -3.069599232962576085, 23.65302469262847751, -43.28003856805327842 ) ) ;
#4098 = CARTESIAN_POINT ( 'NONE',  ( 200.0000000000000853, -13.44239485489230290, 13.44239485489200803 ) ) ;
#4099 = CARTESIAN_POINT ( 'NONE',  ( -2.164901439689549179, -13.92557459411189313, 47.64638340556978591 ) ) ;
#4100 = CARTESIAN_POINT ( 'NONE',  ( 22.70429368897870859, 17.89136451867761579, -43.19357487035025400 ) ) ;
#4101 = CARTESIAN_POINT ( 'NONE',  ( 199.0111317961331281, -6.131174403448985011, -19.03732645848564431 ) ) ;
#4102 = VECTOR ( 'NONE', #24243, 1000.000000000000000 ) ;
#4103 = CARTESIAN_POINT ( 'NONE',  ( 23.37394308801977871, -46.80823611210205115, 13.80096434448272724 ) ) ;
#4104 = CARTESIAN_POINT ( 'NONE',  ( 151.0853911467767432, -29.06993079631231325, 12.04115959307964090 ) ) ;
#4105 = CARTESIAN_POINT ( 'NONE',  ( 163.1118516004056573, 1.251511021549353291E-13, -27.26290988616872824 ) ) ;
#4106 = EDGE_CURVE ( 'NONE', #9701, #3571, #21500, .T. ) ;
#4107 = CARTESIAN_POINT ( 'NONE',  ( -192.9588430854689989, 38.51493924976983152, -38.51493924976893624 ) ) ;
#4108 = CARTESIAN_POINT ( 'NONE',  ( -99.21568817060988010, -22.67402823373193499, 0.000000000000000000 ) ) ;
#4110 = CARTESIAN_POINT ( 'NONE',  ( -105.3755690713226585, 12.89780903124349720, 43.67073346367994446 ) ) ;
#4109 = CARTESIAN_POINT ( 'NONE',  ( -188.8532066752251808, 17.93248812771325262, -43.29285604501834683 ) ) ;
#4111 = CARTESIAN_POINT ( 'NONE',  ( 199.9999999999999432, 20.00000000000013856, 0.000000000000000000 ) ) ;
#4112 = CARTESIAN_POINT ( 'NONE',  ( 170.2234770963711128, -15.44714144992812699, -40.00000000000002132 ) ) ;
#4113 = CARTESIAN_POINT ( 'NONE',  ( -213.1075012329537230, 53.71589010951910836, 2.449293598294708485E-15 ) ) ;
#4114 = EDGE_CURVE ( 'NONE', #5117, #21778, #22040, .T. ) ;
#4115 = CARTESIAN_POINT ( 'NONE',  ( 151.7948205124836250, 1.012150473917908975E-13, -6.767089262349031742 ) ) ;
#4116 = CARTESIAN_POINT ( 'NONE',  ( -56.48582580120559982, 50.09629031063966664, -6.472252184284094767 ) ) ;
#4117 = AXIS2_PLACEMENT_3D ( 'NONE', #15963, #12247, #18363 ) ;
#4118 = CARTESIAN_POINT ( 'NONE',  ( -105.4732637872223080, 19.68494377761377123, -8.153770687239582315 ) ) ;
#4119 = CARTESIAN_POINT ( 'NONE',  ( -86.96347745069645896, 43.67073346367988762, -12.89780903124366418 ) ) ;
#4120 = EDGE_CURVE ( 'NONE', #15268, #9701, #13640, .T. ) ;
#4121 = ADVANCED_FACE ( 'NONE', ( #3539 ), #10569, .T. ) ;
#4122 = ORIENTED_EDGE ( 'NONE', *, *, #21755, .T. ) ;
#4123 = CARTESIAN_POINT ( 'NONE',  ( -91.56559293963834989, -44.31723036834903695, 12.25131212657476709 ) ) ;
#4124 = CARTESIAN_POINT ( 'NONE',  ( -77.55640685876518603, 15.64922766773203122, 15.64922766773211471 ) ) ;
#4125 = APPLICATION_PROTOCOL_DEFINITION ( 'draft international standard', 'automotive_design', 1998, #19110 ) ;
#4126 = ORIENTED_EDGE ( 'NONE', *, *, #14927, .T. ) ;
#4127 = ORIENTED_EDGE ( 'NONE', *, *, #7691, .T. ) ;
#4128 = CARTESIAN_POINT ( 'NONE',  ( -198.0356074513804572, -39.15871834505905724, -17.40982414986491733 ) ) ;
#4129 = CARTESIAN_POINT ( 'NONE',  ( 45.01779936579357866, -38.89115870262487107, -12.15764947739186930 ) ) ;
#4130 = VERTEX_POINT ( 'NONE', #26285 ) ;
#4131 = CARTESIAN_POINT ( 'NONE',  ( -135.8532207217289738, -9.153146818113595984, 0.000000000000000000 ) ) ;
#4132 = B_SPLINE_CURVE_WITH_KNOTS ( 'NONE', 3,
 ( #4408, #25162, #8917, #18629, #2811, #412 ),
 .UNSPECIFIED., .F., .F.,
 ( 4, 2, 4 ),
 ( -5.999999999678665604E-08, 0.03937727993095216372, 0.07875461986190432362 ),
 .UNSPECIFIED. ) ;
#4133 = CARTESIAN_POINT ( 'NONE',  ( -93.01741312767373415, -20.82169463879412419, 8.169811846252175158 ) ) ;
#4134 = ORIENTED_EDGE ( 'NONE', *, *, #15447, .T. ) ;
#4135 = CARTESIAN_POINT ( 'NONE',  ( 199.9999999999998863, 12.28125103214278901, 14.50804496155330447 ) ) ;
#4136 =( BOUNDED_SURFACE ( )  B_SPLINE_SURFACE ( 3, 2, ( 
 ( #23644, #3046, #21272 ),
 ( #11153, #25402, #5422 ),
 ( #21524, #19268, #21400 ),
 ( #17267, #7401, #21147 ),
 ( #19398, #9283, #6896 ),
 ( #13525, #3173, #23272 ),
 ( #2790, #15395, #1050 ),
 ( #5292, #4915, #23520 ),
 ( #19015, #10903, #23398 ),
 ( #13027, #1302, #5174 ),
 ( #7279, #7021, #25273 ),
 ( #13278, #17391, #17138 ),
 ( #9034, #25530, #2921 ),
 ( #11029, #13399, #19139 ),
 ( #3300, #923, #11394 ),
 ( #9411, #17517, #19777 ),
 ( #25917, #7533, #17910 ),
 ( #13655, #16182, #19648 ),
 ( #21649, #5814, #21779 ),
 ( #11795, #7660, #19914 ),
 ( #17640, #9934, #18040 ),
 ( #26194, #6083, #10070 ),
 ( #12064, #3552, #3965 ),
 ( #25783, #7790, #16048 ),
 ( #20181, #15641, #22190 ),
 ( #5948, #24318, #3687 ),
 ( #22054, #13919, #1965 ),
 ( #18175, #8065, #1698 ),
 ( #23769, #24173, #15772 ),
 ( #5547, #14056, #26323 ),
 ( #11653, #3421, #9803 ),
 ( #26053, #3827, #11523 ),
 ( #11929, #20054, #15906 ),
 ( #1565, #1433, #1833 ) ),
 .UNSPECIFIED., .F., .F., .F. ) 
 B_SPLINE_SURFACE_WITH_KNOTS ( ( 4, 2, 2, 2, 2, 2, 2, 2, 2, 2, 2, 2, 2, 2, 2, 2, 4 ),
 ( 3, 3 ),
 ( 0.005135432767689945138, 0.02907015807668583696, 0.05300488338568172531, 0.07693960869467761365, 0.08292329002192658227, 0.08441921035373882443, 0.08446595786410796003, 0.08448933161929252089, 0.08451270537447708175, 0.08460620039521535296, 0.08479319043669189537, 0.08516717051964495244, 0.08591513068555106658, 0.08890697134917555089, 0.09189881201280003520, 0.09489065267642451951, 0.1008743340036735020 ),
 ( 0.000000000000000000, 1.000000000000000000 ),
 .UNSPECIFIED. ) 
 GEOMETRIC_REPRESENTATION_ITEM ( )  RATIONAL_B_SPLINE_SURFACE ( (
 ( 1.000000000000000000, 0.9997813423552077694, 1.000000000000000000),
 ( 1.000000000000000000, 0.9991063898506412633, 1.000000000000000000),
 ( 1.000000000000000000, 0.9968824705949630438, 1.000000000000000000),
 ( 1.000000000000000000, 0.9891556793369802314, 1.000000000000000000),
 ( 1.000000000000000000, 0.9836552277517739418, 1.000000000000000000),
 ( 1.000000000000000000, 0.9690805015308342485, 1.000000000000000000),
 ( 1.000000000000000000, 0.9600094330338765358, 1.000000000000000000),
 ( 1.000000000000000000, 0.9461485276688212931, 1.000000000000000000),
 ( 1.000000000000000000, 0.9432497373317600964, 1.000000000000000000),
 ( 1.000000000000000000, 0.9394620364518223576, 1.000000000000000000),
 ( 1.000000000000000000, 0.9386962831138082608, 1.000000000000000000),
 ( 1.000000000000000000, 0.9378980481303071937, 1.000000000000000000),
 ( 1.000000000000000000, 0.9378738510928912309, 1.000000000000000000),
 ( 1.000000000000000000, 0.9378375433852945697, 1.000000000000000000),
 ( 1.000000000000000000, 0.9378253334781214701, 1.000000000000000000),
 ( 1.000000000000000000, 0.9378014123365954191, 1.000000000000000000),
 ( 1.000000000000000000, 0.9377894572438932874, 1.000000000000000000),
 ( 1.000000000000000000, 0.9377297092068097584, 1.000000000000000000),
 ( 1.000000000000000000, 0.9376819985415333347, 1.000000000000000000),
 ( 1.000000000000000000, 0.9375391312191839743, 1.000000000000000000),
 ( 1.000000000000000000, 0.9374442392362084542, 1.000000000000000000),
 ( 1.000000000000000000, 0.9371606329891914999, 1.000000000000000000),
 ( 1.000000000000000000, 0.9369729884417196120, 1.000000000000000000),
 ( 1.000000000000000000, 0.9364144211479191737, 1.000000000000000000),
 ( 1.000000000000000000, 0.9360478649890143776, 1.000000000000000000),
 ( 1.000000000000000000, 0.9342453465010664981, 1.000000000000000000),
 ( 1.000000000000000000, 0.9329002455189063792, 1.000000000000000000),
 ( 1.000000000000000000, 0.9304321598240474778, 1.000000000000000000),
 ( 1.000000000000000000, 0.9293115443288696431, 1.000000000000000000),
 ( 1.000000000000000000, 0.9273348408774876317, 1.000000000000000000),
 ( 1.000000000000000000, 0.9264755133097204443, 1.000000000000000000),
 ( 1.000000000000000000, 0.9243017816400511677, 1.000000000000000000),
 ( 1.000000000000000000, 0.9233922826849433330, 1.000000000000000000),
 ( 1.000000000000000000, 0.9230541040371987860, 1.000000000000000000) ) ) 
 REPRESENTATION_ITEM ( '' )  SURFACE ( )  );
#4137 = DIRECTION ( 'NONE',  ( 0.000000000000000000, -1.682156097916903834E-16, -1.000000000000000000 ) ) ;
#4138 = CARTESIAN_POINT ( 'NONE',  ( -259.2033419157646676, -6.730120644403570829, -6.730120644403545960 ) ) ;
#4139 = CARTESIAN_POINT ( 'NONE',  ( -188.9266751785330314, -43.31221945728822220, -17.94050871568865091 ) ) ;
#4140 = VECTOR ( 'NONE', #16370, 1000.000000000000000 ) ;
#4141 = CARTESIAN_POINT ( 'NONE',  ( 151.7948205124836534, -39.99999999999987921, -33.23291073765567916 ) ) ;
#4142 = CARTESIAN_POINT ( 'NONE',  ( 136.1360204305621266, -35.03383547441293899, 0.000000000000000000 ) ) ;
#4143 = CARTESIAN_POINT ( 'NONE',  ( -280.0000000000000000, 14.14213562373108246, -14.14213562373078581 ) ) ;
#4144 = CARTESIAN_POINT ( 'NONE',  ( 199.0262541782678340, -11.79586192385960430, 16.15815307234555576 ) ) ;
#4145 = CARTESIAN_POINT ( 'NONE',  ( -56.48582580120558561, -40.00000000000000000, -9.153146818113723882 ) ) ;
#4146 = CARTESIAN_POINT ( 'NONE',  ( 19.06497207195981858, -1.881589693694111225E-13, 54.19242893257843008 ) ) ;
#4147 = CARTESIAN_POINT ( 'NONE',  ( -135.8532207217289738, 7.002209520526292428E-15, -9.153146818113572891 ) ) ;
#4148 = CARTESIAN_POINT ( 'NONE',  ( -192.9588430854689989, -14.46834944099973086, 0.000000000000000000 ) ) ;
#4149 = CARTESIAN_POINT ( 'NONE',  ( -86.96347745069644475, -12.89780903124413491, 12.89780903124398037 ) ) ;
#4150 = CARTESIAN_POINT ( 'NONE',  ( -100.7734535825088500, 22.67402823373189946, -40.00000000000002132 ) ) ;
#4151 = CARTESIAN_POINT ( 'NONE',  ( 151.7948205124836534, 23.49921654116009506, 33.06932595376371609 ) ) ;
#4152 = PLANE ( 'NONE',  #4117 ) ;
#4153 = CARTESIAN_POINT ( 'NONE',  ( -716.9846540392142060, 66.50000000000009948, -71.50000000000005684 ) ) ;
#4154 = CARTESIAN_POINT ( 'NONE',  ( -100.7734535825088500, 39.99999999999976552, 22.67402823373233645 ) ) ;
#4155 = CARTESIAN_POINT ( 'NONE',  ( -198.0356074513804572, 39.99999999999979394, 55.37879056874835726 ) ) ;
#4156 = CARTESIAN_POINT ( 'NONE',  ( 136.1360204305621551, 31.79587985999267374, -24.77266263493117293 ) ) ;
#4157 = CARTESIAN_POINT ( 'NONE',  ( 14.38125909742181285, -10.73282306404712472, -10.73282306404731301 ) ) ;
#4158 = CARTESIAN_POINT ( 'NONE',  ( -188.4265466358326080, -23.47687925214715321, -43.04237830660283493 ) ) ;
#4159 = CARTESIAN_POINT ( 'NONE',  ( -726.9846540392142060, 0.000000000000000000, 0.000000000000000000 ) ) ;
#4160 = ORIENTED_EDGE ( 'NONE', *, *, #8905, .F. ) ;
#4161 = CARTESIAN_POINT ( 'NONE',  ( 151.7948205124836250, -23.49921654116371883, 23.49921654116317526 ) ) ;
#4162 = B_SPLINE_CURVE_WITH_KNOTS ( 'NONE', 3,
 ( #19957, #13569, #15688, #16093, #21695, #15959, #3471, #1477, #9715, #5595, #21826, #1877, #3595, #11975 ),
 .UNSPECIFIED., .F., .F.,
 ( 4, 2, 2, 2, 2, 2, 4 ),
 ( 2.647940464546886252E-17, 0.002941681445497028834, 0.004412522168245528939, 0.005883362890994029044, 0.008825044336491017979, 0.01029588505923952069, 0.01176672578198802166 ),
 .UNSPECIFIED. ) ;
#4163 = DIRECTION ( 'NONE',  ( -0.3301743741188450376, 0.000000000000000000, -0.9439199556504932476 ) ) ;
#4164 = CARTESIAN_POINT ( 'NONE',  ( -198.0356074513804572, -15.37879056873074290, -40.00000000000002132 ) ) ;
#4165 = CARTESIAN_POINT ( 'NONE',  ( -87.11017345524855671, 17.07168028895587852, 13.10675206033511131 ) ) ;
#4166 = CARTESIAN_POINT ( 'NONE',  ( 0.2972598230769990524, -18.14793986248671231, -38.42060263243687501 ) ) ;
#4167 = EDGE_LOOP ( 'NONE', ( #4648, #20084, #12084, #10262, #3453 ) ) ;
#4168 = VERTEX_POINT ( 'NONE', #3925 ) ;
#4169 = CARTESIAN_POINT ( 'NONE',  ( 199.9999999999999716, 16.82248425547956217, 8.841323171526189739 ) ) ;
#4170 = CARTESIAN_POINT ( 'NONE',  ( 1.564570055219380196, -24.39611894128483627, 44.28524390194910865 ) ) ;
#4171 = CARTESIAN_POINT ( 'NONE',  ( -2.004660104981413227, 18.09067139728989559, 43.67474423981169451 ) ) ;
#4172 = EDGE_LOOP ( 'NONE', ( #8266, #6834, #3852, #6664 ) ) ;
#4173 = EDGE_LOOP ( 'NONE', ( #25851, #18747, #17266, #5978 ) ) ;
#4174 = CARTESIAN_POINT ( 'NONE',  ( -100.7734535825088358, -22.67402823373193499, 0.000000000000000000 ) ) ;
#4175 = CARTESIAN_POINT ( 'NONE',  ( 199.0087111817176435, -0.6649071253763039202, -19.99597453042600392 ) ) ;
#4176 = CARTESIAN_POINT ( 'NONE',  ( -77.78698626355769363, -9.956330463956303944, -19.58753875850657167 ) ) ;
#4177 = DIRECTION ( 'NONE',  ( 0.000000000000000000, -0.9166903767142837722, -0.3995982397851930989 ) ) ;
#4178 = CARTESIAN_POINT ( 'NONE',  ( 3.854700064722245578, 44.60002223906914054, -24.62824689551992563 ) ) ;
#4179 = CARTESIAN_POINT ( 'NONE',  ( -91.56559293963836410, 40.00000000000019185, -17.32597176626768487 ) ) ;
#4180 = CARTESIAN_POINT ( 'NONE',  ( 200.0000000000000284, -14.89458464808834748, 11.81399803044240038 ) ) ;
#4181 = CARTESIAN_POINT ( 'NONE',  ( -642.1644459338755269, 30.49398659613246920, 25.89371287723436055 ) ) ;
#4182 = CARTESIAN_POINT ( 'NONE',  ( -210.0000000000000284, 66.50000000000001421, -66.50000000000005684 ) ) ;
#4183 = CARTESIAN_POINT ( 'NONE',  ( 199.0152755141893692, 15.03153897770602221, 13.19647528785794677 ) ) ;
#4184 = CARTESIAN_POINT ( 'NONE',  ( -121.8281105898911818, 8.694016233166976804, 23.07023229731760239 ) ) ;
#4185 = CARTESIAN_POINT ( 'NONE',  ( -3.406542234095930155, -17.94112998239644341, -43.31371932780105283 ) ) ;
#4186 = CARTESIAN_POINT ( 'NONE',  ( -100.7734535825088500, -40.53558337403692491, 16.03295912088671571 ) ) ;
#4187 =( BOUNDED_SURFACE ( )  B_SPLINE_SURFACE ( 3, 3, ( 
 ( #11115, #20970, #19100, #22839, #12710, #347, #8451, #18972, #6982, #12578, #10584, #8590, #25874, #23728, #1395, #1009, #5509, #25743, #3515, #5383, #1525, #13611, #7618, #13359, #5636, #19229, #7492, #23604, #9112, #13488 ),
 ( #21609, #5257, #9247, #9496, #11360, #9632, #17223, #15477, #7365, #19477, #25619, #3256, #1263, #11235, #19353, #3383, #17601, #11481, #7116, #19609, #7238, #25362, #15733, #23859, #1142, #15227, #17353, #25489, #23358, #15603 ),
 ( #21869, #21739, #11615, #5135, #19737, #17477, #17733, #13743, #3647, #13240, #21365, #3133, #15359, #23483, #21481, #9367, #20280, #7752, #24135, #14016, #24275, #7889, #13880, #1922, #16142, #22013, #3784, #6171, #2059, #10165 ),
 ( #23992, #14150, #18268, #2191, #181, #20415, #52, #22546, #6045, #11752, #10028, #19873, #18138, #5772, #8164, #10299, #26145, #9764, #26286, #11886, #15863, #20007, #16009, #22282, #8025, #12158, #3926, #4056, #16276, #18000 ),
 ( #8288, #20144, #24405, #9896, #6298, #18406, #1792, #16415, #5907, #14281, #22145, #12024, #24543, #14416, #22418, #4194, #12287, #1655, #17865, #26015, #8831, #12827, #12417, #16940, #10830, #14945, #16809, #12956, #25075, #10967 ),
 ( #4327, #18945, #8698, #20545, #24947, #10423, #22940, #20814, #18811, #2586, #23079, #21075, #4452, #6695, #14548, #4851, #12547, #20679, #18541, #726, #6826, #19075, #24808, #2860, #856, #323, #8424, #2315, #14808, #6430 ),
 ( #4720, #591, #4587, #8563, #8965, #16544, #10559, #24674, #10701, #22678, #458, #2448, #17074, #25208, #6956, #15073, #18672, #16677, #6560, #14675, #22811, #12684, #20947, #2725, #11088, #17452, #7591, #11584, #5230, #5355 ) ),
 .UNSPECIFIED., .T., .F., .F. ) 
 B_SPLINE_SURFACE_WITH_KNOTS ( ( 4, 3, 4 ),
 ( 4, 2, 2, 2, 2, 2, 2, 2, 2, 2, 2, 2, 2, 2, 4 ),
 ( 0.000000000000000000, 0.5000000000000000000, 1.000000000000000000 ),
 ( 0.000000000000000000, 0.1357259735107005372, 0.1651108541090157700, 0.1944957347073310028, 0.3598804999793158710, 0.3867117631979620773, 0.4135430264166082281, 0.5789277916885930964, 0.6062785021374117456, 0.6336292125862302838, 0.8508620842112317728, 0.8814014469398914198, 0.9119408096685510667, 0.9559704048342755334, 1.000000000000000000 ),
 .UNSPECIFIED. ) 
 GEOMETRIC_REPRESENTATION_ITEM ( )  RATIONAL_B_SPLINE_SURFACE ( (
 ( 1.000000000000000000, 1.000000000000000000, 1.000000000000000000, 1.000000000000000000, 1.000000000000000000, 1.000000000000000000, 1.000000000000000000, 1.000000000000000000, 1.000000000000000000, 1.000000000000000000, 1.000000000000000000, 1.000000000000000000, 1.000000000000000000, 1.000000000000000000, 1.000000000000000000, 1.000000000000000000, 1.000000000000000000, 1.000000000000000000, 1.000000000000000000, 1.000000000000000000, 1.000000000000000000, 1.000000000000000000, 1.000000000000000000, 1.000000000000000000, 1.000000000000000000, 1.000000000000000000, 1.000000000000000000, 1.000000000000000000, 1.000000000000000000, 1.000000000000000000),
 ( 0.3333333333333333703, 0.3333333333333333703, 0.3333333333333333703, 0.3333333333333333703, 0.3333333333333333703, 0.3333333333333333703, 0.3333333333333333703, 0.3333333333333333703, 0.3333333333333333703, 0.3333333333333333703, 0.3333333333333333703, 0.3333333333333333703, 0.3333333333333333703, 0.3333333333333333703, 0.3333333333333333703, 0.3333333333333333703, 0.3333333333333333703, 0.3333333333333333703, 0.3333333333333333703, 0.3333333333333333703, 0.3333333333333333703, 0.3333333333333333703, 0.3333333333333333703, 0.3333333333333333703, 0.3333333333333333703, 0.3333333333333333703, 0.3333333333333333703, 0.3333333333333333703, 0.3333333333333333703, 0.3333333333333333703),
 ( 0.3333333333333333703, 0.3333333333333333703, 0.3333333333333333703, 0.3333333333333333703, 0.3333333333333333703, 0.3333333333333333703, 0.3333333333333333703, 0.3333333333333333703, 0.3333333333333333703, 0.3333333333333333703, 0.3333333333333333703, 0.3333333333333333703, 0.3333333333333333703, 0.3333333333333333703, 0.3333333333333333703, 0.3333333333333333703, 0.3333333333333333703, 0.3333333333333333703, 0.3333333333333333703, 0.3333333333333333703, 0.3333333333333333703, 0.3333333333333333703, 0.3333333333333333703, 0.3333333333333333703, 0.3333333333333333703, 0.3333333333333333703, 0.3333333333333333703, 0.3333333333333333703, 0.3333333333333333703, 0.3333333333333333703),
 ( 1.000000000000000000, 1.000000000000000000, 1.000000000000000000, 1.000000000000000000, 1.000000000000000000, 1.000000000000000000, 1.000000000000000000, 1.000000000000000000, 1.000000000000000000, 1.000000000000000000, 1.000000000000000000, 1.000000000000000000, 1.000000000000000000, 1.000000000000000000, 1.000000000000000000, 1.000000000000000000, 1.000000000000000000, 1.000000000000000000, 1.000000000000000000, 1.000000000000000000, 1.000000000000000000, 1.000000000000000000, 1.000000000000000000, 1.000000000000000000, 1.000000000000000000, 1.000000000000000000, 1.000000000000000000, 1.000000000000000000, 1.000000000000000000, 1.000000000000000000),
 ( 0.3333333333333333703, 0.3333333333333333703, 0.3333333333333333703, 0.3333333333333333703, 0.3333333333333333703, 0.3333333333333333703, 0.3333333333333333703, 0.3333333333333333703, 0.3333333333333333703, 0.3333333333333333703, 0.3333333333333333703, 0.3333333333333333703, 0.3333333333333333703, 0.3333333333333333703, 0.3333333333333333703, 0.3333333333333333703, 0.3333333333333333703, 0.3333333333333333703, 0.3333333333333333703, 0.3333333333333333703, 0.3333333333333333703, 0.3333333333333333703, 0.3333333333333333703, 0.3333333333333333703, 0.3333333333333333703, 0.3333333333333333703, 0.3333333333333333703, 0.3333333333333333703, 0.3333333333333333703, 0.3333333333333333703),
 ( 0.3333333333333333703, 0.3333333333333333703, 0.3333333333333333703, 0.3333333333333333703, 0.3333333333333333703, 0.3333333333333333703, 0.3333333333333333703, 0.3333333333333333703, 0.3333333333333333703, 0.3333333333333333703, 0.3333333333333333703, 0.3333333333333333703, 0.3333333333333333703, 0.3333333333333333703, 0.3333333333333333703, 0.3333333333333333703, 0.3333333333333333703, 0.3333333333333333703, 0.3333333333333333703, 0.3333333333333333703, 0.3333333333333333703, 0.3333333333333333703, 0.3333333333333333703, 0.3333333333333333703, 0.3333333333333333703, 0.3333333333333333703, 0.3333333333333333703, 0.3333333333333333703, 0.3333333333333333703, 0.3333333333333333703),
 ( 1.000000000000000000, 1.000000000000000000, 1.000000000000000000, 1.000000000000000000, 1.000000000000000000, 1.000000000000000000, 1.000000000000000000, 1.000000000000000000, 1.000000000000000000, 1.000000000000000000, 1.000000000000000000, 1.000000000000000000, 1.000000000000000000, 1.000000000000000000, 1.000000000000000000, 1.000000000000000000, 1.000000000000000000, 1.000000000000000000, 1.000000000000000000, 1.000000000000000000, 1.000000000000000000, 1.000000000000000000, 1.000000000000000000, 1.000000000000000000, 1.000000000000000000, 1.000000000000000000, 1.000000000000000000, 1.000000000000000000, 1.000000000000000000, 1.000000000000000000) ) ) 
 REPRESENTATION_ITEM ( '' )  SURFACE ( )  );
#4188 = CARTESIAN_POINT ( 'NONE',  ( -200.0000000000000000, 22.85346793133691889, 44.96258949770047764 ) ) ;
#4189 = CARTESIAN_POINT ( 'NONE',  ( 57.59792236341148453, -54.84617931850877426, -1.722363176415331099 ) ) ;
#4190 = CARTESIAN_POINT ( 'NONE',  ( -77.80650228860213247, 20.78729124363272973, 7.074397727529034618 ) ) ;
#4191 = CARTESIAN_POINT ( 'NONE',  ( 151.7948205124836250, 23.49921654116328540, 23.49921654116366554 ) ) ;
#4192 = CARTESIAN_POINT ( 'NONE',  ( 146.6084372240433709, -5.374981219216948602, 40.00000000000002132 ) ) ;
#4193 = CARTESIAN_POINT ( 'NONE',  ( 163.1118516004056573, 19.27778845538780317, -19.27778845538757224 ) ) ;
#4194 = CARTESIAN_POINT ( 'NONE',  ( 0.2972598230770129857, -54.33493731733938148, 40.00000000000002132 ) ) ;
#4195 = CARTESIAN_POINT ( 'NONE',  ( -105.4741150117367283, 19.77569912955882359, -7.943527260733686646 ) ) ;
#4196 = CARTESIAN_POINT ( 'NONE',  ( -162.0762913951021176, 40.00000000000001421, -1.694272876827905394 ) ) ;
#4197 = CARTESIAN_POINT ( 'NONE',  ( 192.4448373802101173, 42.42640687116508502, -14.14213562375874567 ) ) ;
#4198 = CARTESIAN_POINT ( 'NONE',  ( -100.7734535825088500, -22.67402823373193499, -40.00000000000002132 ) ) ;
#4199 = VERTEX_POINT ( 'NONE', #16543 ) ;
#4200 = ORIENTED_EDGE ( 'NONE', *, *, #9474, .F. ) ;
#4201 = CARTESIAN_POINT ( 'NONE',  ( 130.8568914410475372, -34.05028731879786363, 0.000000000000000000 ) ) ;
#4202 = CARTESIAN_POINT ( 'NONE',  ( -99.29480781227057662, -8.165122821357709171, -20.80016781325170783 ) ) ;
#4203 = CARTESIAN_POINT ( 'NONE',  ( 0.2972598230769883387, 39.99999999999997158, 14.33493731733947563 ) ) ;
#4204 = CARTESIAN_POINT ( 'NONE',  ( -91.56559293963834989, 40.53558337403654832, 16.03295912088756481 ) ) ;
#4205 = CARTESIAN_POINT ( 'NONE',  ( 151.7948205124836250, -33.23291073765550863, 0.000000000000000000 ) ) ;
#4206 = EDGE_CURVE ( 'NONE', #1180, #25953, #22281, .T. ) ;
#4207 = CARTESIAN_POINT ( 'NONE',  ( -126.6834156231674342, 9.107266674873963908, -24.89646324320098714 ) ) ;
#4208 = CARTESIAN_POINT ( 'NONE',  ( -200.0000000000000000, 66.50000000000009948, -66.50000000000005684 ) ) ;
#4209 = CARTESIAN_POINT ( 'NONE',  ( 200.0000000000001421, 16.60215271479902910, 9.252637072649047667 ) ) ;
#4210 = ADVANCED_FACE ( 'NONE', ( #9895, #16414 ), #22677, .F. ) ;
#4211 = CARTESIAN_POINT ( 'NONE',  ( 199.9999999999999147, -17.31672820518381783, 7.849270303112303004 ) ) ;
#4212 = CARTESIAN_POINT ( 'NONE',  ( 19.06497207195981147, 38.31983398719673772, -38.31983398719579981 ) ) ;
#4213 = CARTESIAN_POINT ( 'NONE',  ( -238.4067589809705794, -57.25054294077233408, -0.6820004458489551391 ) ) ;
#4214 = CARTESIAN_POINT ( 'NONE',  ( -210.0000000000000284, 71.50000000000009948, 66.50000000000005684 ) ) ;
#4215 = CARTESIAN_POINT ( 'NONE',  ( -259.2033419157646676, 40.00000000000029843, -30.48217210827696988 ) ) ;
#4216 = CARTESIAN_POINT ( 'NONE',  ( -135.8532207217289738, -50.09629031063973770, 6.472252184283735943 ) ) ;
#4217 = CARTESIAN_POINT ( 'NONE',  ( 199.9999999999999432, -14.14213562373115884, 14.14213562373085153 ) ) ;
#4218 = CARTESIAN_POINT ( 'NONE',  ( -105.3755690713226585, -43.67073346367983788, 12.89780903124397149 ) ) ;
#4219 = ADVANCED_FACE ( 'NONE', ( #20279 ), #24134, .T. ) ;
#4220 = CARTESIAN_POINT ( 'NONE',  ( -192.9588430854690273, -38.51493924976932703, -18.05360324515463688 ) ) ;
#4221 = CARTESIAN_POINT ( 'NONE',  ( 199.0168430542531155, 12.91005451537445126, 15.29445721284177573 ) ) ;
#4222 = AXIS2_PLACEMENT_3D ( 'NONE', #23852, #25868, #5503 ) ;
#4223 = ADVANCED_FACE ( 'NONE', ( #50 ), #4055, .T. ) ;
#4225 = CARTESIAN_POINT ( 'NONE',  ( -280.0000000000000568, 39.99999999999990763, 20.00000000000015987 ) ) ;
#4224 = CARTESIAN_POINT ( 'NONE',  ( -192.9588430854690273, 10.23066800229588758, -66.79921049721882298 ) ) ;
#4226 = CARTESIAN_POINT ( 'NONE',  ( 136.1360204305621551, 31.79587985999232558, 24.77266263493161702 ) ) ;
#4227 = CARTESIAN_POINT ( 'NONE',  ( 22.82148508083511729, 43.16138278736985967, -17.87803012130492775 ) ) ;
#4228 = CARTESIAN_POINT ( 'NONE',  ( -208.1127848780264742, 15.00245453012665742, -40.00000000000002132 ) ) ;
#4229 = CARTESIAN_POINT ( 'NONE',  ( -56.48582580120559271, -9.153146818113595984, 0.000000000000000000 ) ) ;
#4230 = CARTESIAN_POINT ( 'NONE',  ( -3.675706741949858802, -43.24173023805415994, 17.91131112508043088 ) ) ;
#4231 = B_SPLINE_CURVE_WITH_KNOTS ( 'NONE', 3,
 ( #15197, #19693, #1481, #23444, #17692, #15692, #9082, #21197, #23817, #11080, #977, #19194 ),
 .UNSPECIFIED., .F., .F.,
 ( 4, 2, 2, 2, 2, 4 ),
 ( 1.471635563490154540E-15, 0.004698945756008183518, 0.007048418634011560137, 0.009397891512014935889, 0.01409683726802164749, 0.01879578302402835910 ),
 .UNSPECIFIED. ) ;
#4232 = CARTESIAN_POINT ( 'NONE',  ( -100.7734535825088358, 17.32597176626809343, 2.449293598294708485E-15 ) ) ;
#4233 = ORIENTED_EDGE ( 'NONE', *, *, #3689, .F. ) ;
#4234 = DIRECTION ( 'NONE',  ( -1.303213150798907793E-16, 1.000000000000000000, -1.682156097916904081E-16 ) ) ;
#4235 = CARTESIAN_POINT ( 'NONE',  ( 0.2972598230769990524, -18.14793986248724522, 38.42060263243662632 ) ) ;
#4236 = CARTESIAN_POINT ( 'NONE',  ( -7.297127544296671431, -13.59739983758519699, 45.86058602276306573 ) ) ;
#4237 = B_SPLINE_CURVE_WITH_KNOTS ( 'NONE', 3,
 ( #18504, #6795, #424, #14906, #6397, #20914 ),
 .UNSPECIFIED., .F., .F.,
 ( 4, 2, 4 ),
 ( 2.417129106265379096E-15, 0.03937685942888179830, 0.07875371885776118186 ),
 .UNSPECIFIED. ) ;
#4238 = CARTESIAN_POINT ( 'NONE',  ( -3.473570583883086371, 17.93385599103773487, -43.29615835920785116 ) ) ;
#4239 = CARTESIAN_POINT ( 'NONE',  ( 199.0181825105790665, -16.81808889125263207, -10.83063377519274795 ) ) ;
#4240 = CARTESIAN_POINT ( 'NONE',  ( -105.4741150117382773, -19.77569912955116749, -7.943527260750395946 ) ) ;
#4241 = DIRECTION ( 'NONE',  ( 0.000000000000000000, -0.6739498806388346530, -0.7387770694782699321 ) ) ;
#4242 = CARTESIAN_POINT ( 'NONE',  ( -174.2682069747356479, -16.26528465553954206, 39.26787081107618604 ) ) ;
#4243 = CARTESIAN_POINT ( 'NONE',  ( 91.82158438592158234, 16.11829626346161604, -16.11829626346121103 ) ) ;
#4244 = CARTESIAN_POINT ( 'NONE',  ( -91.56559293963836410, 22.67402823373189946, -0.000000000000000000 ) ) ;
#4246 = DIRECTION ( 'NONE',  ( -1.000000000000000000, -1.836970198721030181E-16, -0.000000000000000000 ) ) ;
#4245 = CARTESIAN_POINT ( 'NONE',  ( -188.4265466358252752, 23.47687925214783533, -43.04237830660004249 ) ) ;
#4247 = CARTESIAN_POINT ( 'NONE',  ( -259.2033419157646676, 21.55415060305790931, 35.01439189186571355 ) ) ;
#4248 = CARTESIAN_POINT ( 'NONE',  ( 200.0000000000000000, -19.99999999999988631, -40.00000000000002132 ) ) ;
#4249 = CARTESIAN_POINT ( 'NONE',  ( -105.3755690713226585, 18.24025645688350750, -40.00000000000002132 ) ) ;
#4250 = CARTESIAN_POINT ( 'NONE',  ( -213.1075012329537230, 1.045191102001431893E-13, -13.71589010951911902 ) ) ;
#4251 = CARTESIAN_POINT ( 'NONE',  ( 163.1118516004056573, -19.27778845539233998, 37.29075403953149959 ) ) ;
#4252 = CARTESIAN_POINT ( 'NONE',  ( -369.0000000000000568, -4.857225732735059864E-14, 0.000000000000000000 ) ) ;
#4253 = CARTESIAN_POINT ( 'NONE',  ( 0.2972598230770048811, -10.13633138497415942, -66.70487387989865624 ) ) ;
#4254 = ORIENTED_EDGE ( 'NONE', *, *, #17937, .F. ) ;
#4255 = CARTESIAN_POINT ( 'NONE',  ( 14.38125909742181285, -17.55144818341476309, 39.01709431150910490 ) ) ;
#4256 = CARTESIAN_POINT ( 'NONE',  ( -190.1935349183500534, -13.92226178597258723, -47.62328764229022227 ) ) ;
#4257 = VERTEX_POINT ( 'NONE', #14149 ) ;
#4258 = CARTESIAN_POINT ( 'NONE',  ( 0.2972598230770027716, -38.42060263243656237, -18.14793986248737667 ) ) ;
#4259 = CARTESIAN_POINT ( 'NONE',  ( 2.332272417551007226, -48.72342300852339037, -14.08759251167714943 ) ) ;
#4260 = ORIENTED_EDGE ( 'NONE', *, *, #704, .F. ) ;
#4261 = CARTESIAN_POINT ( 'NONE',  ( -88.39148973765023243, -20.15708830332361856, 8.027153355909467436 ) ) ;
#4262 = DIRECTION ( 'NONE',  ( -1.000000000000000000, 1.836970198721030181E-16, 0.000000000000000000 ) ) ;
#4263 = EDGE_CURVE ( 'NONE', #9693, #1336, #13824, .T. ) ;
#4264 = VECTOR ( 'NONE', #9995, 1000.000000000000000 ) ;
#4265 = VERTEX_POINT ( 'NONE', #10027 ) ;
#4266 = CARTESIAN_POINT ( 'NONE',  ( 199.9999999999998863, 17.10417011681778732, 8.282922153951966848 ) ) ;
#4267 = DIRECTION ( 'NONE',  ( 0.000000000000000000, 1.000000000000000000, 0.000000000000000000 ) ) ;
#4268 = CARTESIAN_POINT ( 'NONE',  ( 170.2234770963711128, -17.36149277826985937, -17.36149277826995174 ) ) ;
#4269 = CARTESIAN_POINT ( 'NONE',  ( -173.7925586253313668, -41.93433064649144626, -12.78856870755330633 ) ) ;
#4270 = CARTESIAN_POINT ( 'NONE',  ( 91.82158438592159655, -40.00000000000008527, 22.79471317813456110 ) ) ;
#4271 = CARTESIAN_POINT ( 'NONE',  ( 146.6084372240433709, -34.62501878078303008, 40.00000000000002132 ) ) ;
#4272 = CARTESIAN_POINT ( 'NONE',  ( 0.2972598230769990524, -18.14793986248671231, -38.42060263243687501 ) ) ;
#4273 = CARTESIAN_POINT ( 'NONE',  ( 199.0263771353516233, -14.14574067859894413, 14.14574067859863682 ) ) ;
#4274 = EDGE_CURVE ( 'NONE', #20612, #16255, #3895, .T. ) ;
#4275 = CARTESIAN_POINT ( 'NONE',  ( -238.4067589809705794, -40.00000000000021316, 40.96449427990166470 ) ) ;
#4276 = CARTESIAN_POINT ( 'NONE',  ( -135.8532207217289738, -40.00000000000014921, 30.84685318188631697 ) ) ;
#4277 = CARTESIAN_POINT ( 'NONE',  ( -198.0356074513804572, 39.99999999999992895, 15.37879056873084771 ) ) ;
#4278 = CARTESIAN_POINT ( 'NONE',  ( -208.1127848780264742, -15.00245453012673202, -40.00000000000002132 ) ) ;
#4279 = CARTESIAN_POINT ( 'NONE',  ( -162.0762913951020892, -57.76657433524000851, 1.198031840315820329 ) ) ;
#4280 = CARTESIAN_POINT ( 'NONE',  ( 0.2972598230770130412, -54.33493731733936016, -2.449293598294708485E-15 ) ) ;
#4281 = CARTESIAN_POINT ( 'NONE',  ( 136.1360204305621551, 24.77266263493108411, 31.79587985999273769 ) ) ;
#4282 = CARTESIAN_POINT ( 'NONE',  ( 128.5824617753800680, -11.99766463964393637, -28.96492468983277035 ) ) ;
#4283 = PRESENTATION_LAYER_ASSIGNMENT (  '', '', ( #15717 ) ) ;
#4284 = FACE_OUTER_BOUND ( 'NONE', #10394, .T. ) ;
#4285 = CARTESIAN_POINT ( 'NONE',  ( 91.82158438592156813, 39.99999999999986500, 17.20528682183341473 ) ) ;
#4286 = CARTESIAN_POINT ( 'NONE',  ( -238.4067589809705794, -1.892706720741712928E-13, 40.96449427998260973 ) ) ;
#4287 = CARTESIAN_POINT ( 'NONE',  ( -135.8532207217289738, 21.81201906317777883, -34.75652343174605363 ) ) ;
#4288 = CARTESIAN_POINT ( 'NONE',  ( -190.0000000000000000, -52.49999999999970868, 82.49999999999998579 ) ) ;
#4289 = CARTESIAN_POINT ( 'NONE',  ( -208.1127848780265026, 10.60833733269551615, -10.60833733269529766 ) ) ;
#4290 = CARTESIAN_POINT ( 'NONE',  ( -91.56559293963834989, -40.53558337403669753, -16.03295912088728770 ) ) ;
#4291 = EDGE_LOOP ( 'NONE', ( #12196, #25344, #12029, #20080 ) ) ;
#4292 = CARTESIAN_POINT ( 'NONE',  ( 4.995406935893294431, -17.50105314357144337, -39.06748935135212264 ) ) ;
#4293 = CARTESIAN_POINT ( 'NONE',  ( 98.29820294270297154, 18.47759065022021474, -7.653668647299666894 ) ) ;
#4294 = CARTESIAN_POINT ( 'NONE',  ( -238.4067589809705794, -40.96449427990185654, -40.00000000000002132 ) ) ;
#4295 = LINE ( 'NONE', #13845, #14879 ) ;
#4296 = FACE_BOUND ( 'NONE', #23610, .T. ) ;
#4297 = CARTESIAN_POINT ( 'NONE',  ( -198.9233928135198539, -14.16707757975730608, -49.24835219440220158 ) ) ;
#4298 = VERTEX_POINT ( 'NONE', #10298 ) ;
#4299 =( BOUNDED_SURFACE ( )  B_SPLINE_SURFACE ( 3, 2, ( 
 ( #22878, #12758, #16881 ),
 ( #25013, #2662, #18343 ),
 ( #8898, #794, #17008 ),
 ( #25146, #6897, #15014 ),
 ( #4793, #19016, #12895 ),
 ( #21009, #2791, #10904 ) ),
 .UNSPECIFIED., .F., .F., .F. ) 
 B_SPLINE_SURFACE_WITH_KNOTS ( ( 4, 2, 4 ),
 ( 3, 3 ),
 ( 0.04143177204414218162, 0.04845749460459651548, 0.05548321716505084933 ),
 ( 0.000000000000000000, 1.000000000000000000 ),
 .UNSPECIFIED. ) 
 GEOMETRIC_REPRESENTATION_ITEM ( )  RATIONAL_B_SPLINE_SURFACE ( (
 ( 1.000000000000000000, 0.9541700777564562364, 1.000000000000000000),
 ( 1.000000000000000000, 0.9520119497953954957, 1.000000000000000000),
 ( 1.000000000000000000, 0.9503149742541672218, 1.000000000000000000),
 ( 1.000000000000000000, 0.9480088400359243384, 1.000000000000000000),
 ( 1.000000000000000000, 0.9474362536298478465, 1.000000000000000000),
 ( 1.000000000000000000, 0.9474350312570024579, 1.000000000000000000) ) ) 
 REPRESENTATION_ITEM ( '' )  SURFACE ( )  );
#4300 = ORIENTED_EDGE ( 'NONE', *, *, #18004, .T. ) ;
#4301 = CARTESIAN_POINT ( 'NONE',  ( 200.0000000000000000, 6.097653648161206696, 18.01359495397503352 ) ) ;
#4302 = DIRECTION ( 'NONE',  ( -0.000000000000000000, -0.000000000000000000, 1.000000000000000000 ) ) ;
#4303 = CARTESIAN_POINT ( 'NONE',  ( 22.31419732600696904, 17.93420418956782214, 43.29699898481114673 ) ) ;
#4304 = EDGE_LOOP ( 'NONE', ( #18143, #20206, #24312, #4993, #6022, #2413, #20180, #22349, #2826 ) ) ;
#4305 = EDGE_CURVE ( 'NONE', #20514, #7340, #18405, .T. ) ;
#4306 = ORIENTED_EDGE ( 'NONE', *, *, #13609, .T. ) ;
#4307 = CARTESIAN_POINT ( 'NONE',  ( -91.56559293963834989, -22.67402823373193499, 0.000000000000000000 ) ) ;
#4308 = CARTESIAN_POINT ( 'NONE',  ( 199.0137359473271488, -10.84478214295758036, -16.80398351328055639 ) ) ;
#4309 = FACE_OUTER_BOUND ( 'NONE', #6498, .T. ) ;
#4310 = ADVANCED_FACE ( 'NONE', ( #180 ), #6990, .T. ) ;
#4311 = EDGE_CURVE ( 'NONE', #17229, #17458, #401, .T. ) ;
#4312 = CARTESIAN_POINT ( 'NONE',  ( -96.94475454968227268, -8.190683501865384741, -20.92018922312004037 ) ) ;
#4313 = CARTESIAN_POINT ( 'NONE',  ( 0.2972598230769956662, 40.00000000000058975, -54.33493731733894094 ) ) ;
#4314 = CARTESIAN_POINT ( 'NONE',  ( 199.9999999999999432, -1.727494763561684666E-13, 20.00000000000010303 ) ) ;
#4315 = CARTESIAN_POINT ( 'NONE',  ( -649.7157619631484522, 34.88051882544941407, 19.58372711145630518 ) ) ;
#4316 = DIRECTION ( 'NONE',  ( 1.000000000000000000, 0.000000000000000000, 0.000000000000000000 ) ) ;
#4317 = CARTESIAN_POINT ( 'NONE',  ( 199.0145894300637792, 15.86095929198710586, 12.18642508278280623 ) ) ;
#4318 = CARTESIAN_POINT ( 'NONE',  ( -191.2489946134182901, 18.16428294930770093, 43.85245824700565720 ) ) ;
#4319 = CARTESIAN_POINT ( 'NONE',  ( 136.1360204305621266, -3.511608612530630058, -3.511608612530719764 ) ) ;
#4320 = CARTESIAN_POINT ( 'NONE',  ( -102.4068193528145088, 20.17396017424893984, -8.735227608997000459 ) ) ;
#4321 = CARTESIAN_POINT ( 'NONE',  ( -30.26275506840325136, 27.08623969584573388, 29.48230279907808793 ) ) ;
#4322 = CARTESIAN_POINT ( 'NONE',  ( -77.59261320673972762, 2.779275804817392448, 21.93453874213112087 ) ) ;
#4323 = CARTESIAN_POINT ( 'NONE',  ( 146.6084372240433709, 52.76785682606523409, -3.800685668858194255 ) ) ;
#4324 = CARTESIAN_POINT ( 'NONE',  ( -280.0000000000000000, 19.99999999999996092, -0.000000000000000000 ) ) ;
#4325 = CARTESIAN_POINT ( 'NONE',  ( -135.8532207217289738, -6.472252184284280396, 6.472252184284099208 ) ) ;
#4326 = CIRCLE ( 'NONE', #20006, 15.00000000000000178 ) ;
#4327 = CARTESIAN_POINT ( 'NONE',  ( -280.0000000000000568, 19.99999999999996092, 40.00000000000002132 ) ) ;
#4328 = CARTESIAN_POINT ( 'NONE',  ( -93.02511667906875914, 20.82219708225684940, -8.169918093965478079 ) ) ;
#4329 = CARTESIAN_POINT ( 'NONE',  ( 130.8568914410475088, 39.99999999999969447, 34.05028731879830417 ) ) ;
#4330 = CARTESIAN_POINT ( 'NONE',  ( -280.0000000000000000, -14.14213562373098831, -14.14213562373098654 ) ) ;
#4331 = CARTESIAN_POINT ( 'NONE',  ( 14.38125909742180752, 15.17850393972634038, 0.000000000000000000 ) ) ;
#4332 = ORIENTED_EDGE ( 'NONE', *, *, #880, .T. ) ;
#4333 = EDGE_LOOP ( 'NONE', ( #14082, #26052, #5291, #11582 ) ) ;
#4334 = CARTESIAN_POINT ( 'NONE',  ( 192.4448373802100889, -20.00000000003938538, 0.000000000000000000 ) ) ;
#4335 = CARTESIAN_POINT ( 'NONE',  ( -100.0753760173602700, -8.149786832858715968, -20.72827493166402135 ) ) ;
#4336 = CARTESIAN_POINT ( 'NONE',  ( 200.0000000000000000, 42.42640687119267540, 14.14213562373153543 ) ) ;
#4337 = DIRECTION ( 'NONE',  ( -1.000000000000000000, 0.000000000000000000, 0.000000000000000000 ) ) ;
#4338 =( BOUNDED_CURVE ( )  B_SPLINE_CURVE ( 3, ( #1130, #6839, #12968, #15085, #14821, #14959, #10980 ),
 .UNSPECIFIED., .F., .F. ) 
 B_SPLINE_CURVE_WITH_KNOTS ( ( 4, 3, 4 ),
 ( 0.0006517261993840123800, 0.02240322356231545103, 0.03884882555987133335 ),
 .UNSPECIFIED. ) 
 CURVE ( )  GEOMETRIC_REPRESENTATION_ITEM ( )  RATIONAL_B_SPLINE_CURVE ( ( 0.5249926329037828410, 0.5828554938567718224, 0.7411912828888442828, 1.000000000000000000, 0.8043231192735467161, 0.6660804010233453143, 0.5852718452493959056 ) ) 
 REPRESENTATION_ITEM ( '' )  );
#4339 = CARTESIAN_POINT ( 'NONE',  ( -716.9846540392142060, -66.50000000000001421, 71.50000000000005684 ) ) ;
#4340 = CARTESIAN_POINT ( 'NONE',  ( 199.9999999999998863, -5.231270638550959085, -18.27112563740264761 ) ) ;
#4341 = CARTESIAN_POINT ( 'NONE',  ( 199.9999999999999716, 9.498725063112413380, -16.45837312633763005 ) ) ;
#4342 = CARTESIAN_POINT ( 'NONE',  ( -213.1075012329537230, -18.58567234101102272, -37.98287015391260013 ) ) ;
#4343 = CARTESIAN_POINT ( 'NONE',  ( -135.8532207217289738, -21.81201906317806305, 34.75652343174590442 ) ) ;
#4344 = CARTESIAN_POINT ( 'NONE',  ( -105.4113873279013660, 20.16970153814047961, 7.043304828828932607 ) ) ;
#4345 = CARTESIAN_POINT ( 'NONE',  ( 91.82158438592156813, 40.00000000000027711, -22.79471317813428044 ) ) ;
#4346 = CARTESIAN_POINT ( 'NONE',  ( 4.995406935893297984, -39.06748935135205869, 17.50105314357158193 ) ) ;
#4347 = CARTESIAN_POINT ( 'NONE',  ( 169.9999999999999716, -115.7889608577475258, 82.50000000000001421 ) ) ;
#4348 = CARTESIAN_POINT ( 'NONE',  ( -138.9613193425346651, -13.65853114850577121, -27.95779829453082499 ) ) ;
#4349 = CARTESIAN_POINT ( 'NONE',  ( -91.56559293963834989, -40.53558337403669753, -16.03295912088728770 ) ) ;
#4350 = CARTESIAN_POINT ( 'NONE',  ( 199.0255859347418834, -7.628281087858428400, 18.49319637005222816 ) ) ;
#4352 = CARTESIAN_POINT ( 'NONE',  ( -259.2033419157646676, -1.564921101325656229E-13, 30.48217210827739621 ) ) ;
#4351 = CARTESIAN_POINT ( 'NONE',  ( -280.0000000000000568, -14.14213562373049449, -42.42640687119305198 ) ) ;
#4353 = CARTESIAN_POINT ( 'NONE',  ( 184.8905102610680444, 41.77492675555983936, 14.79361573936436081 ) ) ;
#4354 = AXIS2_PLACEMENT_3D ( 'NONE', #5482, #11211, #21208 ) ;
#4355 = CARTESIAN_POINT ( 'NONE',  ( 25.05785482530196617, 42.53113694082225038, -17.61697374401517990 ) ) ;
#4356 = CARTESIAN_POINT ( 'NONE',  ( 130.8568914410475088, 5.949712681206719367, -40.00000000000002132 ) ) ;
#4357 = CARTESIAN_POINT ( 'NONE',  ( 163.1118516004056573, 27.26290988616875310, 0.000000000000000000 ) ) ;
#4358 = CARTESIAN_POINT ( 'NONE',  ( 18.89824403360313454, -24.18164459663342214, -43.99464769172848122 ) ) ;
#4359 = B_SPLINE_CURVE_WITH_KNOTS ( 'NONE', 3,
 ( #24552, #22427, #20288, #4335, #4202, #10174, #8034, #2067, #12295, #18278, #2324, #63 ),
 .UNSPECIFIED., .F., .F.,
 ( 4, 2, 2, 2, 2, 4 ),
 ( 1.695971460814453879E-15, 0.004698945756008356123, 0.007048418634011665955, 0.009397891512014975787, 0.01409683726802159545, 0.01879578302402821338 ),
 .UNSPECIFIED. ) ;
#4360 = CARTESIAN_POINT ( 'NONE',  ( -3.977426076247516207, -43.16039317622677629, 17.87762021094849274 ) ) ;
#4361 = CARTESIAN_POINT ( 'NONE',  ( -91.56559293963834989, 17.32597176626808988, 40.00000000000002132 ) ) ;
#4362 = VERTEX_POINT ( 'NONE', #4681 ) ;
#4363 = CARTESIAN_POINT ( 'NONE',  ( 22.89172254855150257, 23.44749030158443048, -43.00256445985473164 ) ) ;
#4364 = CARTESIAN_POINT ( 'NONE',  ( 91.82158438592158234, -12.16597498397761967, -12.16597498397768007 ) ) ;
#4365 = DIRECTION ( 'NONE',  ( 1.000000000000000000, 1.836970198721030181E-16, -0.000000000000000000 ) ) ;
#4366 = EDGE_CURVE ( 'NONE', #18580, #16641, #9577, .T. ) ;
#4367 = CARTESIAN_POINT ( 'NONE',  ( 3.869409319519631296, 24.63759630012732060, -44.61273074174879838 ) ) ;
#4368 = CARTESIAN_POINT ( 'NONE',  ( 199.0152737994447136, -13.19951906643276374, -15.03942049639883294 ) ) ;
#4369 = CARTESIAN_POINT ( 'NONE',  ( -135.8532207217289738, -1.208299557080134822E-13, 9.153146818113572891 ) ) ;
#4370 = CARTESIAN_POINT ( 'NONE',  ( 210.0000000000000284, 71.50000000000009948, -66.50000000000005684 ) ) ;
#4371 = CARTESIAN_POINT ( 'NONE',  ( -188.9524938556157281, -13.86227398172938230, 47.22059665006405282 ) ) ;
#4372 = CARTESIAN_POINT ( 'NONE',  ( 170.2234770963711128, -17.36149277826940462, -39.20704971665412586 ) ) ;
#4373 = CARTESIAN_POINT ( 'NONE',  ( -105.2274517607667974, 13.17594969605270627, -17.01575307708425200 ) ) ;
#4375 = CARTESIAN_POINT ( 'NONE',  ( -91.56559293963834989, 12.25131212657428748, 44.31723036834913643 ) ) ;
#4374 = CARTESIAN_POINT ( 'NONE',  ( -188.4702232936790836, 23.48628015403081193, -43.05505437950374414 ) ) ;
#4376 = CARTESIAN_POINT ( 'NONE',  ( 57.59792236341147031, 26.56190807104652052, 30.00663442387728708 ) ) ;
#4377 = CARTESIAN_POINT ( 'NONE',  ( 4.995406935893307754, -55.24977328853207581, -40.00000000000002132 ) ) ;
#4378 = CARTESIAN_POINT ( 'NONE',  ( 170.2234770963711128, 15.44714144992818738, 40.00000000000002132 ) ) ;
#4379 = CARTESIAN_POINT ( 'NONE',  ( 14.38125909742181108, 1.616281842095393922E-13, -15.17850393972633682 ) ) ;
#4380 = CARTESIAN_POINT ( 'NONE',  ( -135.8532207217289738, 21.81201906317767936, 21.81201906317778239 ) ) ;
#4381 = CARTESIAN_POINT ( 'NONE',  ( -86.86493150571118349, 19.60045294882759137, -8.366608963953964917 ) ) ;
#4382 = CARTESIAN_POINT ( 'NONE',  ( 136.1360204305621551, 24.77266263493153176, -31.79587985999237887 ) ) ;
#4383 = CARTESIAN_POINT ( 'NONE',  ( 0.2972598230769976091, -10.13633138497479180, 10.13633138497468522 ) ) ;
#4385 = ORIENTED_EDGE ( 'NONE', *, *, #6535, .F. ) ;
#4384 = B_SPLINE_CURVE_WITH_KNOTS ( 'NONE', 3,
 ( #21596, #15590, #25478, #17850, #1508, #15345, #5496, #9483, #3766, #17719, #19463, #17587, #19594, #7605, #15719, #17464, #13863, #21856, #19856, #11737, #1642, #26000, #1251, #23978, #9355, #25607, #7350, #15463, #23590, #5369 ),
 .UNSPECIFIED., .F., .F.,
 ( 4, 2, 2, 2, 2, 2, 2, 2, 2, 2, 2, 2, 2, 2, 4 ),
 ( 0.000000000000000000, 0.1357259735107005372, 0.1651108541090157700, 0.1944957347073310028, 0.3598804999793158710, 0.3867117631979620773, 0.4135430264166082281, 0.5789277916885930964, 0.6062785021374117456, 0.6336292125862302838, 0.8508620842112317728, 0.8814014469398914198, 0.9119408096685510667, 0.9559704048342755334, 0.9980677081714144361 ),
 .UNSPECIFIED. ) ;
#4386 = CARTESIAN_POINT ( 'NONE',  ( -100.7734535825088358, -16.03295912088706743, -16.03295912088710296 ) ) ;
#4387 = CARTESIAN_POINT ( 'NONE',  ( -89.91498783734833466, 8.733585468302273114, 20.17141720476648814 ) ) ;
#4388 = CARTESIAN_POINT ( 'NONE',  ( -91.56559293963834989, 16.03295912088683650, 40.53558337403684675 ) ) ;
#4389 = CARTESIAN_POINT ( 'NONE',  ( -4.022465846214378971, -46.99661175925217549, -13.82902411340760196 ) ) ;
#4390 = ORIENTED_EDGE ( 'NONE', *, *, #25827, .T. ) ;
#4391 = CARTESIAN_POINT ( 'NONE',  ( -105.4741150117369273, 8.366608964608960974, -19.60045294982168329 ) ) ;
#4392 = CARTESIAN_POINT ( 'NONE',  ( -77.55640685876515761, -15.64922766773197260, -15.64922766773223550 ) ) ;
#4393 = ORIENTED_EDGE ( 'NONE', *, *, #23125, .F. ) ;
#4394 = CARTESIAN_POINT ( 'NONE',  ( 199.9999999999998579, 18.23094931701148269, -5.355502299499542040 ) ) ;
#4395 = CARTESIAN_POINT ( 'NONE',  ( -114.7823189589618380, -22.12960287296361273, -1.412059986351657637 ) ) ;
#4396 = CARTESIAN_POINT ( 'NONE',  ( -192.1964066538670863, -43.96877160662432260, -24.16259023441631371 ) ) ;
#4397 = CARTESIAN_POINT ( 'NONE',  ( 0.2972598230770103767, -40.00000000000021316, 54.33493731733921805 ) ) ;
#4398 = CARTESIAN_POINT ( 'NONE',  ( 130.8568914410475372, 5.949712681206715814, 2.449293598294708485E-15 ) ) ;
#4399 = CARTESIAN_POINT ( 'NONE',  ( 184.8905102610680444, -14.79361573936399665, 14.79361573936367158 ) ) ;
#4400 = CARTESIAN_POINT ( 'NONE',  ( 199.0242446922718784, -2.616032970993653173, 19.83497009005848710 ) ) ;
#4401 = CARTESIAN_POINT ( 'NONE',  ( -259.2033419157646676, -1.564921101325656229E-13, 30.48217210827739621 ) ) ;
#4402 = CARTESIAN_POINT ( 'NONE',  ( -105.3755690713226585, 40.00000000000007816, -21.75974354311636461 ) ) ;
#4403 = CARTESIAN_POINT ( 'NONE',  ( -4.039451493210490796, 46.99046209229823745, -13.82811171175438147 ) ) ;
#4404 = CARTESIAN_POINT ( 'NONE',  ( -198.0356074513804572, -15.37879056873074290, 0.000000000000000000 ) ) ;
#4405 = CARTESIAN_POINT ( 'NONE',  ( -198.0356074513804572, -55.37879056874826489, 40.00000000000002132 ) ) ;
#4406 = CARTESIAN_POINT ( 'NONE',  ( -192.9588430854690273, 18.05360324515418924, 38.51493924976949756 ) ) ;
#4407 = CARTESIAN_POINT ( 'NONE',  ( -91.56559293963834989, -2.543181659092656077E-13, 22.67402823373191723 ) ) ;
#4408 = CARTESIAN_POINT ( 'NONE',  ( -188.2995950289364657, -23.44932284466040784, 43.00522595870950937 ) ) ;
#4409 = CARTESIAN_POINT ( 'NONE',  ( -259.2033419157646676, 2.741182173978444749E-13, -30.48217210827739621 ) ) ;
#4410 = CARTESIAN_POINT ( 'NONE',  ( 91.82158438592158234, -6.516925787240506436E-14, 22.79471317813470321 ) ) ;
#4411 = CARTESIAN_POINT ( 'NONE',  ( 170.2234770963711128, -17.36149277826985937, -17.36149277826995174 ) ) ;
#4412 = DIRECTION ( 'NONE',  ( 0.000000000000000000, 1.000000000000000000, 0.000000000000000000 ) ) ;
#4413 = CARTESIAN_POINT ( 'NONE',  ( -135.8532207217289738, -6.472252184284280396, 6.472252184284099208 ) ) ;
#4414 = CARTESIAN_POINT ( 'NONE',  ( -238.4067589809705794, -57.25054294065807881, 0.6820004457338858517 ) ) ;
#4415 = ORIENTED_EDGE ( 'NONE', *, *, #8905, .T. ) ;
#4416 = CARTESIAN_POINT ( 'NONE',  ( -8.720657192080711440, 41.62108041047287799, -22.53512351407914593 ) ) ;
#4417 = CARTESIAN_POINT ( 'NONE',  ( -4.039451493210483690, -23.44932283416618191, -43.00522595894033628 ) ) ;
#4418 = CARTESIAN_POINT ( 'NONE',  ( -192.9588430854690273, -54.46834944101725284, -40.00000000000002132 ) ) ;
#4419 = CARTESIAN_POINT ( 'NONE',  ( -87.13361725327072804, -21.49321519333430786, -1.371494219583687668 ) ) ;
#4420 = CARTESIAN_POINT ( 'NONE',  ( -162.0762913951020892, 1.694272876828294194, 0.000000000000000000 ) ) ;
#4421 =( NAMED_UNIT ( * ) PLANE_ANGLE_UNIT ( ) SI_UNIT ( $, .RADIAN. ) );
#4422 = ORIENTED_EDGE ( 'NONE', *, *, #2584, .T. ) ;
#4423 = ORIENTED_EDGE ( 'NONE', *, *, #23315, .T. ) ;
#4424 = CARTESIAN_POINT ( 'NONE',  ( 200.0000000000000284, 4.307699855108636733, 18.51410484079663377 ) ) ;
#4425 = CARTESIAN_POINT ( 'NONE',  ( 125.5832160019860169, 11.61997419108396734, -28.05309928653990781 ) ) ;
#4426 = CARTESIAN_POINT ( 'NONE',  ( 22.66553228237577855, 17.89571368754772607, 43.20407469282439905 ) ) ;
#4427 = ORIENTED_EDGE ( 'NONE', *, *, #5571, .F. ) ;
#4428 = VERTEX_POINT ( 'NONE', #16642 ) ;
#4429 = CARTESIAN_POINT ( 'NONE',  ( -56.48582580120559982, -34.75652343174615311, 21.81201906317766870 ) ) ;
#4430 = CARTESIAN_POINT ( 'NONE',  ( 199.0232879746372134, -20.00360196692749071, -0.1645009869758431997 ) ) ;
#4431 = DIRECTION ( 'NONE',  ( 0.000000000000000000, 1.000000000000000000, 0.000000000000000000 ) ) ;
#4432 = DIRECTION ( 'NONE',  ( 0.000000000000000000, 0.9166903767332116315, -0.3995982397417718879 ) ) ;
#4433 = CARTESIAN_POINT ( 'NONE',  ( 170.2234770963711128, 10.92277846919201068, 10.92277846919202133 ) ) ;
#4434 = CARTESIAN_POINT ( 'NONE',  ( -199.9999999999999432, -24.32899771311792136, 44.86773131993664521 ) ) ;
#4435 = CARTESIAN_POINT ( 'NONE',  ( -626.9846540392142060, 95.00000000000000000, 0.000000000000000000 ) ) ;
#4436 = CARTESIAN_POINT ( 'NONE',  ( 200.0000000000000000, 39.99999999999985079, 20.00000000000052225 ) ) ;
#4437 = CARTESIAN_POINT ( 'NONE',  ( 170.2234770963711128, 39.99999999999980105, 24.55285855007229401 ) ) ;
#4438 = CARTESIAN_POINT ( 'NONE',  ( -656.2662938234084322, 39.46402985900065374, 6.545868711047839739 ) ) ;
#4439 = CYLINDRICAL_SURFACE ( 'NONE', #5169, 74.99999999999995737 ) ;
#4440 = CARTESIAN_POINT ( 'NONE',  ( 199.0089741461167989, 19.95552976068599804, 1.321036586804004820 ) ) ;
#4441 = CARTESIAN_POINT ( 'NONE',  ( -187.3036811847890419, 23.25512365539898596, 42.71162014090150905 ) ) ;
#4442 = CARTESIAN_POINT ( 'NONE',  ( 57.59792236341147031, 1.722363176415040886, 1.722363176415060426 ) ) ;
#4443 = EDGE_CURVE ( 'NONE', #916, #3826, #2545, .T. ) ;
#4444 = CARTESIAN_POINT ( 'NONE',  ( -200.0000000000000568, 21.40989205436302711, 45.24754806068986568 ) ) ;
#4445 = CARTESIAN_POINT ( 'NONE',  ( -238.4067589809705794, -0.6820004458488042598, 57.25054294077229855 ) ) ;
#4446 = DIRECTION ( 'NONE',  ( 0.000000000000000000, -1.000000000000000000, 0.000000000000000000 ) ) ;
#4447 = CARTESIAN_POINT ( 'NONE',  ( -100.7734535825088500, 44.31723036834907958, -12.25131212657445801 ) ) ;
#4448 = DIRECTION ( 'NONE',  ( -1.000000000000000000, -1.836970198721030181E-16, -2.465190328815661892E-32 ) ) ;
#4449 = CARTESIAN_POINT ( 'NONE',  ( 4.995406935893293543, -15.24977328854832592, 0.000000000000000000 ) ) ;
#4450 = ADVANCED_FACE ( 'NONE', ( #6524 ), #15995, .T. ) ;
#4451 = CARTESIAN_POINT ( 'NONE',  ( -162.0762913951021176, 29.48230308784730980, 27.08623940707652622 ) ) ;
#4452 = CARTESIAN_POINT ( 'NONE',  ( -86.96347745069645896, 21.75974354311648895, 40.00000000000002132 ) ) ;
#4453 = CARTESIAN_POINT ( 'NONE',  ( -598.8194166445492783, 39.91519017297324723, -20.78534762901812272 ) ) ;
#4454 = CARTESIAN_POINT ( 'NONE',  ( 163.1118516004056573, 39.99999999999976552, 27.26290988616914746 ) ) ;
#4455 = ADVANCED_FACE ( 'NONE', ( #8709 ), #5983, .T. ) ;
#4456 = CARTESIAN_POINT ( 'NONE',  ( 199.0061375790170644, 7.656915158548016187, -18.47094169875700942 ) ) ;
#4457 = EDGE_CURVE ( 'NONE', #1425, #2455, #2326, .T. ) ;
#4458 = CARTESIAN_POINT ( 'NONE',  ( -200.0000000000000000, 66.50000000000009948, 66.50000000000005684 ) ) ;
#4459 = EDGE_LOOP ( 'NONE', ( #13810, #22818, #22074, #18648 ) ) ;
#4460 = VERTEX_POINT ( 'NONE', #4464 ) ;
#4461 = CARTESIAN_POINT ( 'NONE',  ( 163.1118516004056573, -27.26290988616869626, 40.00000000000002132 ) ) ;
#4462 = FILL_AREA_STYLE ('',( #16153 ) ) ;
#4463 = CARTESIAN_POINT ( 'NONE',  ( 4.995406935893290878, 39.06748935135239265, -39.06748935135144762 ) ) ;
#4464 = CARTESIAN_POINT ( 'NONE',  ( -626.9846540392142060, 75.00000000000000000, 74.99999999999991473 ) ) ;
#4465 = CARTESIAN_POINT ( 'NONE',  ( -198.0012279374157629, -44.79720170867064155, -24.77357825033872629 ) ) ;
#4466 = DIRECTION ( 'NONE',  ( -1.000000000000000000, -1.836970198721030181E-16, 0.000000000000000000 ) ) ;
#4467 = CARTESIAN_POINT ( 'NONE',  ( 199.9999999999999147, -6.121038220875967717, -17.99280653461927315 ) ) ;
#4468 = CARTESIAN_POINT ( 'NONE',  ( 200.0000000000000000, -61.50000000000001421, 66.50000000000005684 ) ) ;
#4469 = CARTESIAN_POINT ( 'NONE',  ( 14.38125909742181285, -17.55144818341421598, -39.01709431150935359 ) ) ;
#4470 = FACE_BOUND ( 'NONE', #8196, .T. ) ;
#4471 = CARTESIAN_POINT ( 'NONE',  ( -86.96347745069645896, 40.00000000000019895, -18.24025645688310249 ) ) ;
#4472 = CARTESIAN_POINT ( 'NONE',  ( 14.38125909742181285, -10.73282306404712472, -10.73282306404731301 ) ) ;
#4473 = CARTESIAN_POINT ( 'NONE',  ( 151.7948205124836250, 33.23291073765556547, 0.000000000000000000 ) ) ;
#4474 = CARTESIAN_POINT ( 'NONE',  ( -163.5815439473252866, -18.59457101086894681, -35.61501074501018849 ) ) ;
#4475 = CARTESIAN_POINT ( 'NONE',  ( -208.1127848780264742, -38.89260858015728672, -17.67593391476669851 ) ) ;
#4476 = CARTESIAN_POINT ( 'NONE',  ( 199.0117673552712745, 18.58883966351390526, 7.374690901580303937 ) ) ;
#4478 = CARTESIAN_POINT ( 'NONE',  ( 151.7948205124836534, -40.00000000000001421, 6.767089262348889633 ) ) ;
#4477 = CARTESIAN_POINT ( 'NONE',  ( 199.9999999999999432, 14.14213562373110911, -14.14213562373072364 ) ) ;
#4479 =( GEOMETRIC_REPRESENTATION_CONTEXT ( 3 ) GLOBAL_UNCERTAINTY_ASSIGNED_CONTEXT ( ( #21345 ) ) GLOBAL_UNIT_ASSIGNED_CONTEXT ( ( #8933, #24908, #426 ) ) REPRESENTATION_CONTEXT ( 'NONE', 'WORKASPACE' ) );
#4480 = CARTESIAN_POINT ( 'NONE',  ( 4.995406935893283773, 39.06748935135171052, 17.50105314357239195 ) ) ;
#4481 = CARTESIAN_POINT ( 'NONE',  ( 22.66553228237832585, 43.20407469282481827, -17.89571368754818081 ) ) ;
#4482 = CARTESIAN_POINT ( 'NONE',  ( -280.0000000000000568, 19.99999999999996447, -40.00000000000002132 ) ) ;
#4483 = CARTESIAN_POINT ( 'NONE',  ( -213.1075012329537230, -13.71589010951915810, 0.000000000000000000 ) ) ;
#4484 = CARTESIAN_POINT ( 'NONE',  ( -213.1075012329537230, 53.71589010953660193, 40.00000000000002132 ) ) ;
#4485 = B_SPLINE_CURVE_WITH_KNOTS ( 'NONE', 3,
 ( #23479, #11477, #1391, #11356, #7488, #19472 ),
 .UNSPECIFIED., .F., .F.,
 ( 4, 2, 4 ),
 ( -0.0001324603514699870008, 0.04003639359265966785, 0.08020524753678931473 ),
 .UNSPECIFIED. ) ;
#4486 = CARTESIAN_POINT ( 'NONE',  ( -4.339409867971073531, -43.06267456183169173, 17.83714383556879923 ) ) ;
#4487 = CARTESIAN_POINT ( 'NONE',  ( -100.7734535825088500, 17.32597176626808988, 40.00000000000002132 ) ) ;
#4488 = EDGE_LOOP ( 'NONE', ( #15103, #19715, #16978, #18514 ) ) ;
#4489 = CARTESIAN_POINT ( 'NONE',  ( -199.9999999999999147, 46.69454133506851434, 26.45173932753578683 ) ) ;
#4490 = DIRECTION ( 'NONE',  ( -1.000000000000000000, 0.000000000000000000, 0.000000000000000000 ) ) ;
#4491 = CARTESIAN_POINT ( 'NONE',  ( -4.076660308449226555, -13.82548859978938260, 46.97758120990467035 ) ) ;
#4492 = CARTESIAN_POINT ( 'NONE',  ( 6.984886629811533076, 24.81009931999678031, -44.84679502273271368 ) ) ;
#4493 = CARTESIAN_POINT ( 'NONE',  ( 199.0223302282441296, -19.84245377806801613, -2.613091800807908260 ) ) ;
#4494 = CARTESIAN_POINT ( 'NONE',  ( 136.1360204305621266, -24.77266263493151044, 24.77266263493093135 ) ) ;
#4495 = DIRECTION ( 'NONE',  ( 1.000000000000000000, 1.303213150798907793E-16, 2.465190328815661892E-32 ) ) ;
#4496 = FACE_OUTER_BOUND ( 'NONE', #3080, .T. ) ;
#4497 = CARTESIAN_POINT ( 'NONE',  ( -188.8842637254074646, -17.93596642850445733, 43.30125340596327987 ) ) ;
#4498 = CARTESIAN_POINT ( 'NONE',  ( 170.2234770963711128, -40.00000000000024158, 24.55285855007145202 ) ) ;
#4499 = CARTESIAN_POINT ( 'NONE',  ( 130.8568914410475088, -24.07718906446864793, -32.49135343045505664 ) ) ;
#4500 = CARTESIAN_POINT ( 'NONE',  ( 130.8568914410475372, 34.05028731879791337, 0.000000000000000000 ) ) ;
#4501 = VECTOR ( 'NONE', #17086, 1000.000000000000000 ) ;
#4502 = AXIS2_PLACEMENT_3D ( 'NONE', #5106, #5352, #13211 ) ;
#4504 = CARTESIAN_POINT ( 'NONE',  ( 184.8905102610680444, 41.77492675555983936, 14.79361573936436081 ) ) ;
#4503 = CARTESIAN_POINT ( 'NONE',  ( -215.0000000000000284, 72.72568232011437317, -59.67546976104961942 ) ) ;
#4505 = CARTESIAN_POINT ( 'NONE',  ( 170.2234770963711128, 10.92277846919147066, 45.64576402573197811 ) ) ;
#4506 = CARTESIAN_POINT ( 'NONE',  ( 163.1118516004056573, -12.73709011382472234, -2.449293598294708485E-15 ) ) ;
#4507 = CARTESIAN_POINT ( 'NONE',  ( 163.1118516004056573, 12.73709011382477918, 40.00000000000002132 ) ) ;
#4508 = CARTESIAN_POINT ( 'NONE',  ( 184.8905102610680444, -40.00000000000021316, 20.92133201514402430 ) ) ;
#4509 = CARTESIAN_POINT ( 'NONE',  ( -208.1127848780265026, 10.60833733269537049, 10.60833733269544510 ) ) ;
#4510 = DIRECTION ( 'NONE',  ( 1.000000000000000000, 0.000000000000000000, 0.000000000000000000 ) ) ;
#4511 = CARTESIAN_POINT ( 'NONE',  ( 57.59792236341148453, 1.722363176415528940, -54.84617931850878136 ) ) ;
#4512 = CARTESIAN_POINT ( 'NONE',  ( -114.4364955367327354, 8.064892380842190178, 20.29001642038852182 ) ) ;
#4513 = VERTEX_POINT ( 'NONE', #12558 ) ;
#4514 = AXIS2_PLACEMENT_3D ( 'NONE', #15403, #23528, #7161 ) ;
#4515 = CARTESIAN_POINT ( 'NONE',  ( -86.96347745069644475, -15.38646221621786125, -15.38646221621789856 ) ) ;
#4516 = AXIS2_PLACEMENT_3D ( 'NONE', #7888, #18267, #14015 ) ;
#4517 = CARTESIAN_POINT ( 'NONE',  ( 170.0000000000000000, -2.301191124287261779E-13, 24.95097643317000546 ) ) ;
#4518 = ITEM_DEFINED_TRANSFORMATION ( 'NONE', 'NONE', #26153,  #21058 ) ;
#4519 = AXIS2_PLACEMENT_3D ( 'NONE', #17420, #19548, #17545 ) ;
#4520 = EDGE_CURVE ( 'NONE', #2760, #1888, #11698, .T. ) ;
#4521 = CARTESIAN_POINT ( 'NONE',  ( -86.96347745069643054, 15.38646221621763210, 41.18208027870604582 ) ) ;
#4522 = CARTESIAN_POINT ( 'NONE',  ( -3.966425590329097250, -43.02666064534183477, -23.46521855348083463 ) ) ;
#4523 = ORIENTED_EDGE ( 'NONE', *, *, #2841, .T. ) ;
#4524 = CARTESIAN_POINT ( 'NONE',  ( -86.96347745069644475, -21.75974354311651737, 0.000000000000000000 ) ) ;
#4525 = CARTESIAN_POINT ( 'NONE',  ( -77.78738185796684945, -9.951839775390311615, -19.58912165101554592 ) ) ;
#4526 = EDGE_LOOP ( 'NONE', ( #6023, #12931 ) ) ;
#4527 = CARTESIAN_POINT ( 'NONE',  ( 200.0000000000001137, 15.89309473284322749, -10.41337480477382371 ) ) ;
#4528 = CLOSED_SHELL ( 'NONE', ( #22740, #10620, #25086, #15305, #15945, #11187, #4861, #24012, #4918 ) ) ;
#4529 = DIRECTION ( 'NONE',  ( 0.000000000000000000, -1.000000000000000000, 0.000000000000000000 ) ) ;
#4530 = CARTESIAN_POINT ( 'NONE',  ( 184.8905102610680444, 19.07866798485561333, 40.00000000000002132 ) ) ;
#4531 = CARTESIAN_POINT ( 'NONE',  ( 130.8568914410475088, -52.36146031193413108, -4.207082182990267150 ) ) ;
#4532 = CARTESIAN_POINT ( 'NONE',  ( 199.0093797572272081, 19.86600527971208763, 2.306481033292959726 ) ) ;
#4533 = AXIS2_PLACEMENT_3D ( 'NONE', #3557, #11401, #19524 ) ;
#4534 = CARTESIAN_POINT ( 'NONE',  ( 4.995406935893312195, -67.35176059882525124, -10.78321810390210445 ) ) ;
#4535 = CARTESIAN_POINT ( 'NONE',  ( -259.2033419157646676, 39.99999999999987210, 30.48217210827754542 ) ) ;
#4536 = CARTESIAN_POINT ( 'NONE',  ( 14.38125909742180930, 39.99999999999982947, 55.17850393971022527 ) ) ;
#4537 = CARTESIAN_POINT ( 'NONE',  ( 151.7948205124836250, 1.439163438361279259E-13, -33.23291073765553705 ) ) ;
#4538 = CARTESIAN_POINT ( 'NONE',  ( 91.82158438592158234, 17.20528682183301683, 0.000000000000000000 ) ) ;
#4539 = CARTESIAN_POINT ( 'NONE',  ( 199.9999999999999432, 14.14213562373113398, -14.14213562373094923 ) ) ;
#4540 = CARTESIAN_POINT ( 'NONE',  ( -86.96347745069643054, -18.24025645688353947, -40.00000000000002132 ) ) ;
#4541 = EDGE_CURVE ( 'NONE', #916, #15838, #25694, .T. ) ;
#4542 = CARTESIAN_POINT ( 'NONE',  ( -198.0356074513804288, -39.15871834505936278, 39.15871834505892224 ) ) ;
#4543 = CARTESIAN_POINT ( 'NONE',  ( 140.2235668266255857, -12.60094438999819744, -30.42137084504307509 ) ) ;
#4544 = CARTESIAN_POINT ( 'NONE',  ( -110.0960685945713777, 12.40690815813350412, -15.98210693810259286 ) ) ;
#4545 = CARTESIAN_POINT ( 'NONE',  ( 200.0000000000000000, 39.99999999999985079, 20.00000000000052225 ) ) ;
#4546 = CARTESIAN_POINT ( 'NONE',  ( 4.995406935893298872, -1.944352046434030652E-13, 55.24977328854835434 ) ) ;
#4547 = CARTESIAN_POINT ( 'NONE',  ( 151.7948205124836534, 4.785054706298574878, -51.78348778862537927 ) ) ;
#4548 = AXIS2_PLACEMENT_3D ( 'NONE', #15192, #10954, #9203 ) ;
#4549 = LINE ( 'NONE', #14377, #15153 ) ;
#4550 = CARTESIAN_POINT ( 'NONE',  ( -188.2995950289364941, -46.99046209955426434, -13.82811170417247126 ) ) ;
#4551 = CARTESIAN_POINT ( 'NONE',  ( 14.38125909742181818, -39.01709431150904095, -17.55144818341490165 ) ) ;
#4552 = ORIENTED_EDGE ( 'NONE', *, *, #1929, .T. ) ;
#4553 = CARTESIAN_POINT ( 'NONE',  ( -190.1935349183499113, 23.83022391594541745, -43.51927535257637913 ) ) ;
#4554 = CARTESIAN_POINT ( 'NONE',  ( 200.0000000000000000, 72.72568232011447265, -59.67546976104962653 ) ) ;
#4555 = CARTESIAN_POINT ( 'NONE',  ( 184.8905102610680444, 20.92133201514447194, -40.00000000000002132 ) ) ;
#4556 = EDGE_CURVE ( 'NONE', #6926, #11522, #21720, .T. ) ;
#4557 = DIRECTION ( 'NONE',  ( -0.01051738777841065495, 0.3656191333258888565, -0.9307051272558590771 ) ) ;
#4558 = CARTESIAN_POINT ( 'NONE',  ( -100.7734535825088358, -16.03295912088728770, 16.03295912088687913 ) ) ;
#4559 = ORIENTED_EDGE ( 'NONE', *, *, #25346, .T. ) ;
#4560 = VERTEX_POINT ( 'NONE', #17432 ) ;
#4561 = CARTESIAN_POINT ( 'NONE',  ( 200.0000000000000000, -11.82748140626729239, 14.88626897493814027 ) ) ;
#4562 = CARTESIAN_POINT ( 'NONE',  ( 121.8740240556053038, 11.10671848392283145, -26.81399039734612089 ) ) ;
#4563 = CARTESIAN_POINT ( 'NONE',  ( 23.38399212876430155, 23.33762193384666261, 42.85408588822703280 ) ) ;
#4564 = VERTEX_POINT ( 'NONE', #21957 ) ;
#4565 = EDGE_LOOP ( 'NONE', ( #8568, #7532 ) ) ;
#4566 = CARTESIAN_POINT ( 'NONE',  ( -198.0356074513804572, -17.40982414986482141, 39.15871834505909987 ) ) ;
#4567 = CARTESIAN_POINT ( 'NONE',  ( 199.0207495982873809, -19.04631292825652622, -6.112231798784620196 ) ) ;
#4568 = CARTESIAN_POINT ( 'NONE',  ( -110.0904723790771271, 3.161343376072184075, 19.95170499002183107 ) ) ;
#4569 = CARTESIAN_POINT ( 'NONE',  ( -56.48582580120559982, -6.472252184284282173, 50.09629031063965243 ) ) ;
#4570 = CARTESIAN_POINT ( 'NONE',  ( 4.995406935893289102, 10.78321810388998081, 10.78321810389001811 ) ) ;
#4571 = CARTESIAN_POINT ( 'NONE',  ( 190.0000000000000000, 4.765939974807309500E-14, 82.49999999999997158 ) ) ;
#4572 = CARTESIAN_POINT ( 'NONE',  ( -190.0000000000001705, 1.836970198721007106E-15, 0.000000000000000000 ) ) ;
#4573 = CARTESIAN_POINT ( 'NONE',  ( -135.8532207217289738, 40.00000000000031974, -30.84685318188603986 ) ) ;
#4574 = CARTESIAN_POINT ( 'NONE',  ( -56.48582580120559271, -1.062504017861011783E-13, 9.153146818113587102 ) ) ;
#4575 = CARTESIAN_POINT ( 'NONE',  ( -77.55640685876512919, -9.396736996787174904E-14, 22.13135000837103661 ) ) ;
#4576 = CARTESIAN_POINT ( 'NONE',  ( 190.0000000000000000, 52.50000000000007816, 52.49999999999999289 ) ) ;
#4577 = CARTESIAN_POINT ( 'NONE',  ( 199.0066333181452478, 19.18530965003537858, -5.635992787424102701 ) ) ;
#4578 = CARTESIAN_POINT ( 'NONE',  ( -183.1090696430332514, 13.45963186436838477, 45.18841929383249578 ) ) ;
#4579 = CARTESIAN_POINT ( 'NONE',  ( 14.38125909742181818, -39.01709431150928253, 17.55144818341435808 ) ) ;
#4580 = DIRECTION ( 'NONE',  ( 1.000000000000000000, 1.303213150798907793E-16, 2.465190328815661892E-32 ) ) ;
#4581 = CARTESIAN_POINT ( 'NONE',  ( 14.38125909742181996, -10.73282306403606157, 67.30136555895948902 ) ) ;
#4582 = DIRECTION ( 'NONE',  ( 0.000000000000000000, 0.000000000000000000, 1.000000000000000000 ) ) ;
#4583 = CARTESIAN_POINT ( 'NONE',  ( -30.26275506840325136, 27.08623969584614244, -29.48230279907770779 ) ) ;
#4584 = DIRECTION ( 'NONE',  ( 0.000000000000000000, 1.000000000000000000, 0.000000000000000000 ) ) ;
#4585 = CARTESIAN_POINT ( 'NONE',  ( 136.1360204305621266, 35.03383547441298163, 40.00000000000002132 ) ) ;
#4586 = CARTESIAN_POINT ( 'NONE',  ( -105.3755690713226585, 12.89780903124349720, 43.67073346367994446 ) ) ;
#4587 = CARTESIAN_POINT ( 'NONE',  ( -238.4067589809705794, -0.9644942799826262680, 0.000000000000000000 ) ) ;
#4588 = CARTESIAN_POINT ( 'NONE',  ( -615.3980966596806184, 30.54813962807670435, -33.04656978373367338 ) ) ;
#4589 = ORIENTED_EDGE ( 'NONE', *, *, #12576, .F. ) ;
#4590 = CARTESIAN_POINT ( 'NONE',  ( 151.7948205124836534, -39.99999999999992184, -6.767089262349454515 ) ) ;
#4591 = CARTESIAN_POINT ( 'NONE',  ( 199.0067109444755147, 5.297717337603594423, -19.32538706503994064 ) ) ;
#4592 = DIRECTION ( 'NONE',  ( 0.000000000000000000, 0.000000000000000000, 1.000000000000000000 ) ) ;
#4593 = EDGE_LOOP ( 'NONE', ( #5480, #4756, #26123, #10064, #24035 ) ) ;
#4594 = ORIENTED_EDGE ( 'NONE', *, *, #19220, .T. ) ;
#4595 = CARTESIAN_POINT ( 'NONE',  ( 91.82158438592158234, 22.79471317813471742, 40.00000000000002132 ) ) ;
#4596 = PRESENTATION_STYLE_ASSIGNMENT (( #2457 ) ) ;
#4597 = EDGE_CURVE ( 'NONE', #18341, #10496, #17055, .T. ) ;
#4598 = CARTESIAN_POINT ( 'NONE',  ( 136.1360204305621266, 3.511608612530757068, -3.511608612530642937 ) ) ;
#4599 = CARTESIAN_POINT ( 'NONE',  ( -105.2053629887268187, -21.49364769383058160, 0.6703845944188828732 ) ) ;
#4600 = ADVANCED_FACE ( 'NONE', ( #1607 ), #11564, .T. ) ;
#4601 = CARTESIAN_POINT ( 'NONE',  ( -77.55640685876511498, -22.13135000837103661, -4.964495286674871776E-15 ) ) ;
#4602 = DIRECTION ( 'NONE',  ( 1.000000000000000000, 1.836970198721030181E-16, 0.000000000000000000 ) ) ;
#4603 = CARTESIAN_POINT ( 'NONE',  ( 200.0000000000000853, 11.56430744387933274, -15.08818561847743922 ) ) ;
#4604 = ADVANCED_FACE ( 'NONE', ( #15815 ), #15950, .F. ) ;
#4605 = CARTESIAN_POINT ( 'NONE',  ( -190.0000000000000000, -52.49999999999972289, -82.49999999999998579 ) ) ;
#4606 = CARTESIAN_POINT ( 'NONE',  ( 91.82158438592158234, -12.16597498399995203, -44.40256751092347542 ) ) ;
#4607 = CARTESIAN_POINT ( 'NONE',  ( -208.1127848780265026, -10.60833733269537227, -10.60833733269551793 ) ) ;
#4608 = FACE_OUTER_BOUND ( 'NONE', #5489, .T. ) ;
#4609 = CARTESIAN_POINT ( 'NONE',  ( 184.8905102610680444, 39.99999999999983658, 20.92133201514485563 ) ) ;
#4610 = CARTESIAN_POINT ( 'NONE',  ( 146.6084372240433993, 24.48358557860307272, 24.48358557860347418 ) ) ;
#4611 = CARTESIAN_POINT ( 'NONE',  ( 180.0000000000000284, -135.7889608577475542, -82.49999999999998579 ) ) ;
#4612 = CARTESIAN_POINT ( 'NONE',  ( 192.4448373802100889, -14.14213562375876698, -14.14213562375885047 ) ) ;
#4613 = CARTESIAN_POINT ( 'NONE',  ( 14.38125909742183062, -67.30136555898262429, 10.73282306405838682 ) ) ;
#4614 = CARTESIAN_POINT ( 'NONE',  ( 199.0061394614210144, 18.47445098178025447, -7.648446613688572704 ) ) ;
#4616 = CARTESIAN_POINT ( 'NONE',  ( -192.9588430854690273, 39.99999999999980105, 54.46834944098235809 ) ) ;
#4615 = CARTESIAN_POINT ( 'NONE',  ( 151.7948205124836534, -51.78348778862529400, -4.785054706299085581 ) ) ;
#4617 = CARTESIAN_POINT ( 'NONE',  ( 22.80622392652934494, 43.16567765897924147, -17.87980911537434636 ) ) ;
#4618 = CARTESIAN_POINT ( 'NONE',  ( 199.9999999999999432, -20.00000000000006750, 0.000000000000000000 ) ) ;
#4619 = CARTESIAN_POINT ( 'NONE',  ( -100.7734535825088500, -16.03295912088716335, 40.53558337403673306 ) ) ;
#4620 = CARTESIAN_POINT ( 'NONE',  ( -198.0356074513804572, 55.37879056871320671, 40.00000000000002132 ) ) ;
#4621 = CARTESIAN_POINT ( 'NONE',  ( -40.07203023069898506, -34.25109662817532552, 11.15662918590587260 ) ) ;
#4622 = CARTESIAN_POINT ( 'NONE',  ( 130.8568914410475088, -34.05028731879786363, 40.00000000000002132 ) ) ;
#4623 = ORIENTED_EDGE ( 'NONE', *, *, #14927, .F. ) ;
#4624 = CARTESIAN_POINT ( 'NONE',  ( 85.88462004915263037, -10.32535765023374807, -22.72792989731669167 ) ) ;
#4625 = CARTESIAN_POINT ( 'NONE',  ( -198.0356074513804572, -17.40982414986482141, 39.15871834505909987 ) ) ;
#4626 = CARTESIAN_POINT ( 'NONE',  ( -8.255580677127136724, -22.62611236876437815, 41.75907689859029404 ) ) ;
#4627 = CARTESIAN_POINT ( 'NONE',  ( 8.556015491740193823, 14.17785852676870917, -49.31947911770388515 ) ) ;
#4628 = CARTESIAN_POINT ( 'NONE',  ( 199.0236444319429268, -19.98745889671670284, 0.8241971460415670192 ) ) ;
#4629 = CARTESIAN_POINT ( 'NONE',  ( 184.8905102610680444, -14.79361573936399665, 14.79361573936367158 ) ) ;
#4630 = EDGE_CURVE ( 'NONE', #25529, #20449, #14665, .T. ) ;
#4631 = DIRECTION ( 'NONE',  ( 2.985653255390529422E-32, -4.182618615277681568E-16, 1.000000000000000000 ) ) ;
#4632 = DIRECTION ( 'NONE',  ( 1.000000000000000000, 1.836970198721030181E-16, 0.000000000000000000 ) ) ;
#4634 = AXIS2_PLACEMENT_3D ( 'NONE', #19307, #15685, #23560 ) ;
#4633 = CARTESIAN_POINT ( 'NONE',  ( -188.2957210513883979, -13.82790368522451452, 46.98905903629621150 ) ) ;
#4635 = CARTESIAN_POINT ( 'NONE',  ( -135.8532207217289738, 6.472252184284096543, 6.472252184284234211 ) ) ;
#4636 = CARTESIAN_POINT ( 'NONE',  ( -259.2033419157646676, -6.730120644403663199, 6.730120644403451813 ) ) ;
#4637 = CARTESIAN_POINT ( 'NONE',  ( -86.96347745069644475, 15.38646221621772092, 15.38646221621800336 ) ) ;
#4639 = CARTESIAN_POINT ( 'NONE',  ( 199.9999999999999432, 14.14213562373110911, -14.14213562373072364 ) ) ;
#4638 = CARTESIAN_POINT ( 'NONE',  ( -86.96347745069644475, 15.38646221621772092, 15.38646221621800336 ) ) ;
#4640 = CARTESIAN_POINT ( 'NONE',  ( -135.8532207217289738, -6.472252184284280396, 6.472252184284099208 ) ) ;
#4641 = CARTESIAN_POINT ( 'NONE',  ( 151.7948205124836250, -6.767089262349004208, -2.449293598294708485E-15 ) ) ;
#4642 = CARTESIAN_POINT ( 'NONE',  ( -91.56559293963834989, -22.67402823373193499, -40.00000000000002132 ) ) ;
#4643 = CARTESIAN_POINT ( 'NONE',  ( -192.9588430854689989, 1.161019517985663313E-13, -14.46834944099969533 ) ) ;
#4644 = CARTESIAN_POINT ( 'NONE',  ( -56.48582580120559982, 21.81201906317778594, -34.75652343174606074 ) ) ;
#4645 = CARTESIAN_POINT ( 'NONE',  ( -89.91498783732122035, 20.17141720496151436, -8.733585467785427880 ) ) ;
#4646 = CARTESIAN_POINT ( 'NONE',  ( 170.2234770963711128, -10.92277846919187034, -10.92277846919209594 ) ) ;
#4647 = CARTESIAN_POINT ( 'NONE',  ( 190.0000000000000284, -82.49999999999990052, 52.49999999999977973 ) ) ;
#4648 = ORIENTED_EDGE ( 'NONE', *, *, #7991, .F. ) ;
#4649 = CARTESIAN_POINT ( 'NONE',  ( 146.6084372240433709, -24.48358557860329299, 32.08495691632052882 ) ) ;
#4650 = CARTESIAN_POINT ( 'NONE',  ( -89.91498783732303934, 8.087768383598069377, 20.43892340003915820 ) ) ;
#4651 = CARTESIAN_POINT ( 'NONE',  ( -86.96347745069644475, -12.89780903124413491, 12.89780903124398037 ) ) ;
#4652 = CARTESIAN_POINT ( 'NONE',  ( 8.556015491675912799, -44.89939803569713916, -24.84887822172902361 ) ) ;
#4653 = ORIENTED_EDGE ( 'NONE', *, *, #2327, .F. ) ;
#4654 = CARTESIAN_POINT ( 'NONE',  ( -105.2054292635175443, 15.69192375045724930, 14.70407267694731956 ) ) ;
#4655 = CARTESIAN_POINT ( 'NONE',  ( -82.28158521660047597, -9.172166285104129457, -18.01696758243814855 ) ) ;
#4656 = CARTESIAN_POINT ( 'NONE',  ( 199.9999999999997442, 8.817246258963736594, -16.83121203733840332 ) ) ;
#4657 = CARTESIAN_POINT ( 'NONE',  ( 200.0000000000000000, 66.50000000000009948, -66.50000000000005684 ) ) ;
#4658 = AXIS2_PLACEMENT_3D ( 'NONE', #13819, #1218, #15681 ) ;
#4659 = CARTESIAN_POINT ( 'NONE',  ( -208.1127848780265026, 55.00245453012668406, 2.449293598294708485E-15 ) ) ;
#4660 = CARTESIAN_POINT ( 'NONE',  ( -135.8532207217289738, -6.472252184284280396, 6.472252184284099208 ) ) ;
#4661 = CARTESIAN_POINT ( 'NONE',  ( 199.0130717410369812, 17.47129959974107294, 9.736724163761770967 ) ) ;
#4662 = B_SPLINE_CURVE_WITH_KNOTS ( 'NONE', 3,
 ( #1352, #3468, #21564, #21692, #25695, #25573 ),
 .UNSPECIFIED., .F., .F.,
 ( 4, 2, 4 ),
 ( 0.000000000000000000, 0.03937794852163882531, 0.07875589704327765062 ),
 .UNSPECIFIED. ) ;
#4663 = CARTESIAN_POINT ( 'NONE',  ( 19.06497207195981858, -38.31983398719641087, 18.24870850772724040 ) ) ;
#4664 = CARTESIAN_POINT ( 'NONE',  ( 130.8568914410475372, 8.154165912415230659E-16, 5.949712681206690945 ) ) ;
#4665 = CARTESIAN_POINT ( 'NONE',  ( 151.7948205124836534, 40.00000000000017053, -33.23291073765538783 ) ) ;
#4666 = DIRECTION ( 'NONE',  ( 1.000000000000000000, 0.000000000000000000, -0.000000000000000000 ) ) ;
#4667 = CARTESIAN_POINT ( 'NONE',  ( 192.4448373802101173, -19.99999999996056843, -40.00000000000002132 ) ) ;
#4669 = CARTESIAN_POINT ( 'NONE',  ( -105.3755690713226727, 15.38646221621793231, -15.38646221621779020 ) ) ;
#4668 = CARTESIAN_POINT ( 'NONE',  ( 21.80824205441264141, -13.88338701302259715, -47.36272483143062573 ) ) ;
#4670 = CARTESIAN_POINT ( 'NONE',  ( -208.1127848780264742, -55.00245453012676222, -2.449293598294708485E-15 ) ) ;
#4671 = CARTESIAN_POINT ( 'NONE',  ( 163.1118516004056573, -9.006482792069636645, 9.006482792069567367 ) ) ;
#4672 = CARTESIAN_POINT ( 'NONE',  ( 141.7948666911894975, -12.58737617328892888, -30.38861427224631839 ) ) ;
#4673 = CARTESIAN_POINT ( 'NONE',  ( -114.6097568999588390, 10.88341597703020547, -19.09891331897681255 ) ) ;
#4674 = CARTESIAN_POINT ( 'NONE',  ( 151.7948205124836534, 39.99999999999970157, 33.23291073765595627 ) ) ;
#4675 = CARTESIAN_POINT ( 'NONE',  ( -135.8532207217289738, 39.99999999999989342, 30.84685318188660474 ) ) ;
#4676 = CARTESIAN_POINT ( 'NONE',  ( 199.0262541782678340, -11.79586192385960430, 16.15815307234555576 ) ) ;
#4677 = CARTESIAN_POINT ( 'NONE',  ( -716.9846540392142060, -52.49999999999972999, -82.49999999999998579 ) ) ;
#4678 = CARTESIAN_POINT ( 'NONE',  ( 19.06497207195981858, -38.31983398719616218, -18.24870850772777331 ) ) ;
#4679 = EDGE_LOOP ( 'NONE', ( #25946, #11681, #735, #14353 ) ) ;
#4681 = CARTESIAN_POINT ( 'NONE',  ( 98.29820294267312875, 7.653668647304333383, -18.47759065023115355 ) ) ;
#4680 = CARTESIAN_POINT ( 'NONE',  ( 170.2234770963711128, 17.36149277826980253, 17.36149277827007253 ) ) ;
#4682 = CARTESIAN_POINT ( 'NONE',  ( 125.5832160019861305, 28.05309928654008900, -11.61997419108379859 ) ) ;
#4683 = CARTESIAN_POINT ( 'NONE',  ( 192.4448373802101173, 20.00000000003945644, -40.00000000000002132 ) ) ;
#4684 = CIRCLE ( 'NONE', #3390, 5.000000000000004441 ) ;
#4685 = CARTESIAN_POINT ( 'NONE',  ( -105.2054292635176580, 14.23233549213511573, 16.16366093526940517 ) ) ;
#4686 = CARTESIAN_POINT ( 'NONE',  ( 200.0000000000000000, -42.42640687119272513, -14.14213562373140753 ) ) ;
#4687 = ORIENTED_EDGE ( 'NONE', *, *, #15718, .F. ) ;
#4688 = VERTEX_POINT ( 'NONE', #9710 ) ;
#4689 = CARTESIAN_POINT ( 'NONE',  ( -105.4741150117369273, 8.366608964608960974, -19.60045294982168329 ) ) ;
#4690 = CARTESIAN_POINT ( 'NONE',  ( -102.4294859495706049, 8.407280617849425042, -20.29697089045613012 ) ) ;
#4691 = ADVANCED_FACE ( 'NONE', ( #17815 ), #23941, .T. ) ;
#4692 = CARTESIAN_POINT ( 'NONE',  ( 22.78333232258906094, 17.88247728649375645, 43.17211919388270758 ) ) ;
#4693 = ORIENTED_EDGE ( 'NONE', *, *, #19719, .F. ) ;
#4694 = ORIENTED_EDGE ( 'NONE', *, *, #1482, .T. ) ;
#4695 = CARTESIAN_POINT ( 'NONE',  ( 14.38125909742181285, -17.55144818341476309, 39.01709431150910490 ) ) ;
#4696 = CARTESIAN_POINT ( 'NONE',  ( 199.0173355507466226, -15.87315179554041045, -12.16952887920782445 ) ) ;
#4697 = CARTESIAN_POINT ( 'NONE',  ( -114.6659165473969040, -4.804252803496178892, 21.50057250525394181 ) ) ;
#4698 = CARTESIAN_POINT ( 'NONE',  ( 146.6084372240433709, -24.48358557860329299, 32.08495691632052882 ) ) ;
#4699 = CARTESIAN_POINT ( 'NONE',  ( 184.8905102610680444, -14.79361573936379415, -14.79361573936387941 ) ) ;
#4700 = CARTESIAN_POINT ( 'NONE',  ( 151.7948205124836534, 40.00000000000002842, 6.767089262349174739 ) ) ;
#4701 = CARTESIAN_POINT ( 'NONE',  ( -199.9999999999999716, -18.14835560307974660, 46.41341197396111795 ) ) ;
#4702 = EDGE_CURVE ( 'NONE', #23932, #17972, #15684, .T. ) ;
#4703 = CARTESIAN_POINT ( 'NONE',  ( -88.37877758191619648, -8.575405934157467769, -19.92653024494341807 ) ) ;
#4704 = COLOUR_RGB ( '',0.7921568627450980005, 0.8196078431372548767, 0.9333333333333333481 ) ;
#4705 = ADVANCED_FACE ( 'NONE', ( #17949 ), #22095, .F. ) ;
#4706 = CARTESIAN_POINT ( 'NONE',  ( -86.96347745069644475, 1.775309070576523494E-13, -18.24025645688352881 ) ) ;
#4707 = CARTESIAN_POINT ( 'NONE',  ( -86.96347745069644475, -2.438961472018186339E-13, 21.75974354311649961 ) ) ;
#4708 = CARTESIAN_POINT ( 'NONE',  ( -652.7959024289831405, 36.96089747262086433, 15.32130098737787627 ) ) ;
#4709 = CARTESIAN_POINT ( 'NONE',  ( -87.13361725327072804, -21.49321519333431141, -3.542586001259484843E-15 ) ) ;
#4710 = CARTESIAN_POINT ( 'NONE',  ( 199.0116003924211725, 18.71458825927322422, 7.055789865482638312 ) ) ;
#4711 = CARTESIAN_POINT ( 'NONE',  ( -188.9524464571000522, 23.58788642769107469, 43.19209889639545707 ) ) ;
#4712 = CARTESIAN_POINT ( 'NONE',  ( 184.8905102610680444, -41.77492675556007384, 14.79361573936348684 ) ) ;
#4713 = CARTESIAN_POINT ( 'NONE',  ( -94.58366989427474891, 9.000605044545403999, 20.58370269626844618 ) ) ;
#4714 = CARTESIAN_POINT ( 'NONE',  ( -198.0356074513804572, -10.87444709760996986, 67.44298959253333692 ) ) ;
#4715 = CARTESIAN_POINT ( 'NONE',  ( -575.0231298121445889, 75.00000000000000000, 34.99999999999821654 ) ) ;
#4716 = CARTESIAN_POINT ( 'NONE',  ( 200.0000000000000000, 42.42640687119310172, -14.14213562373052646 ) ) ;
#4717 = CARTESIAN_POINT ( 'NONE',  ( -659.9578749576080554, 43.44209025057394058, 11.75201215860449366 ) ) ;
#4718 = DIRECTION ( 'NONE',  ( -7.401486830834374307E-15, 0.9307566067077635008, -0.3656393565657962141 ) ) ;
#4719 = CARTESIAN_POINT ( 'NONE',  ( -208.1127848780264742, 38.89260858015707356, 17.67593391476696141 ) ) ;
#4720 = CARTESIAN_POINT ( 'NONE',  ( -280.0000000000000000, 19.99999999999996092, -0.000000000000000000 ) ) ;
#4721 = DIRECTION ( 'NONE',  ( 0.9698969544411717436, -0.09318942518908124306, 0.2249791741443379622 ) ) ;
#4722 = ORIENTED_EDGE ( 'NONE', *, *, #11245, .F. ) ;
#4723 = CARTESIAN_POINT ( 'NONE',  ( 163.1118516004056573, -39.99999999999986500, -12.73709011382517353 ) ) ;
#4724 = CARTESIAN_POINT ( 'NONE',  ( -626.9846540392142060, 95.00000000000000000, 0.000000000000000000 ) ) ;
#4725 = CARTESIAN_POINT ( 'NONE',  ( 160.9163046357249129, -125.7889608577475400, 55.61140153332248559 ) ) ;
#4726 = VERTEX_POINT ( 'NONE', #5855 ) ;
#4727 = VERTEX_POINT ( 'NONE', #13442 ) ;
#4728 = CARTESIAN_POINT ( 'NONE',  ( 91.82158438592158234, 22.79471317813472098, 2.449293598294708485E-15 ) ) ;
#4729 = CARTESIAN_POINT ( 'NONE',  ( -102.4309680866828671, -20.43798635329655866, -8.087567261865729051 ) ) ;
#4730 = CARTESIAN_POINT ( 'NONE',  ( -114.6097568999414733, -21.20070836099096923, -5.809233881233475394 ) ) ;
#4731 = DIRECTION ( 'NONE',  ( 0.000000000000000000, -1.000000000000000000, 0.000000000000000000 ) ) ;
#4732 = CARTESIAN_POINT ( 'NONE',  ( 91.82158438592159655, -39.99999999999994316, -17.20528682183314118 ) ) ;
#4733 = CARTESIAN_POINT ( 'NONE',  ( 200.0000000000002842, 11.06692676694369304, -15.45668394874709506 ) ) ;
#4734 = CARTESIAN_POINT ( 'NONE',  ( 199.9999999999999716, -3.099454106775636930, -18.75032367107563758 ) ) ;
#4735 = VECTOR ( 'NONE', #4757, 1000.000000000000000 ) ;
#4736 = CIRCLE ( 'NONE', #5992, 15.00000000000000533 ) ;
#4737 = CARTESIAN_POINT ( 'NONE',  ( 130.8568914410475088, -24.07718906446864793, -32.49135343045505664 ) ) ;
#4738 = CARTESIAN_POINT ( 'NONE',  ( -162.0762913951020892, -1.198031840385767266, -1.198031840385758384 ) ) ;
#4739 = AXIS2_PLACEMENT_3D ( 'NONE', #23683, #7444, #10979 ) ;
#4740 = SPHERICAL_SURFACE ( 'NONE', #23344, 15.00000000000000000 ) ;
#4741 = CARTESIAN_POINT ( 'NONE',  ( 136.1360204305621266, -3.419521671106983309E-13, 35.03383547441296741 ) ) ;
#4742 = CARTESIAN_POINT ( 'NONE',  ( 192.4448373802100889, 14.14213562375873678, 14.14213562375894817 ) ) ;
#4743 = CARTESIAN_POINT ( 'NONE',  ( 21.99343714674520811, 13.87412077874984462, 47.30053030063388064 ) ) ;
#4744 = CARTESIAN_POINT ( 'NONE',  ( 184.8905102610680444, -14.79361573936389540, 41.77492675555996016 ) ) ;
#4745 = CARTESIAN_POINT ( 'NONE',  ( 151.7948205124836250, -4.785054706301671068, 4.785054706301645311 ) ) ;
#4746 = CARTESIAN_POINT ( 'NONE',  ( 199.0089039147429446, 19.99546107379537929, 1.174471671411769780 ) ) ;
#4748 = CARTESIAN_POINT ( 'NONE',  ( 0.2972598230769883387, 39.99999999999997158, 14.33493731733947563 ) ) ;
#4747 = CARTESIAN_POINT ( 'NONE',  ( 130.8568914410475088, -24.07718906446864793, -32.49135343045505664 ) ) ;
#4749 = DIRECTION ( 'NONE',  ( 0.000000000000000000, 1.000000000000000000, 0.000000000000000000 ) ) ;
#4750 = CARTESIAN_POINT ( 'NONE',  ( -86.96347745069644475, -43.67073346367983788, 12.89780903124397149 ) ) ;
#4751 = CARTESIAN_POINT ( 'NONE',  ( 163.1118516004056573, -27.26290988616869626, 40.00000000000002132 ) ) ;
#4752 = VERTEX_POINT ( 'NONE', #3337 ) ;
#4753 = CARTESIAN_POINT ( 'NONE',  ( 8.209392600955618846, -49.31072049266142443, 14.17653494425346672 ) ) ;
#4754 = CIRCLE ( 'NONE', #11964, 14.99999999999999822 ) ;
#4755 = CARTESIAN_POINT ( 'NONE',  ( -135.8532207217289738, 30.84685318188643421, 40.00000000000002132 ) ) ;
#4756 = ORIENTED_EDGE ( 'NONE', *, *, #8977, .T. ) ;
#4757 = DIRECTION ( 'NONE',  ( 1.000000000000000000, -0.000000000000000000, -0.000000000000000000 ) ) ;
#4758 = AXIS2_PLACEMENT_3D ( 'NONE', #21726, #24121, #17720 ) ;
#4759 = CARTESIAN_POINT ( 'NONE',  ( -91.56559293963834989, -16.03295912088706388, -16.03295912088710651 ) ) ;
#4760 = CARTESIAN_POINT ( 'NONE',  ( -6.754359963543765666, -17.56548336386596532, 42.40682816667121102 ) ) ;
#4761 = DIRECTION ( 'NONE',  ( -1.000000000000000000, 0.000000000000000000, 0.000000000000000000 ) ) ;
#4762 = CARTESIAN_POINT ( 'NONE',  ( 4.155455573169746231, 18.49472242011614398, -44.65020969900606218 ) ) ;
#4763 = CARTESIAN_POINT ( 'NONE',  ( 199.0232268534825835, -20.00153578626446915, -0.3291254421221458948 ) ) ;
#4764 = CARTESIAN_POINT ( 'NONE',  ( 151.7948205124836534, 4.785054706297857230, 51.78348778862544322 ) ) ;
#4765 = CARTESIAN_POINT ( 'NONE',  ( -86.95450734974414786, -20.33657406931063605, 6.704150134019479346 ) ) ;
#4766 = DIRECTION ( 'NONE',  ( 0.000000000000000000, 0.000000000000000000, 1.000000000000000000 ) ) ;
#4767 = CARTESIAN_POINT ( 'NONE',  ( -191.2490444017190327, -18.16428715637485780, 43.85246840377622846 ) ) ;
#4768 = CARTESIAN_POINT ( 'NONE',  ( -213.1075012329537230, 18.58567234101174037, -37.98287015391222354 ) ) ;
#4769 = CARTESIAN_POINT ( 'NONE',  ( 14.38125909742180752, 17.55144818341448953, 39.01709431150923280 ) ) ;
#4770 = CARTESIAN_POINT ( 'NONE',  ( -56.48582580120559982, -6.472252184283581400, -50.09629031063973059 ) ) ;
#4771 = CARTESIAN_POINT ( 'NONE',  ( -238.4067589809705794, -0.6820004457913585449, -0.6820004457913265705 ) ) ;
#4772 = AXIS2_PLACEMENT_3D ( 'NONE', #23209, #462, #4592 ) ;
#4774 = CARTESIAN_POINT ( 'NONE',  ( -198.0356074513804572, 39.15871834505956173, -39.15871834505865223 ) ) ;
#4773 = CARTESIAN_POINT ( 'NONE',  ( -280.0000000000000000, 14.14213562373078581, 14.14213562373108424 ) ) ;
#4775 = CARTESIAN_POINT ( 'NONE',  ( -192.9588430854690273, 66.79921049724377724, -10.23066800231904239 ) ) ;
#4776 = CARTESIAN_POINT ( 'NONE',  ( 184.8905102610680444, 20.92133201514447194, 40.00000000000002132 ) ) ;
#4777 = CARTESIAN_POINT ( 'NONE',  ( 151.7948205124836534, -33.23291073765550863, -40.00000000000002132 ) ) ;
#4778 = CARTESIAN_POINT ( 'NONE',  ( 184.8905102610680444, 41.77492675556005253, -14.79361573936377461 ) ) ;
#4779 = EDGE_CURVE ( 'NONE', #2862, #21778, #11497, .T. ) ;
#4780 = CARTESIAN_POINT ( 'NONE',  ( -200.0000000000000000, 0.000000000000000000, 0.000000000000000000 ) ) ;
#4781 = CARTESIAN_POINT ( 'NONE',  ( 200.0000000000000000, -42.42640687119290988, 14.14213562373064903 ) ) ;
#4782 = EDGE_CURVE ( 'NONE', #4460, #8935, #23839, .T. ) ;
#4783 = CARTESIAN_POINT ( 'NONE',  ( -121.8281105901294978, 23.07023229646648943, -8.694016235322095554 ) ) ;
#4784 = ORIENTED_EDGE ( 'NONE', *, *, #26065, .T. ) ;
#4785 = CARTESIAN_POINT ( 'NONE',  ( -30.26275506840324070, 1.198031551615912571, 57.76657404653985139 ) ) ;
#4786 = CARTESIAN_POINT ( 'NONE',  ( -102.4068193528165835, -20.44188272012828023, -8.088405365068805253 ) ) ;
#4787 = CARTESIAN_POINT ( 'NONE',  ( -280.0000000000000568, 14.14213562373067745, 42.42640687119295251 ) ) ;
#4788 = CARTESIAN_POINT ( 'NONE',  ( 9.345847406389310663, -44.90706793518258877, -24.85453859512280417 ) ) ;
#4789 = EDGE_CURVE ( 'NONE', #22711, #9566, #13628, .T. ) ;
#4790 = EDGE_CURVE ( 'NONE', #1425, #19072, #15746, .T. ) ;
#4791 = VERTEX_POINT ( 'NONE', #5718 ) ;
#4792 = CARTESIAN_POINT ( 'NONE',  ( -30.26275506840324070, 1.694272468446254232, 0.000000000000000000 ) ) ;
#4793 = CARTESIAN_POINT ( 'NONE',  ( -114.7826396786174001, -14.66973228884550373, -16.62872306281069257 ) ) ;
#4794 = CARTESIAN_POINT ( 'NONE',  ( 200.0000000000002274, 18.09557305485218848, -5.802546270622393365 ) ) ;
#4795 = AXIS2_PLACEMENT_3D ( 'NONE', #22185, #22049, #4093 ) ;
#4796 = FACE_OUTER_BOUND ( 'NONE', #26350, .T. ) ;
#4797 = CARTESIAN_POINT ( 'NONE',  ( -213.1075012329537230, 53.71589010950162191, -40.00000000000002132 ) ) ;
#4798 = CARTESIAN_POINT ( 'NONE',  ( -108.4672927838138605, 19.20738496773866544, 7.955959351357155818 ) ) ;
#4799 = CARTESIAN_POINT ( 'NONE',  ( 199.0163148259956358, 13.65645126726637670, 14.61284818176725331 ) ) ;
#4800 = CARTESIAN_POINT ( 'NONE',  ( -208.1127848780264742, -67.17687982760682530, -10.60833733268364298 ) ) ;
#4801 = CARTESIAN_POINT ( 'NONE',  ( -86.96347745069644475, -8.210974027862429531E-14, 18.24025645688352881 ) ) ;
#4802 = CARTESIAN_POINT ( 'NONE',  ( 136.1360204305621551, 40.00000000000002842, 4.966164525587208445 ) ) ;
#4803 = DIRECTION ( 'NONE',  ( 0.000000000000000000, 0.000000000000000000, 1.000000000000000000 ) ) ;
#4804 = CARTESIAN_POINT ( 'NONE',  ( 192.4448373802101173, 20.00000000003945644, -40.00000000000002132 ) ) ;
#4806 = CARTESIAN_POINT ( 'NONE',  ( -626.9846540392140923, 26.45751311064577749, 30.00000000000005329 ) ) ;
#4805 = CARTESIAN_POINT ( 'NONE',  ( 22.13784119383913662, -17.95298715833818193, -43.34234508276890807 ) ) ;
#4807 = CARTESIAN_POINT ( 'NONE',  ( 192.4448373802100889, -19.99999999996057198, -2.449293598294708485E-15 ) ) ;
#4808 = CARTESIAN_POINT ( 'NONE',  ( 19.06497207195981147, -10.03556273973439517, 10.03556273973429214 ) ) ;
#4809 = CARTESIAN_POINT ( 'NONE',  ( -100.7734535825088358, -2.560096224687585342E-13, 22.67402823373191723 ) ) ;
#4810 = CARTESIAN_POINT ( 'NONE',  ( -105.3846709044788810, 19.12138504417525198, -9.637707283830140526 ) ) ;
#4811 = CARTESIAN_POINT ( 'NONE',  ( -198.0356074513804572, 5.461327841961909642E-13, -55.37879056873073580 ) ) ;
#4812 = CARTESIAN_POINT ( 'NONE',  ( 151.7948205124836250, -23.49921654116339553, -23.49921654116350211 ) ) ;
#4813 = FACE_BOUND ( 'NONE', #7599, .T. ) ;
#4814 = DIRECTION ( 'NONE',  ( 0.000000000000000000, 1.000000000000000000, 0.000000000000000000 ) ) ;
#4815 = CARTESIAN_POINT ( 'NONE',  ( 0.2972598230770153171, -66.70487387989861361, 10.13633138497438324 ) ) ;
#4816 = ORIENTED_EDGE ( 'NONE', *, *, #5570, .F. ) ;
#4818 = CARTESIAN_POINT ( 'NONE',  ( -16.78454218927527108, 39.63790004360789965, -16.41855578212769728 ) ) ;
#4817 = CARTESIAN_POINT ( 'NONE',  ( -77.78673448795173329, 6.807559357124845612, -20.89197888679335691 ) ) ;
#4819 = DIRECTION ( 'NONE',  ( 0.9352143323239582307, 0.1355013636775663222, -0.3271292299036774320 ) ) ;
#4820 = CARTESIAN_POINT ( 'NONE',  ( 0.2972598230770129857, -54.33493731733936016, -40.00000000000002132 ) ) ;
#4821 = CARTESIAN_POINT ( 'NONE',  ( -114.6382724355127607, 18.98542650371850016, -11.21026131167359807 ) ) ;
#4822 = CARTESIAN_POINT ( 'NONE',  ( -86.96347745069644475, -15.38646221621807442, 15.38646221621768184 ) ) ;
#4823 = ORIENTED_EDGE ( 'NONE', *, *, #8977, .F. ) ;
#4824 = VERTEX_POINT ( 'NONE', #13823 ) ;
#4825 = CARTESIAN_POINT ( 'NONE',  ( 23.37394308801976450, 46.80823611210215063, -13.80096434448263309 ) ) ;
#4826 = ORIENTED_EDGE ( 'NONE', *, *, #15003, .F. ) ;
#4827 = EDGE_LOOP ( 'NONE', ( #14187, #10973 ) ) ;
#4828 = CARTESIAN_POINT ( 'NONE',  ( -259.2033419157646676, -35.01439189186554302, 21.55415060305832498 ) ) ;
#4829 = CARTESIAN_POINT ( 'NONE',  ( 199.0156165598358768, -13.68207045034666969, -14.60203791353019476 ) ) ;
#4830 = CARTESIAN_POINT ( 'NONE',  ( -105.3841230195786096, -19.11845054111881481, -9.645493323979394518 ) ) ;
#4831 = CARTESIAN_POINT ( 'NONE',  ( -162.0762913951021176, -27.08623940707624911, 29.48230308784761888 ) ) ;
#4832 = CARTESIAN_POINT ( 'NONE',  ( 151.7948205124836250, -23.49921654116339553, -23.49921654116350211 ) ) ;
#4833 = CARTESIAN_POINT ( 'NONE',  ( -135.8532207217289738, 39.99999999999989342, 30.84685318188660474 ) ) ;
#4834 = LINE ( 'NONE', #4965, #14695 ) ;
#4835 = CARTESIAN_POINT ( 'NONE',  ( -199.9999999999999432, 14.17215463606929227, 49.28189405767592746 ) ) ;
#4836 = CARTESIAN_POINT ( 'NONE',  ( 136.1360204305621551, -40.00000000000036238, 35.03383547441254109 ) ) ;
#4837 = CARTESIAN_POINT ( 'NONE',  ( 184.8905102610680444, -1.851754852062639767E-13, 20.92133201514444352 ) ) ;
#4838 = CARTESIAN_POINT ( 'NONE',  ( -82.23726319249648498, 14.28014421912408061, 14.28014421912424226 ) ) ;
#4839 = CARTESIAN_POINT ( 'NONE',  ( 200.0000000000000000, 69.29737539576909455, -75.30386416458597409 ) ) ;
#4840 = CARTESIAN_POINT ( 'NONE',  ( 199.0120006491917479, 18.40818734026414560, 7.815811290271758693 ) ) ;
#4841 = CARTESIAN_POINT ( 'NONE',  ( -188.2956751479549098, 23.44846780264100872, 43.00407324591984093 ) ) ;
#4842 = CARTESIAN_POINT ( 'NONE',  ( 19.06497207195981147, -10.03556273973425483, -10.03556273973443247 ) ) ;
#4843 = DIRECTION ( 'NONE',  ( 1.000000000000000000, -0.000000000000000000, -0.000000000000000000 ) ) ;
#4844 = CARTESIAN_POINT ( 'NONE',  ( -100.7734535825088500, 44.31723036834890905, 12.25131212657507795 ) ) ;
#4845 = CARTESIAN_POINT ( 'NONE',  ( -87.01506749147795006, -18.46228859040754955, 10.84947533659219943 ) ) ;
#4846 = CARTESIAN_POINT ( 'NONE',  ( 57.59792236341147031, 30.00663442387720181, -26.56190807104661289 ) ) ;
#4847 = CARTESIAN_POINT ( 'NONE',  ( -661.9833597215726968, 44.99899330872307246, 1.238957774783474797 ) ) ;
#4848 = CARTESIAN_POINT ( 'NONE',  ( -192.9588430854690273, -14.46834944099973264, 40.00000000000002132 ) ) ;
#4849 = B_SPLINE_CURVE_WITH_KNOTS ( 'NONE', 3,
 ( #24970, #6717, #12978, #14968, #2471, #16964, #20705, #10723, #8991, #10452, #2338, #24697, #12707, #8586, #6453, #12439, #23103, #15094, #24830, #2610, #4743, #16698, #6583, #10851, #18833, #14831 ),
 .UNSPECIFIED., .F., .F.,
 ( 4, 2, 1, 2, 2, 2, 2, 2, 2, 2, 2, 1, 2, 4 ),
 ( -5.999999999144898528E-08, 0.0004354487530732512827, 0.0008709575061464940775, 0.001741975012292979559, 0.003484010024585944883, 0.006968080049171870329, 0.01045215007375779707, 0.01393622009834372295, 0.02090436014751557645, 0.02438843017210149886, 0.02613046518439446353, 0.02700148269054095107, 0.02743699144361419484, 0.02787250019668744208 ),
 .UNSPECIFIED. ) ;
#4850 = CARTESIAN_POINT ( 'NONE',  ( 163.1118516004056573, 9.006482792073693844, 47.56205970284970164 ) ) ;
#4851 = CARTESIAN_POINT ( 'NONE',  ( 0.2972598230769983307, -14.33493731733933352, 40.00000000000002132 ) ) ;
#4852 = CARTESIAN_POINT ( 'NONE',  ( -614.3390598189121192, 30.96862867965382904, -32.65476733775240348 ) ) ;
#4853 = EDGE_LOOP ( 'NONE', ( #4992, #22520, #1464, #4722 ) ) ;
#4854 = CARTESIAN_POINT ( 'NONE',  ( 14.38125909742182529, -39.99999999999944578, -55.17850393971050238 ) ) ;
#4855 = DIRECTION ( 'NONE',  ( 0.000000000000000000, 0.000000000000000000, 1.000000000000000000 ) ) ;
#4856 = CARTESIAN_POINT ( 'NONE',  ( 200.0000000000000000, 69.29737539576909455, -75.30386416458597409 ) ) ;
#4857 = ORIENTED_EDGE ( 'NONE', *, *, #25450, .F. ) ;
#4858 = ORIENTED_EDGE ( 'NONE', *, *, #15559, .T. ) ;
#4859 = ORIENTED_EDGE ( 'NONE', *, *, #8837, .F. ) ;
#4860 = CARTESIAN_POINT ( 'NONE',  ( 0.2972598230769930572, 54.33493731733936016, 2.449293598294708485E-15 ) ) ;
#4861 = ADVANCED_FACE ( 'NONE', ( #11834 ), #1736, .F. ) ;
#4862 = CARTESIAN_POINT ( 'NONE',  ( -716.9846540392142060, 52.49999999999986500, 82.49999999999998579 ) ) ;
#4863 = AXIS2_PLACEMENT_3D ( 'NONE', #3824, #17770, #17904 ) ;
#4864 = CARTESIAN_POINT ( 'NONE',  ( -110.0737093975827747, -19.58505513374902662, 5.042781230409048021 ) ) ;
#4865 = DIRECTION ( 'NONE',  ( -0.2259624730540135129, 0.000000000000000000, -0.9741360073271668751 ) ) ;
#4866 = CARTESIAN_POINT ( 'NONE',  ( -192.9588430854690273, -40.00000000000011369, 14.46834944099955855 ) ) ;
#4867 = CARTESIAN_POINT ( 'NONE',  ( 200.0000000000001705, 1.541304384858841692, -18.93928971938424155 ) ) ;
#4868 = CARTESIAN_POINT ( 'NONE',  ( 199.9999999999999716, -6.703600881535439093, -17.78416426705615550 ) ) ;
#4869 = CARTESIAN_POINT ( 'NONE',  ( -30.26275506840324070, -27.08623969584554558, -29.48230279907826912 ) ) ;
#4870 = CARTESIAN_POINT ( 'NONE',  ( -192.9588430854689989, -10.23066800230742501, -10.23066800230756712 ) ) ;
#4871 = CARTESIAN_POINT ( 'NONE',  ( -114.6380801921741011, -18.98799529646051454, -11.20622827607009597 ) ) ;
#4872 = CARTESIAN_POINT ( 'NONE',  ( 4.995406935893306866, -39.99999999999944578, -55.24977328856505920 ) ) ;
#4873 = CARTESIAN_POINT ( 'NONE',  ( -97.72675010090193837, -8.185591577777461936, 20.89622088363365648 ) ) ;
#4874 = DIRECTION ( 'NONE',  ( 0.000000000000000000, 0.6739498806388345420, 0.7387770694782699321 ) ) ;
#4875 = ADVANCED_FACE ( 'NONE', ( #8507 ), #16185, .F. ) ;
#4876 = CARTESIAN_POINT ( 'NONE',  ( -162.0762913951020607, -1.198031840455708430, 57.76657433537920383 ) ) ;
#4877 = CARTESIAN_POINT ( 'NONE',  ( 199.0053211798077086, 14.13837298227953987, -14.13837298578013701 ) ) ;
#4879 = CARTESIAN_POINT ( 'NONE',  ( 200.0000000000000000, 40.00000000000012790, -19.99999999999996092 ) ) ;
#4878 = CARTESIAN_POINT ( 'NONE',  ( 19.06497207195980792, 10.03556273973447155, -10.03556273973422286 ) ) ;
#4880 = DIRECTION ( 'NONE',  ( 1.000000000000000000, -1.937599346585394162E-16, -0.000000000000000000 ) ) ;
#4881 = CARTESIAN_POINT ( 'NONE',  ( 57.59792236341147031, -1.722363176415123043, 54.84617931850879557 ) ) ;
#4882 = CARTESIAN_POINT ( 'NONE',  ( -208.1127848780264742, 15.00245453012665742, 40.00000000000002132 ) ) ;
#4883 = EDGE_LOOP ( 'NONE', ( #14685, #25180, #18872, #7123 ) ) ;
#4884 = CARTESIAN_POINT ( 'NONE',  ( 20.69615274311347974, -43.59383154590178577, 23.88537831998399241 ) ) ;
#4885 = CARTESIAN_POINT ( 'NONE',  ( -56.48582580120559982, -9.153146818113595984, -40.00000000000002132 ) ) ;
#4886 = CARTESIAN_POINT ( 'NONE',  ( 170.0000000000000284, -24.95097643316995928, -3.062538285713102937 ) ) ;
#4887 = CARTESIAN_POINT ( 'NONE',  ( -213.1075012329537230, 37.98287015391228749, 37.98287015391245802 ) ) ;
#4888 = CARTESIAN_POINT ( 'NONE',  ( 19.06497207195981858, -40.00000000000007105, 14.19242893257826665 ) ) ;
#4889 = CARTESIAN_POINT ( 'NONE',  ( -77.59213678343638776, 21.93717451302018517, 2.696620339532176835 ) ) ;
#4890 = CARTESIAN_POINT ( 'NONE',  ( 14.32711937312299355, -14.14294248749784089, -49.08922911798412514 ) ) ;
#4891 = CARTESIAN_POINT ( 'NONE',  ( 199.0263095778509808, -15.67393427090936875, 12.43211889955359162 ) ) ;
#4892 = B_SPLINE_CURVE_WITH_KNOTS ( 'NONE', 3,
 ( #17968, #11993, #10266, #15975, #9998, #24511 ),
 .UNSPECIFIED., .F., .F.,
 ( 4, 2, 4 ),
 ( -0.0001324603514674868305, 0.04003846212280023908, 0.08020938459706797308 ),
 .UNSPECIFIED. ) ;
#4893 = CARTESIAN_POINT ( 'NONE',  ( -280.0000000000000568, 14.14213562373038968, 42.42640687119305198 ) ) ;
#4894 = CARTESIAN_POINT ( 'NONE',  ( -626.9846540392142060, 105.0000000000000000, -46.18033988749894547 ) ) ;
#4895 = DIRECTION ( 'NONE',  ( 1.000000000000000000, 1.836970198721030181E-16, 0.000000000000000000 ) ) ;
#4896 = CARTESIAN_POINT ( 'NONE',  ( -188.4265466358232572, -23.47687925214823323, 43.04237830659958064 ) ) ;
#4897 = CARTESIAN_POINT ( 'NONE',  ( -30.26275506840324070, 1.218738420030236455E-14, -1.694272468446259783 ) ) ;
#4898 = CARTESIAN_POINT ( 'NONE',  ( -86.96347745069644475, 15.38646221621793586, -15.38646221621778842 ) ) ;
#4899 = CARTESIAN_POINT ( 'NONE',  ( -213.1075012329537230, -18.58567234101102272, -37.98287015391260013 ) ) ;
#4900 = CARTESIAN_POINT ( 'NONE',  ( -200.0000000000000000, 6.162975822039154730E-30, 0.000000000000000000 ) ) ;
#4902 = CARTESIAN_POINT ( 'NONE',  ( -198.0356074513804572, 67.44298959250878056, -10.87444709758402261 ) ) ;
#4901 = CARTESIAN_POINT ( 'NONE',  ( -30.26275506840325136, 27.08623969584614244, -29.48230279907770779 ) ) ;
#4903 = CARTESIAN_POINT ( 'NONE',  ( -259.2033419157646676, -6.730120644402966867, -49.83842185052038332 ) ) ;
#4904 = CARTESIAN_POINT ( 'NONE',  ( 184.8905102610680444, 19.07866798485562398, -40.00000000000002132 ) ) ;
#4905 = CARTESIAN_POINT ( 'NONE',  ( 19.06497207195979726, 38.31983398719629719, -18.24870850772750686 ) ) ;
#4906 = CARTESIAN_POINT ( 'NONE',  ( -575.0231298121445889, 90.00000000000000000, 34.99999999999821654 ) ) ;
#4907 = CARTESIAN_POINT ( 'NONE',  ( 14.38125909742181818, -39.01709431150928253, 17.55144818341435808 ) ) ;
#4908 = CARTESIAN_POINT ( 'NONE',  ( -188.2870673237559060, 46.98612534495561022, -13.82722856953786206 ) ) ;
#4909 = ORIENTED_EDGE ( 'NONE', *, *, #18736, .F. ) ;
#4910 = CARTESIAN_POINT ( 'NONE',  ( -280.0000000000000000, 14.14213562373088351, 14.14213562373098654 ) ) ;
#4911 = CARTESIAN_POINT ( 'NONE',  ( -96.93773665438899911, -20.92028269119435180, -8.190703376740806618 ) ) ;
#4912 = CARTESIAN_POINT ( 'NONE',  ( 4.995406935893301537, -10.78321810390187530, 67.35176059882529387 ) ) ;
#4913 = LINE ( 'NONE', #9032, #23004 ) ;
#4914 = EDGE_LOOP ( 'NONE', ( #22151, #2094 ) ) ;
#4915 = CARTESIAN_POINT ( 'NONE',  ( -183.6284948307073819, -41.87131864454406127, 17.34366805704014780 ) ) ;
#4916 = CARTESIAN_POINT ( 'NONE',  ( 199.9999999999998863, 12.98615309696526587, -13.88358464575571283 ) ) ;
#4917 = CARTESIAN_POINT ( 'NONE',  ( 0.4226707250629899715, 14.03458789212690938, -48.37218667320253473 ) ) ;
#4918 = ADVANCED_FACE ( 'NONE', ( #16621 ), #17409, .T. ) ;
#4919 = CARTESIAN_POINT ( 'NONE',  ( 184.8905102610680444, 19.07866798485562043, 2.449293598294708485E-15 ) ) ;
#4920 = CARTESIAN_POINT ( 'NONE',  ( 35.93739820626764470, 38.99308227184688036, -20.78453043603687433 ) ) ;
#4921 = CARTESIAN_POINT ( 'NONE',  ( 199.0125740919301336, 17.92725630381683644, 8.864156431172764528 ) ) ;
#4922 = AXIS2_PLACEMENT_3D ( 'NONE', #7360, #19350, #19866 ) ;
#4923 = EDGE_CURVE ( 'NONE', #1984, #6082, #2193, .T. ) ;
#4924 = CARTESIAN_POINT ( 'NONE',  ( 192.4448373802101173, -14.14213562370342281, 42.42640687122062104 ) ) ;
#4925 = CARTESIAN_POINT ( 'NONE',  ( -30.26275506840323359, -40.00000000000017053, 41.69427246844613677 ) ) ;
#4926 = CARTESIAN_POINT ( 'NONE',  ( -56.48582580120559982, 39.99999999999990763, 30.84685318188658698 ) ) ;
#4927 = DIRECTION ( 'NONE',  ( -1.000000000000000000, -1.836970198721030181E-16, -0.000000000000000000 ) ) ;
#4928 = CARTESIAN_POINT ( 'NONE',  ( 200.0000000000000000, 20.00000000000013856, -40.00000000000002132 ) ) ;
#4930 = CARTESIAN_POINT ( 'NONE',  ( -613.5337413356613752, 29.67126750635895149, 26.83244280794799153 ) ) ;
#4929 = CARTESIAN_POINT ( 'NONE',  ( 23.26364522860123785, -23.36474233297011338, -42.89098160628034151 ) ) ;
#4931 = EDGE_CURVE ( 'NONE', #16948, #15141, #22345, .T. ) ;
#4932 = CARTESIAN_POINT ( 'NONE',  ( -192.9588430854690273, -14.46834944099973264, 40.00000000000002132 ) ) ;
#4933 = EDGE_CURVE ( 'NONE', #4362, #18547, #12126, .T. ) ;
#4935 = CARTESIAN_POINT ( 'NONE',  ( 91.82158438592158234, 12.16597498397773869, -12.16597498397759303 ) ) ;
#4934 = AXIS2_PLACEMENT_3D ( 'NONE', #10843, #11349, #15346 ) ;
#4936 = VECTOR ( 'NONE', #14558, 1000.000000000000114 ) ;
#4937 = AXIS2_PLACEMENT_3D ( 'NONE', #18995, #2499, #11135 ) ;
#4938 = CARTESIAN_POINT ( 'NONE',  ( -105.3755690713226585, 39.99999999999977263, 21.75974354311691883 ) ) ;
#4939 = CARTESIAN_POINT ( 'NONE',  ( -105.2053629887423796, 15.67233752942116176, -14.72427054405869917 ) ) ;
#4940 = CARTESIAN_POINT ( 'NONE',  ( -105.3755690713226585, -40.00000000000027711, 21.75974354311608749 ) ) ;
#4941 = CYLINDRICAL_SURFACE ( 'NONE', #11428, 5.000000000000004441 ) ;
#4942 = CARTESIAN_POINT ( 'NONE',  ( -65.65550967573157948, -24.04430752632008961, 11.16467289560384835 ) ) ;
#4943 = CARTESIAN_POINT ( 'NONE',  ( 163.1118516004056573, -19.27778845538787422, 19.27778845538743724 ) ) ;
#4944 = CARTESIAN_POINT ( 'NONE',  ( -30.26275506840325136, 27.08623969584573388, 29.48230279907808793 ) ) ;
#4945 = EDGE_LOOP ( 'NONE', ( #23397, #466, #21424, #17582, #15581, #26118 ) ) ;
#4947 = CARTESIAN_POINT ( 'NONE',  ( -199.9999999999998010, 24.82633483071100500, -44.86878812508844305 ) ) ;
#4946 = CARTESIAN_POINT ( 'NONE',  ( 57.59792236341147031, 1.722363176415040886, 1.722363176415060426 ) ) ;
#4948 = CARTESIAN_POINT ( 'NONE',  ( 164.1122551457365262, 24.38379312608506666, -10.10009781492404635 ) ) ;
#4949 = CARTESIAN_POINT ( 'NONE',  ( 151.7948205124836250, -6.767089262349004208, -2.449293598294708485E-15 ) ) ;
#4950 = CARTESIAN_POINT ( 'NONE',  ( -726.9846540392142060, -66.50000000000001421, 66.50000000000005684 ) ) ;
#4951 = CARTESIAN_POINT ( 'NONE',  ( -114.7826396787321954, 1.398624481943209208, -22.13135001986790940 ) ) ;
#4952 = EDGE_LOOP ( 'NONE', ( #16647, #11731, #22184, #11956 ) ) ;
#4953 = ORIENTED_EDGE ( 'NONE', *, *, #21445, .F. ) ;
#4954 = AXIS2_PLACEMENT_3D ( 'NONE', #21453, #21333, #23575 ) ;
#4955 = CARTESIAN_POINT ( 'NONE',  ( 199.9999999999999432, -10.30972604295016559, 15.97265043433685250 ) ) ;
#4956 = CARTESIAN_POINT ( 'NONE',  ( -93.01741312767317993, 8.169811846188826721, -20.82169463882216576 ) ) ;
#4957 = EDGE_LOOP ( 'NONE', ( #12266, #4589, #12791, #9802 ) ) ;
#4958 = ORIENTED_EDGE ( 'NONE', *, *, #2792, .F. ) ;
#4959 = CARTESIAN_POINT ( 'NONE',  ( 199.0250768083106436, -19.24006491846622069, 5.486913247009519878 ) ) ;
#4960 = CARTESIAN_POINT ( 'NONE',  ( -114.5444905533463356, -6.798574478255778430, 20.85462941671082859 ) ) ;
#4961 = CIRCLE ( 'NONE', #9195, 5.000000000000004441 ) ;
#4962 = CARTESIAN_POINT ( 'NONE',  ( -135.8532207217289738, -34.75652343174615311, 21.81201906317767936 ) ) ;
#4963 = CARTESIAN_POINT ( 'NONE',  ( -105.4415978763232147, 19.97871834610316455, 7.511821620885758222 ) ) ;
#4964 = CARTESIAN_POINT ( 'NONE',  ( -280.0000000000000568, 40.00000000000004263, -19.99999999999987210 ) ) ;
#4965 = CARTESIAN_POINT ( 'NONE',  ( -716.9846540392142060, 52.49999999999991473, -82.49999999999998579 ) ) ;
#4966 = DIRECTION ( 'NONE',  ( 0.000000000000000000, -1.000000000000000000, 0.000000000000000000 ) ) ;
#4967 = CARTESIAN_POINT ( 'NONE',  ( -198.0356074513804572, -39.99999999999948130, -55.37879056874863437 ) ) ;
#4968 = CARTESIAN_POINT ( 'NONE',  ( -208.1127848780265026, 5.403397259664334602E-13, -55.00245453012672670 ) ) ;
#4969 = CARTESIAN_POINT ( 'NONE',  ( -114.6375327213470143, -18.99176668987167105, 11.19832436705239687 ) ) ;
#4970 = AXIS2_PLACEMENT_3D ( 'NONE', #10637, #4262, #2255 ) ;
#4971 = DIRECTION ( 'NONE',  ( 1.000000000000000000, 1.836970198721030181E-16, 0.000000000000000000 ) ) ;
#4972 = CARTESIAN_POINT ( 'NONE',  ( 199.0055651108938832, 16.81514173603054374, -10.81990435933588302 ) ) ;
#4973 = EDGE_CURVE ( 'NONE', #9342, #8967, #1524, .T. ) ;
#4974 = CARTESIAN_POINT ( 'NONE',  ( -192.9588430854689989, -10.23066800230756890, 10.23066800230742501 ) ) ;
#4975 = CARTESIAN_POINT ( 'NONE',  ( 130.8568914410475372, 24.07718906447210472, 24.07718906447249907 ) ) ;
#4976 = CARTESIAN_POINT ( 'NONE',  ( -188.2995950289364941, -46.99046209955528042, 13.82811170417144453 ) ) ;
#4977 = CARTESIAN_POINT ( 'NONE',  ( -30.26275506840324070, -1.198031551616032919, 1.198031551616014712 ) ) ;
#4978 = CARTESIAN_POINT ( 'NONE',  ( -86.86493150571111244, -8.366608963953618527, 19.60045294882771572 ) ) ;
#4979 = CARTESIAN_POINT ( 'NONE',  ( 163.1118516004056573, -9.006482792069506971, -9.006482792069697041 ) ) ;
#4980 = CARTESIAN_POINT ( 'NONE',  ( -184.9730489281237737, -13.59277546675971671, -45.83721239347640619 ) ) ;
#4981 = DIRECTION ( 'NONE',  ( 0.000000000000000000, -1.000000000000000000, 0.000000000000000000 ) ) ;
#4982 = ORIENTED_EDGE ( 'NONE', *, *, #25512, .F. ) ;
#4983 = CARTESIAN_POINT ( 'NONE',  ( 130.8568914410475088, 4.207082182989012153, 52.36146031193425188 ) ) ;
#4984 = CARTESIAN_POINT ( 'NONE',  ( -199.9999999999999432, 43.68705981750494516, 18.09577267661451927 ) ) ;
#4985 = AXIS2_PLACEMENT_3D ( 'NONE', #14141, #11740, #24261 ) ;
#4986 = CARTESIAN_POINT ( 'NONE',  ( -601.6309025357880955, 37.98336425937555560, 24.13488029792940637 ) ) ;
#4987 = EDGE_LOOP ( 'NONE', ( #4034, #1852, #15513, #10536 ) ) ;
#4988 = CARTESIAN_POINT ( 'NONE',  ( 146.6084372240433993, 8.568076647504290689E-14, -5.374981219216972583 ) ) ;
#4989 = CARTESIAN_POINT ( 'NONE',  ( 199.0117626354723370, -7.365673525892063367, -18.59241149604612886 ) ) ;
#4990 = CARTESIAN_POINT ( 'NONE',  ( 199.9999999999999432, -20.00000000000006750, 0.000000000000000000 ) ) ;
#4991 = ORIENTED_EDGE ( 'NONE', *, *, #22077, .F. ) ;
#4992 = ORIENTED_EDGE ( 'NONE', *, *, #22984, .T. ) ;
#4993 = ORIENTED_EDGE ( 'NONE', *, *, #14820, .T. ) ;
#4994 = CARTESIAN_POINT ( 'NONE',  ( 146.6084372240433993, 5.374981219216999229, 2.449293598294708485E-15 ) ) ;
#4995 = DIRECTION ( 'NONE',  ( 0.000000000000000000, -1.000000000000000000, 0.000000000000000000 ) ) ;
#4996 = VECTOR ( 'NONE', #6901, 1000.000000000000000 ) ;
#4997 = CARTESIAN_POINT ( 'NONE',  ( -575.0231298121466352, 90.00000000000000000, -30.00000000000202505 ) ) ;
#4998 = CARTESIAN_POINT ( 'NONE',  ( -91.56559293963834989, -39.99999999999995737, -22.67402823373205933 ) ) ;
#4999 = CARTESIAN_POINT ( 'NONE',  ( 200.0000000000000284, -15.63511319855579629, -10.80754414709790190 ) ) ;
#5000 = DIRECTION ( 'NONE',  ( -1.000000000000000000, 0.000000000000000000, 0.000000000000000000 ) ) ;
#5001 = CARTESIAN_POINT ( 'NONE',  ( 0.2972598230769938343, 10.13633138497486286, -10.13633138497461594 ) ) ;
#5002 = CARTESIAN_POINT ( 'NONE',  ( 91.82158438592156813, -16.11829626348459144, 40.45024623143943643 ) ) ;
#5003 = CARTESIAN_POINT ( 'NONE',  ( -114.7544849857915636, -17.49519532552859857, -13.58498122706649447 ) ) ;
#5004 = CARTESIAN_POINT ( 'NONE',  ( 14.38125909742181818, 5.830552384690105017E-13, -55.17850393972636880 ) ) ;
#5005 = CARTESIAN_POINT ( 'NONE',  ( -162.0762913951020892, -1.198031840385767266, -1.198031840385758384 ) ) ;
#5006 = CARTESIAN_POINT ( 'NONE',  ( 91.82158438592156813, 17.20528682183302038, -40.00000000000002132 ) ) ;
#5007 = CARTESIAN_POINT ( 'NONE',  ( -100.7734535825088358, -12.25131212657493052, 12.25131212657478130 ) ) ;
#5008 = CARTESIAN_POINT ( 'NONE',  ( 199.0061264496102353, 18.45002901997423095, -7.707159767720078491 ) ) ;
#5010 = CARTESIAN_POINT ( 'NONE',  ( 136.1360204305621266, 1.473277640373554421E-13, -35.03383547441296741 ) ) ;
#5009 = CARTESIAN_POINT ( 'NONE',  ( 146.6084372240433709, -52.76785682606510619, -3.800685668859292043 ) ) ;
#5011 = CARTESIAN_POINT ( 'NONE',  ( 146.6084372240433993, -34.62501878078303008, 0.000000000000000000 ) ) ;
#5012 = CARTESIAN_POINT ( 'NONE',  ( 184.8905102610680444, -14.79361573936379415, -14.79361573936387941 ) ) ;
#5013 = CARTESIAN_POINT ( 'NONE',  ( 14.38125909742180752, 15.17850393972634038, 0.000000000000000000 ) ) ;
#5014 = ORIENTED_EDGE ( 'NONE', *, *, #687, .T. ) ;
#5015 = CARTESIAN_POINT ( 'NONE',  ( 21.80824205438601382, -47.36272483143281420, 13.88338701303066713 ) ) ;
#5016 = CARTESIAN_POINT ( 'NONE',  ( -30.26275506840324425, 1.694272468446254232, -40.00000000000002132 ) ) ;
#5017 = EDGE_CURVE ( 'NONE', #3113, #5353, #13865, .T. ) ;
#5018 = FACE_OUTER_BOUND ( 'NONE', #24466, .T. ) ;
#5019 = CARTESIAN_POINT ( 'NONE',  ( 192.4448373802101173, -14.14213562375886291, 42.42640687116498555 ) ) ;
#5020 = DIRECTION ( 'NONE',  ( 0.000000000000000000, 0.000000000000000000, 1.000000000000000000 ) ) ;
#5021 = CARTESIAN_POINT ( 'NONE',  ( -87.13238242893044116, 21.48515709343678282, 0.8941846428760004128 ) ) ;
#5022 = LINE ( 'NONE', #2765, #8306 ) ;
#5023 = CARTESIAN_POINT ( 'NONE',  ( 199.0227232939661519, -19.93874224789216143, -1.638880401382246443 ) ) ;
#5024 = CARTESIAN_POINT ( 'NONE',  ( 14.38125909742180220, 39.01709431150892016, 17.55144818341517166 ) ) ;
#5025 = ADVANCED_FACE ( 'NONE', ( #18122 ), #1777, .F. ) ;
#5026 = DIRECTION ( 'NONE',  ( 0.000000000000000000, -1.000000000000000000, 0.000000000000000000 ) ) ;
#5027 = CARTESIAN_POINT ( 'NONE',  ( -280.0000000000000000, 14.14213562373098299, -14.14213562373088706 ) ) ;
#5028 = CARTESIAN_POINT ( 'NONE',  ( 151.7948205124836250, 23.49921654116328540, 23.49921654116366554 ) ) ;
#5029 = EDGE_CURVE ( 'NONE', #5443, #17669, #6188, .T. ) ;
#5030 = CARTESIAN_POINT ( 'NONE',  ( -135.8532207217289738, 6.472252184284186249, -6.472252184284142729 ) ) ;
#5031 = PLANE ( 'NONE',  #2352 ) ;
#5032 = DIRECTION ( 'NONE',  ( 0.000000000000000000, 1.000000000000000000, 0.000000000000000000 ) ) ;
#5034 = CARTESIAN_POINT ( 'NONE',  ( 130.8568914410475088, 32.49135343045448820, 24.07718906446946860 ) ) ;
#5033 = CARTESIAN_POINT ( 'NONE',  ( 151.7948205124836250, 23.49921654116328540, 23.49921654116366554 ) ) ;
#5035 = CARTESIAN_POINT ( 'NONE',  ( 4.995406935893286438, 67.35176059880245703, -10.78321810387767066 ) ) ;
#5036 = CARTESIAN_POINT ( 'NONE',  ( 4.995406935893288214, 15.24977328854832770, -40.00000000000002132 ) ) ;
#5037 = CARTESIAN_POINT ( 'NONE',  ( -135.8532207217289738, -6.472252184284190690, -6.472252184284188914 ) ) ;
#5038 =( BOUNDED_CURVE ( )  B_SPLINE_CURVE ( 3, ( #25463, #15579, #13215, #15206 ),
 .UNSPECIFIED., .F., .F. ) 
 B_SPLINE_CURVE_WITH_KNOTS ( ( 4, 4 ),
 ( 0.01388163287021914639, 0.02359082919309998458 ),
 .UNSPECIFIED. ) 
 CURVE ( )  GEOMETRIC_REPRESENTATION_ITEM ( )  RATIONAL_B_SPLINE_CURVE ( ( 1.000000000000000000, 0.8672072324488988571, 0.7608653435686189015, 0.6809743333591601333 ) ) 
 REPRESENTATION_ITEM ( '' )  );
#5039 = CARTESIAN_POINT ( 'NONE',  ( -208.1127848780265026, -9.061048840815752106E-14, 15.00245453012669472 ) ) ;
#5040 = CARTESIAN_POINT ( 'NONE',  ( -86.96347745069643054, -41.18208027870611687, 15.38646221621750954 ) ) ;
#5041 = CARTESIAN_POINT ( 'NONE',  ( -188.2652133075324343, 42.99509596150244306, -23.44262061655331308 ) ) ;
#5042 = ORIENTED_EDGE ( 'NONE', *, *, #15894, .T. ) ;
#5043 = CARTESIAN_POINT ( 'NONE',  ( -30.26275506840323715, 29.48230279907789253, 29.48230279907799556 ) ) ;
#5044 = DIRECTION ( 'NONE',  ( -1.303213150798907793E-16, 1.000000000000000000, -1.682156097916904081E-16 ) ) ;
#5045 = CARTESIAN_POINT ( 'NONE',  ( -24.53392603776244485, -36.88304647107583634, -19.42583462365220015 ) ) ;
#5046 = ORIENTED_EDGE ( 'NONE', *, *, #4366, .F. ) ;
#5047 = CARTESIAN_POINT ( 'NONE',  ( -105.4894168351564048, 19.67999904371083275, 8.151722511394638104 ) ) ;
#5048 = CARTESIAN_POINT ( 'NONE',  ( 199.9999999999998863, -2.943496653232010374, -18.77345647985907462 ) ) ;
#5049 = CARTESIAN_POINT ( 'NONE',  ( 83.11963132830025813, -9.001241435568109850, 24.42551322431495819 ) ) ;
#5050 = VECTOR ( 'NONE', #7667, 1000.000000000000000 ) ;
#5051 = CARTESIAN_POINT ( 'NONE',  ( -208.1127848780265026, 15.00245453012665564, 0.000000000000000000 ) ) ;
#5052 = DIRECTION ( 'NONE',  ( 0.000000000000000000, 0.000000000000000000, -1.000000000000000000 ) ) ;
#5053 = CARTESIAN_POINT ( 'NONE',  ( 199.0196638708318631, 8.237985373594881366, 18.22956011771260165 ) ) ;
#5054 = CARTESIAN_POINT ( 'NONE',  ( 192.4448373802101173, -42.42640687116510634, 14.14213562375845257 ) ) ;
#5055 = CARTESIAN_POINT ( 'NONE',  ( -208.1127848780264742, 39.99999999999992895, 15.00245453012683683 ) ) ;
#5056 = DIRECTION ( 'NONE',  ( -0.000000000000000000, 0.000000000000000000, 1.000000000000000000 ) ) ;
#5057 = CARTESIAN_POINT ( 'NONE',  ( 3.854699808470055444, 48.95177852071795854, -14.12217777258769047 ) ) ;
#5058 = CARTESIAN_POINT ( 'NONE',  ( 57.59792236341148453, -37.56421063658185489, -40.00000000000002132 ) ) ;
#5060 = DIRECTION ( 'NONE',  ( -1.000000000000000000, 0.000000000000000000, 0.000000000000000000 ) ) ;
#5059 = CARTESIAN_POINT ( 'NONE',  ( 23.58679727197007736, -23.29637218065869675, -42.79169916605220436 ) ) ;
#5061 = CARTESIAN_POINT ( 'NONE',  ( 14.38125909742181285, -15.17850393972633505, 40.00000000000002132 ) ) ;
#5062 = CARTESIAN_POINT ( 'NONE',  ( 163.1118516004056573, 19.27778845538780317, -19.27778845538757224 ) ) ;
#5063 = CARTESIAN_POINT ( 'NONE',  ( 163.1118516004056573, -2.556006622855449647E-13, 27.26290988616872824 ) ) ;
#5064 = CARTESIAN_POINT ( 'NONE',  ( -105.3901353554191900, 9.627478968577326768, -19.08722479148772067 ) ) ;
#5065 = CARTESIAN_POINT ( 'NONE',  ( 170.2234770963711128, -39.99999999999982947, -15.44714144992858529 ) ) ;
#5066 = CARTESIAN_POINT ( 'NONE',  ( 199.0257180514102799, -8.261434504147922908, 18.22213678534573589 ) ) ;
#5067 = CARTESIAN_POINT ( 'NONE',  ( -77.90255099906772784, 20.04994828523968664, -8.644468104261312291 ) ) ;
#5068 = CARTESIAN_POINT ( 'NONE',  ( -192.9588430854690273, 66.79921049724377724, -10.23066800231904239 ) ) ;
#5069 = CARTESIAN_POINT ( 'NONE',  ( -198.0356074513804572, 17.40982414986446969, 39.15871834505921356 ) ) ;
#5070 = ORIENTED_EDGE ( 'NONE', *, *, #8188, .T. ) ;
#5072 = CARTESIAN_POINT ( 'NONE',  ( -3.977426076247482900, 43.16039317622643523, -17.87762021094837195 ) ) ;
#5071 = DIRECTION ( 'NONE',  ( 0.000000000000000000, 0.000000000000000000, -1.000000000000000000 ) ) ;
#5073 = B_SPLINE_CURVE_WITH_KNOTS ( 'NONE', 3,
 ( #12279, #25865, #6035, #3916, #15724, #12015, #5627, #18126, #15999, #14005, #6162, #10156, #16131, #17988, #20135, #9753, #8153, #7741, #1913, #7609, #18259, #23982 ),
 .UNSPECIFIED., .F., .F.,
 ( 4, 2, 2, 2, 2, 2, 2, 2, 2, 2, 4 ),
 ( 0.005049353704792979534, 0.02738431423455156208, 0.04971927476431014375, 0.07205423529406872196, 0.07763797542650840988, 0.08042984549272826078, 0.08182578052583817929, 0.08322171555894809780, 0.08880545569138770245, 0.09159732575760753948, 0.09438919582382739037 ),
 .UNSPECIFIED. ) ;
#5074 = CARTESIAN_POINT ( 'NONE',  ( 130.8568914410475088, 34.05028731879790627, 40.00000000000002132 ) ) ;
#5075 = EDGE_CURVE ( 'NONE', #218, #24643, #19992, .T. ) ;
#5076 = CARTESIAN_POINT ( 'NONE',  ( -175.9234132810913991, -42.70618379831009293, 12.95567001217066760 ) ) ;
#5077 = CARTESIAN_POINT ( 'NONE',  ( -109.1264249741455785, -33.12752917269520481, -13.72187187123273233 ) ) ;
#5078 = DIRECTION ( 'NONE',  ( 1.000000000000000000, 0.000000000000000000, 0.000000000000000000 ) ) ;
#5079 = EDGE_LOOP ( 'NONE', ( #1119, #10639 ) ) ;
#5080 = ORIENTED_EDGE ( 'NONE', *, *, #11566, .F. ) ;
#5081 = CARTESIAN_POINT ( 'NONE',  ( 4.995406935893293543, -10.78321810389005364, 10.78321810388994173 ) ) ;
#5082 = CARTESIAN_POINT ( 'NONE',  ( 35.93765801236255442, -38.99300236445704115, -20.78447758918573385 ) ) ;
#5083 = ORIENTED_EDGE ( 'NONE', *, *, #306, .F. ) ;
#5084 = ORIENTED_EDGE ( 'NONE', *, *, #17492, .F. ) ;
#5085 = CARTESIAN_POINT ( 'NONE',  ( 199.9999999999998579, 3.088973468740698447, 18.75625871509165776 ) ) ;
#5086 = DIRECTION ( 'NONE',  ( -1.000000000000000000, 1.836970198721030181E-16, 0.000000000000000000 ) ) ;
#5087 = ADVANCED_FACE ( 'NONE', ( #9882 ), #24163, .T. ) ;
#5088 = CARTESIAN_POINT ( 'NONE',  ( 146.6084372240433709, -52.76785682606516303, 3.800685668858563737 ) ) ;
#5089 = CARTESIAN_POINT ( 'NONE',  ( -208.1127848780265026, 10.60833733269537049, 10.60833733269544510 ) ) ;
#5090 = CARTESIAN_POINT ( 'NONE',  ( 136.1360204305621551, 40.00000000000017053, -35.03383547441281820 ) ) ;
#5091 = DIRECTION ( 'NONE',  ( 0.000000000000000000, 1.000000000000000000, 0.000000000000000000 ) ) ;
#5092 = FACE_BOUND ( 'NONE', #7433, .T. ) ;
#5093 = CARTESIAN_POINT ( 'NONE',  ( -192.9588430854690273, -39.99999999999991473, -14.46834944100011633 ) ) ;
#5094 = CARTESIAN_POINT ( 'NONE',  ( -192.9588430854689989, 5.375290060580374156E-13, -54.46834944099972375 ) ) ;
#5095 = CARTESIAN_POINT ( 'NONE',  ( -82.23726319253047734, 14.74589317219750662, 13.81439526601152679 ) ) ;
#5096 = CARTESIAN_POINT ( 'NONE',  ( -30.26275506840324070, -29.48230279907780016, -27.08623969584605362 ) ) ;
#5097 = CARTESIAN_POINT ( 'NONE',  ( -200.0000000000000284, 23.83302776610025475, -44.89135967046703257 ) ) ;
#5098 = CARTESIAN_POINT ( 'NONE',  ( -200.0000000000000000, -71.50000000000002842, -66.50000000000005684 ) ) ;
#5099 = CARTESIAN_POINT ( 'NONE',  ( -716.9846540392142060, 52.50000000000007816, -52.49999999999999289 ) ) ;
#5100 = AXIS2_PLACEMENT_3D ( 'NONE', #22642, #8795, #2546 ) ;
#5101 = DIRECTION ( 'NONE',  ( 0.000000000000000000, 0.9307566067254452458, -0.3656393565207865515 ) ) ;
#5102 = CARTESIAN_POINT ( 'NONE',  ( 200.0000000000000000, 42.42640687119290988, 14.14213562373111976 ) ) ;
#5103 = CARTESIAN_POINT ( 'NONE',  ( -77.67315633213154058, -18.60060890639466180, 11.80559230995901387 ) ) ;
#5104 = CARTESIAN_POINT ( 'NONE',  ( -162.0762913951021176, -29.48230308784793152, 27.08623940707591515 ) ) ;
#5105 = CARTESIAN_POINT ( 'NONE',  ( -626.9846540392142060, 28.28427124746186294, -34.99999999999999289 ) ) ;
#5106 = CARTESIAN_POINT ( 'NONE',  ( -200.0000000000000000, -66.50000000000001421, 66.50000000000005684 ) ) ;
#5107 = EDGE_LOOP ( 'NONE', ( #3352, #6536, #18275, #8400 ) ) ;
#5108 = CARTESIAN_POINT ( 'NONE',  ( 14.38125909742180397, 67.30136555898270956, -10.73282306405792319 ) ) ;
#5109 = DIRECTION ( 'NONE',  ( 0.000000000000000000, 1.000000000000000000, 0.000000000000000000 ) ) ;
#5110 = EDGE_CURVE ( 'NONE', #10128, #2915, #19778, .T. ) ;
#5111 = CARTESIAN_POINT ( 'NONE',  ( -105.2054292635175585, -2.444554031225951202E-13, 21.49321519473985020 ) ) ;
#5112 = ORIENTED_EDGE ( 'NONE', *, *, #697, .F. ) ;
#5113 = CARTESIAN_POINT ( 'NONE',  ( 151.7948205124836534, -40.00000000000034817, 33.23291073765511072 ) ) ;
#5114 = CARTESIAN_POINT ( 'NONE',  ( 199.0199587825621563, -18.46922402431326304, -7.678974719652290837 ) ) ;
#5115 = CARTESIAN_POINT ( 'NONE',  ( -4.039451493210496125, 23.44932283416649454, 43.00522595894017286 ) ) ;
#5116 = ORIENTED_EDGE ( 'NONE', *, *, #11656, .T. ) ;
#5117 = VERTEX_POINT ( 'NONE', #19250 ) ;
#5118 = CARTESIAN_POINT ( 'NONE',  ( -208.1127848780264742, 55.00245453010919050, -40.00000000000002132 ) ) ;
#5119 = UNCERTAINTY_MEASURE_WITH_UNIT (LENGTH_MEASURE( 1.000000000000000082E-05 ), #23048, 'distance_accuracy_value', 'NONE');
#5120 = ADVANCED_FACE ( 'NONE', ( #10609 ), #21450, .T. ) ;
#5121 = EDGE_CURVE ( 'NONE', #2152, #25083, #18521, .T. ) ;
#5122 = CARTESIAN_POINT ( 'NONE',  ( -100.0968563617265943, -20.41799937594479530, -8.893120081421919565 ) ) ;
#5123 = CIRCLE ( 'NONE', #19140, 9.999999999999996447 ) ;
#5124 = CARTESIAN_POINT ( 'NONE',  ( -220.0000000000000284, 61.50000000000001421, -66.50000000000005684 ) ) ;
#5125 = CARTESIAN_POINT ( 'NONE',  ( 57.59792236341148453, -40.00000000000000000, -2.435789363418300546 ) ) ;
#5126 = CARTESIAN_POINT ( 'NONE',  ( 199.9999999999999716, -9.233471789954972309, -16.61280101608961246 ) ) ;
#5127 = CARTESIAN_POINT ( 'NONE',  ( -87.02160542365453466, 10.86122935277673918, 18.50851042352477194 ) ) ;
#5128 = CARTESIAN_POINT ( 'NONE',  ( -62.79433447039818361, -11.74096317475005691, -24.94280497470819569 ) ) ;
#5129 = CARTESIAN_POINT ( 'NONE',  ( 91.82158438592158234, 12.16597498397756993, 12.16597498397776356 ) ) ;
#5130 = CARTESIAN_POINT ( 'NONE',  ( -77.55640685876517182, -16.63820247459988622, -14.66025286086431478 ) ) ;
#5131 = CARTESIAN_POINT ( 'NONE',  ( -105.3755690713226585, -39.99999999999985079, -18.24025645688394448 ) ) ;
#5132 = DIRECTION ( 'NONE',  ( 0.000000000000000000, 1.000000000000000000, 0.000000000000000000 ) ) ;
#5133 = CARTESIAN_POINT ( 'NONE',  ( -56.48582580120559982, 9.153146818113574668, -40.00000000000002132 ) ) ;
#5134 = CARTESIAN_POINT ( 'NONE',  ( 14.38125909742182529, -39.01709431150933938, 39.01709431150894147 ) ) ;
#5135 = CARTESIAN_POINT ( 'NONE',  ( -213.1075012329537230, -53.71589010953668719, -40.00000000000002132 ) ) ;
#5137 = CARTESIAN_POINT ( 'NONE',  ( -100.7734535825088500, 40.00000000000008527, -22.67402823373177512 ) ) ;
#5136 = CARTESIAN_POINT ( 'NONE',  ( -86.96347745069644475, -43.67073346367964604, -12.89780903124457545 ) ) ;
#5138 = CARTESIAN_POINT ( 'NONE',  ( -238.4067589809705794, 0.9644942799825386714, 0.000000000000000000 ) ) ;
#5139 = CARTESIAN_POINT ( 'NONE',  ( 146.6084372240433993, 3.800685668858676980, 3.800685668858667210 ) ) ;
#5140 = CARTESIAN_POINT ( 'NONE',  ( -105.3755690713226585, 18.24025645688350750, -40.00000000000002132 ) ) ;
#5141 = ORIENTED_EDGE ( 'NONE', *, *, #22568, .T. ) ;
#5142 = CARTESIAN_POINT ( 'NONE',  ( 5.823571940226716315, -44.77584346942416715, 24.75780943188591010 ) ) ;
#5143 =( BOUNDED_SURFACE ( )  B_SPLINE_SURFACE ( 3, 3, ( 
 ( #12120, #23824, #7719, #9861, #12254, #3887, #1622, #5870, #7986, #14243, #24236, #24095, #22110, #20245, #2025, #17831, #6009, #9729, #15970, #16243, #25844, #17700, #13713, #19971, #15829, #21838, #9595, #10127, #7588, #13839 ),
 ( #22245, #5734, #23959, #16104, #18228, #15, #8126, #17963, #6135, #22383, #15700, #3607, #11717, #19836, #25978, #10261, #24769, #4551, #4678, #18903, #554, #8387, #12648, #24506, #2412, #24634, #6266, #16640, #6392, #12379 ),
 ( #20773, #14508, #4414, #20908, #14379, #2543, #22512, #16903, #10661, #18770, #22639, #4290, #20507, #16509, #16766, #4815, #8791, #6788, #12508, #20376, #150, #2279, #16372, #418, #10388, #18371, #10793, #18499, #2686, #280 ),
 ( #8522, #8254, #22900, #25035, #20636, #10521, #18635, #6522, #12781, #14900, #14633, #22770, #23040, #2151, #8658, #24900, #6655, #682, #14770, #13644, #17032, #9793, #21770, #11643, #7051, #25167, #13050, #947, #9661, #24024 ),
 ( #10926, #15762, #15035, #11172, #25424, #23293, #25907, #1689, #8922, #12917, #7524, #19287, #816, #1556, #3543, #21296, #23757, #19765, #5538, #11785, #15168, #19905, #26044, #1070, #2817, #6918, #23891, #17765, #7648, #21034 ),
 ( #11051, #19037, #17896, #9179, #17290, #5069, #15632, #23165, #13175, #5667, #13773, #3070, #21900, #3677, #4944, #7781, #15897, #21168, #19162, #2941, #9055, #17160, #25294, #1822, #18030, #16037, #26180, #9924, #7920, #5803 ),
 ( #13910, #22045, #3818, #11921, #20043, #10650, #17151, #12636, #25026, #4669, #12908, #23156, #1062, #15281, #6779, #14891, #9046, #8781, #672, #2933, #10917, #25158, #21159, #18893, #13166, #10781, #23031, #8648, #9168, #4539 ) ),
 .UNSPECIFIED., .T., .F., .F. ) 
 B_SPLINE_SURFACE_WITH_KNOTS ( ( 4, 3, 4 ),
 ( 4, 2, 2, 2, 2, 2, 2, 2, 2, 2, 2, 2, 2, 2, 4 ),
 ( 0.000000000000000000, 0.5000000000000000000, 1.000000000000000000 ),
 ( 0.000000000000000000, 0.1357259735107005372, 0.1651108541090157700, 0.1944957347073310028, 0.3598804999793158710, 0.3867117631979620773, 0.4135430264166082281, 0.5789277916885930964, 0.6062785021374117456, 0.6336292125862302838, 0.8508620842112317728, 0.8814014469398914198, 0.9119408096685510667, 0.9559704048342755334, 1.000000000000000000 ),
 .UNSPECIFIED. ) 
 GEOMETRIC_REPRESENTATION_ITEM ( )  RATIONAL_B_SPLINE_SURFACE ( (
 ( 1.000000000000000000, 1.000000000000000000, 1.000000000000000000, 1.000000000000000000, 1.000000000000000000, 1.000000000000000000, 1.000000000000000000, 1.000000000000000000, 1.000000000000000000, 1.000000000000000000, 1.000000000000000000, 1.000000000000000000, 1.000000000000000000, 1.000000000000000000, 1.000000000000000000, 1.000000000000000000, 1.000000000000000000, 1.000000000000000000, 1.000000000000000000, 1.000000000000000000, 1.000000000000000000, 1.000000000000000000, 1.000000000000000000, 1.000000000000000000, 1.000000000000000000, 1.000000000000000000, 1.000000000000000000, 1.000000000000000000, 1.000000000000000000, 1.000000000000000000),
 ( 0.3333333333333333703, 0.3333333333333333703, 0.3333333333333333703, 0.3333333333333333703, 0.3333333333333333703, 0.3333333333333333703, 0.3333333333333333703, 0.3333333333333333703, 0.3333333333333333703, 0.3333333333333333703, 0.3333333333333333703, 0.3333333333333333703, 0.3333333333333333703, 0.3333333333333333703, 0.3333333333333333703, 0.3333333333333333703, 0.3333333333333333703, 0.3333333333333333703, 0.3333333333333333703, 0.3333333333333333703, 0.3333333333333333703, 0.3333333333333333703, 0.3333333333333333703, 0.3333333333333333703, 0.3333333333333333703, 0.3333333333333333703, 0.3333333333333333703, 0.3333333333333333703, 0.3333333333333333703, 0.3333333333333333703),
 ( 0.3333333333333333703, 0.3333333333333333703, 0.3333333333333333703, 0.3333333333333333703, 0.3333333333333333703, 0.3333333333333333703, 0.3333333333333333703, 0.3333333333333333703, 0.3333333333333333703, 0.3333333333333333703, 0.3333333333333333703, 0.3333333333333333703, 0.3333333333333333703, 0.3333333333333333703, 0.3333333333333333703, 0.3333333333333333703, 0.3333333333333333703, 0.3333333333333333703, 0.3333333333333333703, 0.3333333333333333703, 0.3333333333333333703, 0.3333333333333333703, 0.3333333333333333703, 0.3333333333333333703, 0.3333333333333333703, 0.3333333333333333703, 0.3333333333333333703, 0.3333333333333333703, 0.3333333333333333703, 0.3333333333333333703),
 ( 1.000000000000000000, 1.000000000000000000, 1.000000000000000000, 1.000000000000000000, 1.000000000000000000, 1.000000000000000000, 1.000000000000000000, 1.000000000000000000, 1.000000000000000000, 1.000000000000000000, 1.000000000000000000, 1.000000000000000000, 1.000000000000000000, 1.000000000000000000, 1.000000000000000000, 1.000000000000000000, 1.000000000000000000, 1.000000000000000000, 1.000000000000000000, 1.000000000000000000, 1.000000000000000000, 1.000000000000000000, 1.000000000000000000, 1.000000000000000000, 1.000000000000000000, 1.000000000000000000, 1.000000000000000000, 1.000000000000000000, 1.000000000000000000, 1.000000000000000000),
 ( 0.3333333333333333703, 0.3333333333333333703, 0.3333333333333333703, 0.3333333333333333703, 0.3333333333333333703, 0.3333333333333333703, 0.3333333333333333703, 0.3333333333333333703, 0.3333333333333333703, 0.3333333333333333703, 0.3333333333333333703, 0.3333333333333333703, 0.3333333333333333703, 0.3333333333333333703, 0.3333333333333333703, 0.3333333333333333703, 0.3333333333333333703, 0.3333333333333333703, 0.3333333333333333703, 0.3333333333333333703, 0.3333333333333333703, 0.3333333333333333703, 0.3333333333333333703, 0.3333333333333333703, 0.3333333333333333703, 0.3333333333333333703, 0.3333333333333333703, 0.3333333333333333703, 0.3333333333333333703, 0.3333333333333333703),
 ( 0.3333333333333333703, 0.3333333333333333703, 0.3333333333333333703, 0.3333333333333333703, 0.3333333333333333703, 0.3333333333333333703, 0.3333333333333333703, 0.3333333333333333703, 0.3333333333333333703, 0.3333333333333333703, 0.3333333333333333703, 0.3333333333333333703, 0.3333333333333333703, 0.3333333333333333703, 0.3333333333333333703, 0.3333333333333333703, 0.3333333333333333703, 0.3333333333333333703, 0.3333333333333333703, 0.3333333333333333703, 0.3333333333333333703, 0.3333333333333333703, 0.3333333333333333703, 0.3333333333333333703, 0.3333333333333333703, 0.3333333333333333703, 0.3333333333333333703, 0.3333333333333333703, 0.3333333333333333703, 0.3333333333333333703),
 ( 1.000000000000000000, 1.000000000000000000, 1.000000000000000000, 1.000000000000000000, 1.000000000000000000, 1.000000000000000000, 1.000000000000000000, 1.000000000000000000, 1.000000000000000000, 1.000000000000000000, 1.000000000000000000, 1.000000000000000000, 1.000000000000000000, 1.000000000000000000, 1.000000000000000000, 1.000000000000000000, 1.000000000000000000, 1.000000000000000000, 1.000000000000000000, 1.000000000000000000, 1.000000000000000000, 1.000000000000000000, 1.000000000000000000, 1.000000000000000000, 1.000000000000000000, 1.000000000000000000, 1.000000000000000000, 1.000000000000000000, 1.000000000000000000, 1.000000000000000000) ) ) 
 REPRESENTATION_ITEM ( '' )  SURFACE ( )  );
#5144 = CARTESIAN_POINT ( 'NONE',  ( -87.12803293485012546, -14.20621343981222928, 16.13817828097420204 ) ) ;
#5145 = CARTESIAN_POINT ( 'NONE',  ( 57.59792236341147031, -1.722363176415123043, 54.84617931850879557 ) ) ;
#5146 = CARTESIAN_POINT ( 'NONE',  ( -198.0356074513804572, -40.00000000000011369, 15.37879056873056527 ) ) ;
#5147 = FACE_OUTER_BOUND ( 'NONE', #10997, .T. ) ;
#5148 = CIRCLE ( 'NONE', #2190, 20.53474504356812247 ) ;
#5149 = CARTESIAN_POINT ( 'NONE',  ( 8.517493190815727644, -14.17913040910352329, -49.32792454093244316 ) ) ;
#5150 = CARTESIAN_POINT ( 'NONE',  ( 199.9999999999997726, -5.383989893674753446, 18.23209102328170061 ) ) ;
#5151 = CARTESIAN_POINT ( 'NONE',  ( -651.1759909824590977, 35.84781451397984853, -17.76753621510863468 ) ) ;
#5152 = CARTESIAN_POINT ( 'NONE',  ( 170.0000000000000284, -22.62041470344884431, 9.369682556672202622 ) ) ;
#5153 = CARTESIAN_POINT ( 'NONE',  ( 19.06497207195979726, 38.31983398719604139, 18.24870850772803976 ) ) ;
#5154 = CARTESIAN_POINT ( 'NONE',  ( -213.1075012329537230, -9.698598906462304825, -66.26714140138675191 ) ) ;
#5155 = CARTESIAN_POINT ( 'NONE',  ( 192.4448373802101173, 42.42640687122070631, 14.14213562370331623 ) ) ;
#5156 = CARTESIAN_POINT ( 'NONE',  ( 192.4448373802100889, -14.14213562375896061, 14.14213562375865330 ) ) ;
#5157 = CARTESIAN_POINT ( 'NONE',  ( -162.0762913951021176, 27.08623940707639477, -29.48230308784743059 ) ) ;
#5159 = CARTESIAN_POINT ( 'NONE',  ( 200.0000000000000000, -14.14213562373046784, -42.42640687119298804 ) ) ;
#5158 = CARTESIAN_POINT ( 'NONE',  ( -213.1075012329537230, -9.698598906462304825, -66.26714140138675191 ) ) ;
#5160 = CARTESIAN_POINT ( 'NONE',  ( 0.2972598230769959993, 38.42060263243713081, -38.42060263243619289 ) ) ;
#5161 = CARTESIAN_POINT ( 'NONE',  ( 0.2972598230769930017, 14.33493731733933352, -40.00000000000002132 ) ) ;
#5162 = FACE_OUTER_BOUND ( 'NONE', #11393, .T. ) ;
#5163 = CARTESIAN_POINT ( 'NONE',  ( -726.9846540392142060, 0.000000000000000000, 0.000000000000000000 ) ) ;
#5164 = CARTESIAN_POINT ( 'NONE',  ( -100.7734535825088500, -12.25131212657524316, 44.31723036834888774 ) ) ;
#5165 = AXIS2_PLACEMENT_3D ( 'NONE', #9690, #7952, #17796 ) ;
#5166 = CARTESIAN_POINT ( 'NONE',  ( -188.2506440019725176, 46.97351617221541176, -13.82466072834929705 ) ) ;
#5167 = ORIENTED_EDGE ( 'NONE', *, *, #5029, .T. ) ;
#5168 = CARTESIAN_POINT ( 'NONE',  ( 146.6084372240433709, 32.08495691632064961, -24.48358557860320417 ) ) ;
#5169 = AXIS2_PLACEMENT_3D ( 'NONE', #10548, #21194, #9079 ) ;
#5170 = CARTESIAN_POINT ( 'NONE',  ( -88.39148973765153983, -20.15708830332398804, -8.027153355909376842 ) ) ;
#5171 = CARTESIAN_POINT ( 'NONE',  ( 19.94008347562303030, 24.01421467034686330, 43.76810615267632443 ) ) ;
#5172 = CARTESIAN_POINT ( 'NONE',  ( -3.564770973659422193, -43.27160733161171891, -17.92368662243730171 ) ) ;
#5173 = EDGE_LOOP ( 'NONE', ( #4427, #16912, #8399, #22391 ) ) ;
#5174 = CARTESIAN_POINT ( 'NONE',  ( -187.3036811847832723, -42.71162014090015191, 23.25512365538946469 ) ) ;
#5175 = ADVANCED_FACE ( 'NONE', ( #20701 ), #562, .T. ) ;
#5176 = CARTESIAN_POINT ( 'NONE',  ( 199.9999999999998863, -4.016713260438497635, -18.57371263647062420 ) ) ;
#5177 = CARTESIAN_POINT ( 'NONE',  ( 23.32574057153296110, -13.80366151303459077, 46.82643129194502762 ) ) ;
#5178 = CARTESIAN_POINT ( 'NONE',  ( 48.46027422360368320, 35.02097763790654739, -18.19770396007656643 ) ) ;
#5179 = CARTESIAN_POINT ( 'NONE',  ( 199.0068072339493597, 19.36029496603142874, -5.002335373038918398 ) ) ;
#5180 = AXIS2_PLACEMENT_3D ( 'NONE', #15679, #23804, #23309 ) ;
#5181 = CARTESIAN_POINT ( 'NONE',  ( 128.5824617753800680, -28.96492468983284496, 11.99766463964388663 ) ) ;
#5182 = CARTESIAN_POINT ( 'NONE',  ( -100.7734535825088358, 6.065416334915073333E-14, -22.67402823373191723 ) ) ;
#5183 = CARTESIAN_POINT ( 'NONE',  ( 91.82158438592158234, 7.693928927950222250E-14, -17.20528682183300262 ) ) ;
#5184 =( BOUNDED_SURFACE ( )  B_SPLINE_SURFACE ( 3, 2, ( 
 ( #12598, #10606, #11502 ),
 ( #19626, #21756, #23877 ),
 ( #3529, #19248, #7133 ),
 ( #15749, #19752, #9263 ),
 ( #25381, #5272, #5653 ),
 ( #13377, #1159, #11630 ),
 ( #7381, #1411, #17370 ),
 ( #15492, #11133, #5524 ),
 ( #15246, #9512, #23377 ),
 ( #23622, #1029, #5402 ),
 ( #21624, #19495, #17494 ),
 ( #9128, #25508, #17617 ),
 ( #25635, #3276, #9387 ),
 ( #25762, #7257, #15375 ),
 ( #17752, #19372, #13759 ),
 ( #1542, #13631, #11374 ) ),
 .UNSPECIFIED., .F., .F., .F. ) 
 B_SPLINE_SURFACE_WITH_KNOTS ( ( 4, 2, 2, 2, 2, 2, 2, 4 ),
 ( 3, 3 ),
 ( 0.04143342415447111293, 0.04844559399083352147, 0.05195167890901472574, 0.05545776382719592307, 0.06246993366355832467, 0.06422297612264893374, 0.06597601858173952893, 0.06948210349992073320 ),
 ( 0.000000000000000000, 1.000000000000000000 ),
 .UNSPECIFIED. ) 
 GEOMETRIC_REPRESENTATION_ITEM ( )  RATIONAL_B_SPLINE_SURFACE ( (
 ( 1.000000000000000000, 0.9541700779530459808, 1.000000000000000000),
 ( 1.000000000000000000, 0.9520168980288470362, 1.000000000000000000),
 ( 1.000000000000000000, 0.9503263051615414847, 1.000000000000000000),
 ( 1.000000000000000000, 0.9485964699089932672, 1.000000000000000000),
 ( 1.000000000000000000, 0.9481599523395594087, 1.000000000000000000),
 ( 1.000000000000000000, 0.9475783919172264813, 1.000000000000000000),
 ( 1.000000000000000000, 0.9474332805893206366, 1.000000000000000000),
 ( 1.000000000000000000, 0.9474385816627715062, 1.000000000000000000),
 ( 1.000000000000000000, 0.9480200071115888472, 1.000000000000000000),
 ( 1.000000000000000000, 0.9494436219492867757, 1.000000000000000000),
 ( 1.000000000000000000, 0.9497633688930613438, 1.000000000000000000),
 ( 1.000000000000000000, 0.9504729676350489598, 1.000000000000000000),
 ( 1.000000000000000000, 0.9508638236297636270, 1.000000000000000000),
 ( 1.000000000000000000, 0.9521268919818258736, 1.000000000000000000),
 ( 1.000000000000000000, 0.9530924015899429058, 1.000000000000000000),
 ( 1.000000000000000000, 0.9541700779530460919, 1.000000000000000000) ) ) 
 REPRESENTATION_ITEM ( '' )  SURFACE ( )  );
#5185 = DIRECTION ( 'NONE',  ( 1.000000000000000000, 1.836970198721030427E-16, -0.000000000000000000 ) ) ;
#5186 = CARTESIAN_POINT ( 'NONE',  ( -91.56559293963834989, -17.32597176626812896, -2.449293598294708485E-15 ) ) ;
#5188 = CARTESIAN_POINT ( 'NONE',  ( 170.0000000000000000, 30.00000000000007105, 0.000000000000000000 ) ) ;
#5187 = CARTESIAN_POINT ( 'NONE',  ( 25.05785482536186137, -17.61697374403291505, -42.53113694077947571 ) ) ;
#5189 = CARTESIAN_POINT ( 'NONE',  ( -208.1127848780265026, -15.00245453012673202, 0.000000000000000000 ) ) ;
#5190 = CARTESIAN_POINT ( 'NONE',  ( 136.1360204305621266, 24.77266263493138965, -24.77266263493110188 ) ) ;
#5191 = CARTESIAN_POINT ( 'NONE',  ( 151.7948205124836534, 39.99999999999970157, 33.23291073765595627 ) ) ;
#5192 = CARTESIAN_POINT ( 'NONE',  ( -100.7734535825088500, -39.99999999999986500, -17.32597176626853397 ) ) ;
#5193 = CYLINDRICAL_SURFACE ( 'NONE', #10940, 5.000000000000004441 ) ;
#5194 = ORIENTED_EDGE ( 'NONE', *, *, #15462, .T. ) ;
#5196 = CARTESIAN_POINT ( 'NONE',  ( 11.28112952480928755, 44.87390167243371053, -18.58737866929334359 ) ) ;
#5195 = DIRECTION ( 'NONE',  ( 1.000000000000000000, 0.000000000000000000, 0.000000000000000000 ) ) ;
#5197 = CARTESIAN_POINT ( 'NONE',  ( 146.6084372240433709, -5.374981219216948602, 40.00000000000002132 ) ) ;
#5198 =( NAMED_UNIT ( * ) SI_UNIT ( $, .STERADIAN. ) SOLID_ANGLE_UNIT ( ) );
#5199 = CARTESIAN_POINT ( 'NONE',  ( -194.7885354600941525, 44.44047100927782878, -18.40784581029470957 ) ) ;
#5200 = ORIENTED_EDGE ( 'NONE', *, *, #7342, .F. ) ;
#5201 = EDGE_LOOP ( 'NONE', ( #20211, #11684, #5915, #4160 ) ) ;
#5202 = CIRCLE ( 'NONE', #23470, 20.53474504356812247 ) ;
#5203 = CARTESIAN_POINT ( 'NONE',  ( 136.1360204305621266, 24.77266263493138965, -24.77266263493110188 ) ) ;
#5204 = DIRECTION ( 'NONE',  ( 0.000000000000000000, 0.000000000000000000, 1.000000000000000000 ) ) ;
#5205 = ORIENTED_EDGE ( 'NONE', *, *, #15010, .T. ) ;
#5206 = VERTEX_POINT ( 'NONE', #8690 ) ;
#5207 = CARTESIAN_POINT ( 'NONE',  ( 199.0263095778509808, -15.67393427090936875, 12.43211889955359162 ) ) ;
#5208 = CARTESIAN_POINT ( 'NONE',  ( -114.4364955367327070, 8.644468109209567430, -20.04994829327642947 ) ) ;
#5209 = CARTESIAN_POINT ( 'NONE',  ( 170.2234770963711128, 10.92277846919201068, 10.92277846919202133 ) ) ;
#5210 = CARTESIAN_POINT ( 'NONE',  ( -114.4364955367319965, -20.29001642039104070, -8.064892380835031460 ) ) ;
#5211 = CARTESIAN_POINT ( 'NONE',  ( -56.48582580120559271, 2.158176344243877536E-14, -9.153146818113587102 ) ) ;
#5212 = CARTESIAN_POINT ( 'NONE',  ( -265.0000000000000000, -4.867971026610730343E-14, -6.532754371361504014E-30 ) ) ;
#5213 = FACE_OUTER_BOUND ( 'NONE', #5173, .T. ) ;
#5214 = CARTESIAN_POINT ( 'NONE',  ( 0.2972598230770103767, -39.99999999999945288, -54.33493731733979359 ) ) ;
#5215 = CARTESIAN_POINT ( 'NONE',  ( 19.06497207195981858, 5.735870351258996432E-13, -54.19242893257843008 ) ) ;
#5216 = CARTESIAN_POINT ( 'NONE',  ( -77.71409353909379547, 19.10608670630663397, 10.98878756468862861 ) ) ;
#5217 = CARTESIAN_POINT ( 'NONE',  ( -192.9588430854690273, -66.79921049724377724, 10.23066800231950069 ) ) ;
#5218 = CARTESIAN_POINT ( 'NONE',  ( 19.06497207195981147, -4.605042221739098431E-14, 14.19242893257840521 ) ) ;
#5219 = CARTESIAN_POINT ( 'NONE',  ( -56.48582580120559271, 6.472252184284211118, -6.472252184284153387 ) ) ;
#5220 = CARTESIAN_POINT ( 'NONE',  ( 133.2080217031554810, 29.90338805389109211, 12.38638889282741573 ) ) ;
#5221 = DIRECTION ( 'NONE',  ( 0.000000000000000000, -1.000000000000000000, 0.000000000000000000 ) ) ;
#5222 = CARTESIAN_POINT ( 'NONE',  ( -210.0000000000000284, 57.47694228411666728, -64.52066607436458412 ) ) ;
#5223 = CARTESIAN_POINT ( 'NONE',  ( -82.23729782350187634, -15.18297044030989440, 13.37626936638599950 ) ) ;
#5224 = CARTESIAN_POINT ( 'NONE',  ( -30.26275506840323715, 29.48230279907789253, 29.48230279907799556 ) ) ;
#5225 = CARTESIAN_POINT ( 'NONE',  ( 0.2972598230770027716, -38.42060263243681817, 18.14793986248684377 ) ) ;
#5226 = CARTESIAN_POINT ( 'NONE',  ( -114.4364955367321102, -8.064892380842767494, -20.29001642038801734 ) ) ;
#5227 = CARTESIAN_POINT ( 'NONE',  ( -93.12335834970892279, 16.03295912088692177, 16.03295912088721664 ) ) ;
#5228 = ORIENTED_EDGE ( 'NONE', *, *, #21220, .F. ) ;
#5229 = CARTESIAN_POINT ( 'NONE',  ( 146.6084372240433709, 32.08495691632030145, 24.48358557860365181 ) ) ;
#5230 = CARTESIAN_POINT ( 'NONE',  ( 192.4448373802100889, 20.00000000003945644, 0.000000000000000000 ) ) ;
#5231 = DIRECTION ( 'NONE',  ( 1.000000000000000000, 1.836970198721030181E-16, 0.000000000000000000 ) ) ;
#5232 = VERTEX_POINT ( 'NONE', #7203 ) ;
#5233 = DIRECTION ( 'NONE',  ( 0.9352143323240564854, -0.1355013636652032116, 0.3271292299085176158 ) ) ;
#5234 = CARTESIAN_POINT ( 'NONE',  ( 199.0199679947243112, -18.47654620739217890, -7.661348058496780133 ) ) ;
#5235 = CARTESIAN_POINT ( 'NONE',  ( -200.0000000000001421, -14.17215463606902404, -49.28189405767602693 ) ) ;
#5236 = ORIENTED_EDGE ( 'NONE', *, *, #11202, .T. ) ;
#5237 = ORIENTED_EDGE ( 'NONE', *, *, #15083, .T. ) ;
#5238 = CARTESIAN_POINT ( 'NONE',  ( 136.1360204305621266, 24.77266263493138965, -24.77266263493110188 ) ) ;
#5239 = CARTESIAN_POINT ( 'NONE',  ( -105.3755690713226585, 40.00000000000007816, -21.75974354311636461 ) ) ;
#5240 = CARTESIAN_POINT ( 'NONE',  ( -97.73860346104240193, -20.89580782304671658, -8.185503821051291595 ) ) ;
#5241 = EDGE_CURVE ( 'NONE', #9554, #24441, #12998, .T. ) ;
#5242 = FACE_OUTER_BOUND ( 'NONE', #22253, .T. ) ;
#5243 = CARTESIAN_POINT ( 'NONE',  ( -135.8532207217289738, -40.00000000000001421, -9.153146818113709671 ) ) ;
#5244 = CARTESIAN_POINT ( 'NONE',  ( 199.9999999999998863, -9.504749071264818383, -16.45922038047892144 ) ) ;
#5245 = EDGE_CURVE ( 'NONE', #11726, #6963, #15001, .T. ) ;
#5246 = CARTESIAN_POINT ( 'NONE',  ( -77.55640685878515228, 14.66973228108125582, 16.62872305437120701 ) ) ;
#5247 = CARTESIAN_POINT ( 'NONE',  ( -6.342283169552904276, -23.00001740814894546, -42.32555349774978737 ) ) ;
#5248 = CARTESIAN_POINT ( 'NONE',  ( -198.0356074513804572, -10.87444709758429262, -67.44298959250878056 ) ) ;
#5249 = LINE ( 'NONE', #11745, #15248 ) ;
#5250 = CARTESIAN_POINT ( 'NONE',  ( -213.1075012329537230, -39.99999999999948841, -53.71589010950208376 ) ) ;
#5251 = FACE_OUTER_BOUND ( 'NONE', #6274, .T. ) ;
#5252 = CARTESIAN_POINT ( 'NONE',  ( 200.0000000000000000, 20.00000000000013856, 40.00000000000002132 ) ) ;
#5253 = CARTESIAN_POINT ( 'NONE',  ( -162.0762913951020892, -41.69427287672991866, -40.00000000000002132 ) ) ;
#5254 = EDGE_CURVE ( 'NONE', #19106, #9028, #7453, .T. ) ;
#5255 = EDGE_CURVE ( 'NONE', #5806, #122, #9587, .T. ) ;
#5256 = CARTESIAN_POINT ( 'NONE',  ( 57.59792236341148453, 1.722363176414758668, 54.84617931850880268 ) ) ;
#5257 = CARTESIAN_POINT ( 'NONE',  ( -259.2033419157646676, 9.517827891722582478, -40.00000000000002132 ) ) ;
#5259 = CARTESIAN_POINT ( 'NONE',  ( 4.995406935893283773, 39.99999999999997158, 15.24977328854846803 ) ) ;
#5258 = CARTESIAN_POINT ( 'NONE',  ( -114.4008516218694496, 20.18474087537135730, 8.248277354728019262 ) ) ;
#5260 = CARTESIAN_POINT ( 'NONE',  ( -114.6170081391615838, 21.23870042814614933, 5.725526104550264783 ) ) ;
#5261 = CARTESIAN_POINT ( 'NONE',  ( 151.7948205124836534, -23.49921654116027980, 33.06932595376354556 ) ) ;
#5262 = CARTESIAN_POINT ( 'NONE',  ( -135.8532207217289738, 30.84685318188643777, -40.00000000000002132 ) ) ;
#5263 = ORIENTED_EDGE ( 'NONE', *, *, #25351, .T. ) ;
#5264 = CARTESIAN_POINT ( 'NONE',  ( 22.66553228237864204, -43.20407469282417168, 17.89571368754787528 ) ) ;
#5265 = CARTESIAN_POINT ( 'NONE',  ( -105.2502153031277601, 17.39736479739449138, -12.58638139385909760 ) ) ;
#5266 = CARTESIAN_POINT ( 'NONE',  ( -100.7734535825088358, 12.25131212657480440, 12.25131212657487012 ) ) ;
#5267 = CARTESIAN_POINT ( 'NONE',  ( 14.38125909742181108, -5.035366881890652543E-14, 15.17850393972633682 ) ) ;
#5268 = CARTESIAN_POINT ( 'NONE',  ( -77.65265458751275673, 21.61050232527882287, -4.374419871749616107 ) ) ;
#5269 = CARTESIAN_POINT ( 'NONE',  ( 1.564252679174726213, -14.06374044400928724, -48.56509332159251358 ) ) ;
#5270 = CARTESIAN_POINT ( 'NONE',  ( 199.9999999999999147, -8.688421465551046552, 16.91138275242808575 ) ) ;
#5271 = CARTESIAN_POINT ( 'NONE',  ( -87.13361725323537144, -21.49321519332493580, -1.359587258213210248 ) ) ;
#5272 = CARTESIAN_POINT ( 'NONE',  ( -82.24432634617156168, 2.528896859437274269, -20.04338201863724578 ) ) ;
#5273 = CARTESIAN_POINT ( 'NONE',  ( -259.2033419157646676, -6.730120644403663199, 6.730120644403451813 ) ) ;
#5274 = CARTESIAN_POINT ( 'NONE',  ( -198.0356074513804572, -10.87444709758429262, -67.44298959250878056 ) ) ;
#5275 = CARTESIAN_POINT ( 'NONE',  ( -56.48582580120559982, 34.75652343174597547, 21.81201906317791384 ) ) ;
#5276 = CARTESIAN_POINT ( 'NONE',  ( 199.9999999999999432, -14.14213562373115884, 14.14213562373085153 ) ) ;
#5277 = CARTESIAN_POINT ( 'NONE',  ( -135.8532207217289738, 6.472252184284583265, -50.09629031063960980 ) ) ;
#5279 = CARTESIAN_POINT ( 'NONE',  ( 57.59792236341147031, -1.722363176414363206, -54.84617931850881689 ) ) ;
#5278 = CARTESIAN_POINT ( 'NONE',  ( 184.8905102610680444, 14.79361573936424890, -41.77492675555986068 ) ) ;
#5280 = CARTESIAN_POINT ( 'NONE',  ( 4.995406935893290878, 39.06748935135239265, -39.06748935135144762 ) ) ;
#5281 = CARTESIAN_POINT ( 'NONE',  ( -105.2054292635175585, -15.19799821370250825, 15.19799821370211923 ) ) ;
#5282 = CARTESIAN_POINT ( 'NONE',  ( 130.8568914410475372, -24.07718906447222551, -24.07718906447233209 ) ) ;
#5283 = LINE ( 'NONE', #19507, #23365 ) ;
#5284 = CARTESIAN_POINT ( 'NONE',  ( 170.2234770963711128, -10.92277846919235529, 45.64576402573175073 ) ) ;
#5285 = CARTESIAN_POINT ( 'NONE',  ( -192.9588430854690273, 54.46834944101718889, 40.00000000000002132 ) ) ;
#5286 = ORIENTED_EDGE ( 'NONE', *, *, #2014, .T. ) ;
#5287 = CARTESIAN_POINT ( 'NONE',  ( -135.8532207217289738, 21.81201906317777883, -34.75652343174605363 ) ) ;
#5288 = CARTESIAN_POINT ( 'NONE',  ( -82.24286360236595783, -15.97561011111183049, -12.41695498259727692 ) ) ;
#5289 = CARTESIAN_POINT ( 'NONE',  ( 25.62979979009272924, 22.88075396655783322, 42.16299361905724652 ) ) ;
#5290 = CARTESIAN_POINT ( 'NONE',  ( -8.255580677151938218, -41.75907689858397731, -22.62611236873543774 ) ) ;
#5291 = ORIENTED_EDGE ( 'NONE', *, *, #15160, .T. ) ;
#5292 = CARTESIAN_POINT ( 'NONE',  ( -183.1090696431200229, -45.18841929385192202, 13.45963186438693704 ) ) ;
#5293 = CARTESIAN_POINT ( 'NONE',  ( 199.9999999999999147, -15.17855064416508526, -11.43956010876637563 ) ) ;
#5294 = CARTESIAN_POINT ( 'NONE',  ( 37.37129771735379080, -20.48130208310442413, 38.51719860173601262 ) ) ;
#5295 = DIRECTION ( 'NONE',  ( 1.000000000000000000, -0.000000000000000000, -0.000000000000000000 ) ) ;
#5296 = CARTESIAN_POINT ( 'NONE',  ( 199.0054082256929746, 12.16974446990029790, -15.87805152391047159 ) ) ;
#5297 = DIRECTION ( 'NONE',  ( 0.000000000000000000, 0.000000000000000000, 1.000000000000000000 ) ) ;
#5298 = CARTESIAN_POINT ( 'NONE',  ( -91.56559293963836410, 40.00000000000008527, -22.67402823373177867 ) ) ;
#5299 = CARTESIAN_POINT ( 'NONE',  ( -82.26522640325165980, -5.034412314778461628, 19.58751121911369708 ) ) ;
#5300 = CARTESIAN_POINT ( 'NONE',  ( 200.0000000000000000, -71.50000000000002842, -66.50000000000005684 ) ) ;
#5301 = CARTESIAN_POINT ( 'NONE',  ( 146.6084372240433709, -5.374981219216948602, 40.00000000000002132 ) ) ;
#5303 = DIRECTION ( 'NONE',  ( 0.000000000000000000, 0.000000000000000000, 1.000000000000000000 ) ) ;
#5302 = CARTESIAN_POINT ( 'NONE',  ( 36.66494225458649225, -16.22659705900232652, -39.17447069114147951 ) ) ;
#5304 = CARTESIAN_POINT ( 'NONE',  ( 57.59792236341147031, 2.435789363418170872, 40.00000000000002132 ) ) ;
#5305 = CARTESIAN_POINT ( 'NONE',  ( 14.38125909742181285, -10.73282306404727393, 10.73282306404716380 ) ) ;
#5306 = CARTESIAN_POINT ( 'NONE',  ( -238.4067589809705794, 40.00000000000040501, -40.96449427990138759 ) ) ;
#5307 = CARTESIAN_POINT ( 'NONE',  ( -30.26275506840323359, -39.99999999999959499, -41.69427246844670520 ) ) ;
#5308 = EDGE_CURVE ( 'NONE', #12893, #2033, #4231, .T. ) ;
#5309 = CARTESIAN_POINT ( 'NONE',  ( 104.1674819957097355, -20.61915445364400412, -8.540733419364878287 ) ) ;
#5310 = ORIENTED_EDGE ( 'NONE', *, *, #22980, .F. ) ;
#5312 = CARTESIAN_POINT ( 'NONE',  ( -4.082462733454346626, 46.97557262069204853, -13.82507958736555231 ) ) ;
#5311 = FACE_BOUND ( 'NONE', #11458, .T. ) ;
#5313 = CARTESIAN_POINT ( 'NONE',  ( -198.0356074513804572, -55.37879056874826489, 40.00000000000002132 ) ) ;
#5314 = CARTESIAN_POINT ( 'NONE',  ( -213.1075012329537230, 9.698598906450543566, -9.698598906450348167 ) ) ;
#5315 = CARTESIAN_POINT ( 'NONE',  ( -197.4154352060510575, 44.73190714601614815, -24.72550168627246592 ) ) ;
#5316 = DIRECTION ( 'NONE',  ( 1.282749433769087757E-30, -6.982962677686266711E-15, -1.000000000000000000 ) ) ;
#5317 = AXIS2_PLACEMENT_3D ( 'NONE', #6691, #4584, #21071 ) ;
#5318 = VERTEX_POINT ( 'NONE', #25324 ) ;
#5319 = ORIENTED_EDGE ( 'NONE', *, *, #16953, .F. ) ;
#5320 = CARTESIAN_POINT ( 'NONE',  ( -200.0000000000000000, 61.50000000000009948, 66.50000000000005684 ) ) ;
#5321 = CARTESIAN_POINT ( 'NONE',  ( 154.0339099654740949, 11.67508747798894753, -28.18615453125283210 ) ) ;
#5322 = CARTESIAN_POINT ( 'NONE',  ( 107.5473083967345076, 1.035215841339324533E-13, -23.99138244111055585 ) ) ;
#5323 = ORIENTED_EDGE ( 'NONE', *, *, #14014, .T. ) ;
#5324 = CARTESIAN_POINT ( 'NONE',  ( 199.0263356842403653, -15.36141226383640301, 12.81629321302553848 ) ) ;
#5325 = AXIS2_PLACEMENT_3D ( 'NONE', #600, #19337, #4995 ) ;
#5326 = CIRCLE ( 'NONE', #24003, 30.00000000000000355 ) ;
#5327 = CARTESIAN_POINT ( 'NONE',  ( -189.2428547182112766, 13.87687415872436603, 47.31876910929162960 ) ) ;
#5328 = ADVANCED_FACE ( 'NONE', ( #7083 ), #23323, .T. ) ;
#5329 = CARTESIAN_POINT ( 'NONE',  ( -259.2033419157646676, 21.55415060305830366, 21.55415060305842800 ) ) ;
#5330 = CARTESIAN_POINT ( 'NONE',  ( 23.37394308801978937, 23.33966569535129310, -42.85717664514559999 ) ) ;
#5331 = CARTESIAN_POINT ( 'NONE',  ( -259.2033419157646676, -1.438356298054549103E-14, -9.517827891722632216 ) ) ;
#5332 = CARTESIAN_POINT ( 'NONE',  ( -199.9999999999999716, -48.92947633520100226, 14.52307781036571299 ) ) ;
#5333 = EDGE_CURVE ( 'NONE', #15169, #7956, #11201, .T. ) ;
#5334 = B_SPLINE_CURVE_WITH_KNOTS ( 'NONE', 3,
 ( #15033, #11415, #13543, #25165, #4942, #15534 ),
 .UNSPECIFIED., .F., .F.,
 ( 4, 2, 4 ),
 ( -5.998621905481146787E-08, 0.03937827992695891455, 0.07875661984013687666 ),
 .UNSPECIFIED. ) ;
#5335 = FACE_OUTER_BOUND ( 'NONE', #21939, .T. ) ;
#5336 = CARTESIAN_POINT ( 'NONE',  ( 14.38125909742181818, -39.99999999999986500, -15.17850393972675604 ) ) ;
#5337 = CARTESIAN_POINT ( 'NONE',  ( 199.9999999999999432, 2.486775779033024914E-13, -19.99999999999992539 ) ) ;
#5338 = CARTESIAN_POINT ( 'NONE',  ( -82.24528527568789116, 16.01766212874386142, 12.29859689796261435 ) ) ;
#5339 = CARTESIAN_POINT ( 'NONE',  ( 0.2972598230770027716, -38.42060263243656237, -18.14793986248737667 ) ) ;
#5340 = CARTESIAN_POINT ( 'NONE',  ( 4.995406935893290878, -5.232665749138292703E-14, 15.24977328854832592 ) ) ;
#5341 = CARTESIAN_POINT ( 'NONE',  ( 170.2234770963711128, 17.36149277827004411, -17.36149277826983095 ) ) ;
#5342 = DIRECTION ( 'NONE',  ( 0.000000000000000000, 0.3656393565198218232, -0.9307566067258242759 ) ) ;
#5343 = EDGE_CURVE ( 'NONE', #4460, #2152, #13706, .T. ) ;
#5344 = CARTESIAN_POINT ( 'NONE',  ( -362.0709805440841365, -4.857225732735059864E-14, 0.000000000000000000 ) ) ;
#5345 = CARTESIAN_POINT ( 'NONE',  ( -198.0356074513804572, -10.87444709759729911, 10.87444709759714812 ) ) ;
#5346 = CARTESIAN_POINT ( 'NONE',  ( -77.84351360267456243, 20.59686641853765110, -7.423967632478677636 ) ) ;
#5347 = CARTESIAN_POINT ( 'NONE',  ( 151.7948205124836534, -51.78348778862535795, 4.785054706298367044 ) ) ;
#5348 = AXIS2_PLACEMENT_3D ( 'NONE', #68, #12298, #4337 ) ;
#5349 = VECTOR ( 'NONE', #22440, 1000.000000000000000 ) ;
#5350 = CARTESIAN_POINT ( 'NONE',  ( -213.1075012329537230, -66.26714140136188291, -9.698598906438677503 ) ) ;
#5351 = DIRECTION ( 'NONE',  ( 1.000000000000000000, -0.000000000000000000, -0.000000000000000000 ) ) ;
#5352 = DIRECTION ( 'NONE',  ( 1.000000000000000000, -1.836970198721030181E-16, -0.000000000000000000 ) ) ;
#5353 = VERTEX_POINT ( 'NONE', #11708 ) ;
#5354 = CARTESIAN_POINT ( 'NONE',  ( 170.2234770963711128, 39.20704971665372796, 17.36149277827039583 ) ) ;
#5355 = CARTESIAN_POINT ( 'NONE',  ( 199.9999999999999432, 20.00000000000013856, 0.000000000000000000 ) ) ;
#5356 = CARTESIAN_POINT ( 'NONE',  ( 170.0000000000001421, 9.369682556672135121, 22.62041470344889760 ) ) ;
#5357 = ORIENTED_EDGE ( 'NONE', *, *, #5017, .T. ) ;
#5358 = CARTESIAN_POINT ( 'NONE',  ( 130.8568914410475088, -40.00000000000036238, 34.05028731879746573 ) ) ;
#5359 = CARTESIAN_POINT ( 'NONE',  ( 199.0233250129033991, -20.00353002365851651, -0.06339277442724530753 ) ) ;
#5360 = CARTESIAN_POINT ( 'NONE',  ( -70.33906596057607885, 9.443630424063320206, 22.79894064192813730 ) ) ;
#5361 = CIRCLE ( 'NONE', #25392, 44.99999999999997158 ) ;
#5362 = VERTEX_POINT ( 'NONE', #20369 ) ;
#5363 = EDGE_LOOP ( 'NONE', ( #2038, #25045 ) ) ;
#5364 = AXIS2_PLACEMENT_3D ( 'NONE', #7596, #5233, #17709 ) ;
#5365 = CARTESIAN_POINT ( 'NONE',  ( -105.3755690713226585, -12.89780903124383471, -43.67073346367985920 ) ) ;
#5366 = CARTESIAN_POINT ( 'NONE',  ( 130.8568914410475372, 8.154165912415230659E-16, 5.949712681206690945 ) ) ;
#5367 = CARTESIAN_POINT ( 'NONE',  ( -200.0000000000000000, 52.49999999999987210, 82.49999999999998579 ) ) ;
#5368 = CLOSED_SHELL ( 'NONE', ( #17057, #12399, #7002, #21965, #18670, #8007, #25920, #12918, #10358, #5425, #9718, #5494, #21354, #141, #11720, #24847, #22644, #15938, #3879, #8489, #17108 ) ) ;
#5369 = CARTESIAN_POINT ( 'NONE',  ( 199.0053211798077086, 14.13837298227953987, -14.13837298578013701 ) ) ;
#5370 = CARTESIAN_POINT ( 'NONE',  ( 19.06497207195982924, -40.00000000000021316, 54.19242893257830218 ) ) ;
#5371 = CARTESIAN_POINT ( 'NONE',  ( 199.9999999999996874, -18.99916535394237727, -0.6249076428296399532 ) ) ;
#5372 = CARTESIAN_POINT ( 'NONE',  ( 57.59792236341147031, 1.908507979671054758E-14, -2.435789363418160658 ) ) ;
#5373 = COLOUR_RGB ( '',0.7921568627450980005, 0.8196078431372548767, 0.9333333333333333481 ) ;
#5374 = CARTESIAN_POINT ( 'NONE',  ( 160.9163046357249129, -125.7889608577475684, -61.61140153332246427 ) ) ;
#5375 = CARTESIAN_POINT ( 'NONE',  ( -16.78454218927544517, -16.41855578218329725, -39.63790004357984031 ) ) ;
#5376 = CARTESIAN_POINT ( 'NONE',  ( -91.56559293963836410, 44.31723036834908669, -12.25131212657445801 ) ) ;
#5377 = CARTESIAN_POINT ( 'NONE',  ( -87.11162894489338271, -17.01505826597962923, 13.17695786910780242 ) ) ;
#5378 = CARTESIAN_POINT ( 'NONE',  ( -162.0762913951020892, -39.99999999999961631, -41.69427287692722928 ) ) ;
#5379 = DIRECTION ( 'NONE',  ( -1.000000000000000000, 0.000000000000000000, 0.000000000000000000 ) ) ;
#5380 = CARTESIAN_POINT ( 'NONE',  ( 163.1118516004056573, -12.73709011382472589, 40.00000000000002132 ) ) ;
#5381 = CARTESIAN_POINT ( 'NONE',  ( -192.9588430854690273, -14.46834944099973264, -40.00000000000002132 ) ) ;
#5382 = CARTESIAN_POINT ( 'NONE',  ( -91.56559293963836410, 44.31723036834890905, 12.25131212657507795 ) ) ;
#5383 = CARTESIAN_POINT ( 'NONE',  ( 57.59792236341147031, 2.435789363418171760, 0.000000000000000000 ) ) ;
#5385 = DIRECTION ( 'NONE',  ( 0.000000000000000000, 0.000000000000000000, 1.000000000000000000 ) ) ;
#5384 = CARTESIAN_POINT ( 'NONE',  ( 14.33519843538174143, -44.71104701565631956, -24.71012982060716467 ) ) ;
#5386 = CARTESIAN_POINT ( 'NONE',  ( -114.7498586125400948, 21.95311410698565879, -2.658373467578531546 ) ) ;
#5387 = CARTESIAN_POINT ( 'NONE',  ( 163.1118516004056573, -19.27778845539233998, 37.29075403953149959 ) ) ;
#5388 = CARTESIAN_POINT ( 'NONE',  ( -162.0762913951020892, 41.69427287692678163, -40.00000000000002132 ) ) ;
#5389 = ORIENTED_EDGE ( 'NONE', *, *, #8188, .F. ) ;
#5390 = EDGE_CURVE ( 'NONE', #7865, #22425, #6002, .T. ) ;
#5391 = CARTESIAN_POINT ( 'NONE',  ( 23.58679727197032605, -46.73132340479989466, 13.78527791282015080 ) ) ;
#5392 = CARTESIAN_POINT ( 'NONE',  ( -200.0000000000000000, -30.70179486994625861, -44.88127304973837539 ) ) ;
#5393 = EDGE_CURVE ( 'NONE', #7095, #4298, #9853, .T. ) ;
#5394 = CIRCLE ( 'NONE', #25792, 5.000000000000011546 ) ;
#5395 = CARTESIAN_POINT ( 'NONE',  ( 192.4448373802101173, -42.42640687122073473, 14.14213562370301780 ) ) ;
#5396 = CARTESIAN_POINT ( 'NONE',  ( 130.8568914410475372, 1.429239637432775288E-13, -34.05028731879788495 ) ) ;
#5397 = CARTESIAN_POINT ( 'NONE',  ( -77.72102721667458525, 21.24333237935468688, 5.844331514166557717 ) ) ;
#5398 = EDGE_CURVE ( 'NONE', #22348, #12615, #22238, .T. ) ;
#5399 = CARTESIAN_POINT ( 'NONE',  ( 199.0053211801402142, 14.13668625429389891, -14.14005970859717642 ) ) ;
#5400 = CARTESIAN_POINT ( 'NONE',  ( 199.9999999999995737, 11.06459441337805494, 15.46579378046570952 ) ) ;
#5401 = CARTESIAN_POINT ( 'NONE',  ( -87.02161082285356031, -20.76757691164967667, -5.407310480324148294 ) ) ;
#5402 = CARTESIAN_POINT ( 'NONE',  ( -77.65695844554115013, -4.467916498578468065, -21.58737861310262929 ) ) ;
#5403 = CARTESIAN_POINT ( 'NONE',  ( 4.995406935893289102, 10.78321810389013002, -10.78321810388986712 ) ) ;
#5404 = CARTESIAN_POINT ( 'NONE',  ( 163.1118516004056573, 47.56205970284970164, -9.006482792073828847 ) ) ;
#5405 = CARTESIAN_POINT ( 'NONE',  ( -105.2058579006776569, 21.49041530794428567, -0.4803593358688896808 ) ) ;
#5406 = CARTESIAN_POINT ( 'NONE',  ( -105.3755690713226585, 15.38646221621820764, -41.18208027870583265 ) ) ;
#5408 = CARTESIAN_POINT ( 'NONE',  ( 192.4448373802101173, -42.42640687122053578, -14.14213562370360577 ) ) ;
#5407 = CARTESIAN_POINT ( 'NONE',  ( -280.0000000000000000, -14.14213562373088706, -14.14213562373108424 ) ) ;
#5409 = CARTESIAN_POINT ( 'NONE',  ( 136.1360204305621266, 3.511608612530757068, -3.511608612530642937 ) ) ;
#5410 = CARTESIAN_POINT ( 'NONE',  ( 57.59792236341147031, -2.435789363418150444, 0.000000000000000000 ) ) ;
#5411 = DIRECTION ( 'NONE',  ( -1.000000000000000000, -1.836970198721030181E-16, -0.000000000000000000 ) ) ;
#5412 = CARTESIAN_POINT ( 'NONE',  ( -280.0000000000000568, -40.00000000000014211, 19.99999999999987210 ) ) ;
#5413 = CARTESIAN_POINT ( 'NONE',  ( -91.56559293963834989, -16.03295912088728414, 16.03295912088688269 ) ) ;
#5414 = CARTESIAN_POINT ( 'NONE',  ( 192.4448373802101173, 19.99999999996063949, 40.00000000000002132 ) ) ;
#5415 = ORIENTED_EDGE ( 'NONE', *, *, #1674, .F. ) ;
#5416 = CARTESIAN_POINT ( 'NONE',  ( -30.26275506840325136, 29.48230279907798135, -27.08623969584585112 ) ) ;
#5417 = PRODUCT_RELATED_PRODUCT_CATEGORY ( 'part', '', ( #12840 ) ) ;
#5418 = CARTESIAN_POINT ( 'NONE',  ( 8.833560042532678125, 43.71578035519811323, 18.10766911284586200 ) ) ;
#5419 = CARTESIAN_POINT ( 'NONE',  ( 90.68848816916745648, 9.291443204245480203, 21.08311784283745638 ) ) ;
#5420 = CARTESIAN_POINT ( 'NONE',  ( -5.379830816903176327, -46.52611083736033493, -13.73345071524792438 ) ) ;
#5421 = VERTEX_POINT ( 'NONE', #10120 ) ;
#5422 = CARTESIAN_POINT ( 'NONE',  ( -121.8281105900276202, -22.46071553383595187, 10.16551987041848548 ) ) ;
#5423 = CARTESIAN_POINT ( 'NONE',  ( 199.9999999999999147, -13.65919145721374761, -13.21838778087559518 ) ) ;
#5424 = CARTESIAN_POINT ( 'NONE',  ( 90.71510531252879161, -8.810647084079668900, 21.27078368671903164 ) ) ;
#5425 = ADVANCED_FACE ( 'NONE', ( #9720, #23951 ), #26103, .F. ) ;
#5426 = CYLINDRICAL_SURFACE ( 'NONE', #10487, 28.79780246617542616 ) ;
#5427 = CARTESIAN_POINT ( 'NONE',  ( 199.0058938177734547, 17.94521767341456098, -8.824629201450257199 ) ) ;
#5428 = B_SPLINE_CURVE_WITH_KNOTS ( 'NONE', 3,
 ( #4403, #6643, #6906, #18890, #14757, #2930, #12768, #22887, #11039, #11532, #5057, #15278, #9295, #11664, #11405, #9165, #13410, #3309, #5433, #21534, #19527, #7038, #1443, #1311, #25793, #19407 ),
 .UNSPECIFIED., .F., .F.,
 ( 4, 2, 1, 2, 2, 2, 2, 2, 2, 2, 2, 1, 2, 4 ),
 ( -5.999999997206916261E-08, 0.0004354487530732705815, 0.0008709575061465131595, 0.001741975012292999074, 0.003484010024585964399, 0.006968080049171889410, 0.01045215007375781442, 0.01393622009834374030, 0.02090436014751559726, 0.02438843017210152314, 0.02613046518439449475, 0.02700148269054097883, 0.02743699144361421913, 0.02787250019668745596 ),
 .UNSPECIFIED. ) ;
#5429 = B_SPLINE_CURVE_WITH_KNOTS ( 'NONE', 3,
 ( #26105, #26246, #16099, #14238, #11845, #17826, #22240, #24090, #25973, #11981 ),
 .UNSPECIFIED., .F., .F.,
 ( 4, 2, 2, 2, 4 ),
 ( 0.7921542097165071850, 0.8508620842112317728, 0.8814014469398914198, 0.9119408096685510667, 0.9406682828395843687 ),
 .UNSPECIFIED. ) ;
#5430 = CARTESIAN_POINT ( 'NONE',  ( 121.8740240556052470, -26.81399039734623102, 11.10671848392256855 ) ) ;
#5431 = CARTESIAN_POINT ( 'NONE',  ( 192.4448373802101173, 40.00000000000012790, -20.00000000003928236 ) ) ;
#5432 = CARTESIAN_POINT ( 'NONE',  ( -86.96347745069644475, 5.999880687339585546E-14, -21.75974354311649961 ) ) ;
#5433 = CARTESIAN_POINT ( 'NONE',  ( 20.59573805978977035, 47.74081960064699359, -13.93986955483940626 ) ) ;
#5434 = CARTESIAN_POINT ( 'NONE',  ( -56.48582580120559982, 9.153146818113574668, 40.00000000000002132 ) ) ;
#5436 = CARTESIAN_POINT ( 'NONE',  ( -616.1376504080243421, 28.58319296853060720, -27.98701491627070581 ) ) ;
#5435 = CARTESIAN_POINT ( 'NONE',  ( 90.68848423385740887, -8.814708749674085908, -21.28058941768224699 ) ) ;
#5437 = CARTESIAN_POINT ( 'NONE',  ( -259.2033419157646676, 9.517827891722582478, 40.00000000000002132 ) ) ;
#5438 = CARTESIAN_POINT ( 'NONE',  ( 151.7948205124835681, 33.23291073765556547, -40.00000000000002132 ) ) ;
#5439 = CARTESIAN_POINT ( 'NONE',  ( 130.8568914410475372, -34.05028731879786363, 0.000000000000000000 ) ) ;
#5440 = CARTESIAN_POINT ( 'NONE',  ( -105.3755690713226585, 40.00000000000019185, -18.24025645688310249 ) ) ;
#5441 = CARTESIAN_POINT ( 'NONE',  ( 151.7948205124836534, -39.99999999999992184, -6.767089262349454515 ) ) ;
#5442 = CARTESIAN_POINT ( 'NONE',  ( 158.3376637473630240, -26.51176758098464958, -10.98153369452720796 ) ) ;
#5443 = VERTEX_POINT ( 'NONE', #9984 ) ;
#5445 = CARTESIAN_POINT ( 'NONE',  ( -1.087763065869005397, 47.95583523902985235, -13.97201973056374946 ) ) ;
#5444 = CARTESIAN_POINT ( 'NONE',  ( -53.37769371643640426, -29.42719939405413854, 10.11111068829016801 ) ) ;
#5446 = CARTESIAN_POINT ( 'NONE',  ( 192.4448373802100889, -19.99999999996057198, -2.449293598294708485E-15 ) ) ;
#5447 = CARTESIAN_POINT ( 'NONE',  ( 14.38125909742180752, 10.73282306404735387, -10.73282306404708919 ) ) ;
#5448 = CARTESIAN_POINT ( 'NONE',  ( -105.4732637872235728, -8.153770687239582315, 19.68494377761378544 ) ) ;
#5449 =( NAMED_UNIT ( * ) PLANE_ANGLE_UNIT ( ) SI_UNIT ( $, .RADIAN. ) );
#5450 = VERTEX_POINT ( 'NONE', #8119 ) ;
#5451 = ORIENTED_EDGE ( 'NONE', *, *, #22923, .F. ) ;
#5452 = CYLINDRICAL_SURFACE ( 'NONE', #4519, 5.000000000000095035 ) ;
#5453 = CARTESIAN_POINT ( 'NONE',  ( 140.2235668266255857, 12.60094438999845678, -30.42137084504298272 ) ) ;
#5454 = VERTEX_POINT ( 'NONE', #17823 ) ;
#5455 = ORIENTED_EDGE ( 'NONE', *, *, #14107, .T. ) ;
#5456 = ORIENTED_EDGE ( 'NONE', *, *, #19531, .F. ) ;
#5457 = CARTESIAN_POINT ( 'NONE',  ( 199.0263771350486763, -14.37646237564524476, 13.91501816527019919 ) ) ;
#5458 = CARTESIAN_POINT ( 'NONE',  ( -192.9588430854690273, 66.79921049721887982, 10.23066800229522677 ) ) ;
#5459 = DIRECTION ( 'NONE',  ( 1.000000000000000000, -1.836970198721030181E-16, -0.000000000000000000 ) ) ;
#5460 = CARTESIAN_POINT ( 'NONE',  ( 184.8905102610680444, 1.070102760522089011E-13, -20.92133201514444352 ) ) ;
#5461 = DIRECTION ( 'NONE',  ( 1.000000000000000000, 0.000000000000000000, 0.000000000000000000 ) ) ;
#5462 = CARTESIAN_POINT ( 'NONE',  ( -362.0709805440841365, -4.857225732735059864E-14, 0.000000000000000000 ) ) ;
#5463 = CARTESIAN_POINT ( 'NONE',  ( 98.29820294273055481, 14.14213562373424971, 14.14213562373465116 ) ) ;
#5464 = CARTESIAN_POINT ( 'NONE',  ( 98.29820294267423719, -14.14213562374330024, 14.14213562372619926 ) ) ;
#5465 = CARTESIAN_POINT ( 'NONE',  ( -198.0356074513804572, -39.99999999999948130, -55.37879056874863437 ) ) ;
#5466 = CARTESIAN_POINT ( 'NONE',  ( -105.4741150117390447, -8.366608964578304608, 19.60045294983322961 ) ) ;
#5467 = CARTESIAN_POINT ( 'NONE',  ( -86.96347745069644475, 15.38646221621793586, -15.38646221621778842 ) ) ;
#5468 = CARTESIAN_POINT ( 'NONE',  ( 0.2972598230769957217, -4.999556039334937811E-14, 14.33493731733933352 ) ) ;
#5469 = CARTESIAN_POINT ( 'NONE',  ( -114.4364955367336449, 20.04994829326807348, -8.644468109231272734 ) ) ;
#5470 = CARTESIAN_POINT ( 'NONE',  ( 159.7744820660626317, 25.95909830917683792, 10.75261058663758540 ) ) ;
#5471 = AXIS2_PLACEMENT_3D ( 'NONE', #23943, #7196, #15433 ) ;
#5472 = B_SPLINE_CURVE_WITH_KNOTS ( 'NONE', 3,
 ( #13441, #3336, #11436, #1347, #9449, #25693 ),
 .UNSPECIFIED., .F., .F.,
 ( 4, 2, 4 ),
 ( 0.0002283715791020996064, 0.004317053718188323432, 0.008405735857274547473 ),
 .UNSPECIFIED. ) ;
#5473 = DIRECTION ( 'NONE',  ( 0.000000000000000000, -1.000000000000000000, 0.000000000000000000 ) ) ;
#5474 = CARTESIAN_POINT ( 'NONE',  ( -192.9588430854689989, -10.23066800230756890, 10.23066800230742501 ) ) ;
#5475 = CARTESIAN_POINT ( 'NONE',  ( 170.2234770963711128, -39.99999999999991473, -24.55285855007201334 ) ) ;
#5476 = CARTESIAN_POINT ( 'NONE',  ( 130.8568914410475088, -24.07718906446910623, 32.49135343045471558 ) ) ;
#5477 = CARTESIAN_POINT ( 'NONE',  ( 184.8905102610680444, -13.49065550809791603, -13.49065550809818781 ) ) ;
#5478 = CARTESIAN_POINT ( 'NONE',  ( -144.0562696877137796, -14.68019673979266848, -29.54283206235778536 ) ) ;
#5479 = CARTESIAN_POINT ( 'NONE',  ( 14.32711916788072770, 24.71075626504586609, 44.71189734681512107 ) ) ;
#5480 = ORIENTED_EDGE ( 'NONE', *, *, #1775, .F. ) ;
#5481 = CARTESIAN_POINT ( 'NONE',  ( 200.0000000000000000, 42.42640687119267540, 14.14213562373153543 ) ) ;
#5482 = CARTESIAN_POINT ( 'NONE',  ( -626.9846540392142060, 75.00000000000000000, 0.000000000000000000 ) ) ;
#5483 = CARTESIAN_POINT ( 'NONE',  ( -622.1697599706657229, 28.66687854691249981, 34.68786982843303690 ) ) ;
#5484 = ORIENTED_EDGE ( 'NONE', *, *, #3118, .F. ) ;
#5485 = CARTESIAN_POINT ( 'NONE',  ( -105.3755690713226727, -2.472783935621397949E-13, 21.75974354311649961 ) ) ;
#5486 = CARTESIAN_POINT ( 'NONE',  ( 199.0263117864500657, -15.86583567901655911, 12.25628060790395679 ) ) ;
#5487 = CARTESIAN_POINT ( 'NONE',  ( -726.9846540392142060, 66.50000000000009948, 66.50000000000005684 ) ) ;
#5488 = VERTEX_POINT ( 'NONE', #7841 ) ;
#5489 = EDGE_LOOP ( 'NONE', ( #22288, #9933, #13800, #10941 ) ) ;
#5490 = CARTESIAN_POINT ( 'NONE',  ( 4.995406935893289102, 55.24977328856464709, -40.00000000000002132 ) ) ;
#5491 = CARTESIAN_POINT ( 'NONE',  ( -86.96347745069644475, 15.38646221621793586, -15.38646221621778842 ) ) ;
#5492 = CARTESIAN_POINT ( 'NONE',  ( -162.0762913951020892, 39.99999999999985079, 41.69427287692695216 ) ) ;
#5493 = CARTESIAN_POINT ( 'NONE',  ( 98.29820294267312875, 7.653668647304333383, -18.47759065023115355 ) ) ;
#5494 = ADVANCED_FACE ( 'NONE', ( #15822 ), #4152, .T. ) ;
#5495 = CIRCLE ( 'NONE', #23752, 5.000000000000004441 ) ;
#5496 = CARTESIAN_POINT ( 'NONE',  ( -192.9588430854689989, 38.51493924976983152, -38.51493924976893624 ) ) ;
#5497 = CARTESIAN_POINT ( 'NONE',  ( -213.1075012329537230, -40.00000000000025580, 53.71589010953650956 ) ) ;
#5498 = CARTESIAN_POINT ( 'NONE',  ( 200.0000000000001137, -16.46591192518303970, -9.498466322123544359 ) ) ;
#5499 = CARTESIAN_POINT ( 'NONE',  ( 0.2972598230769883387, 39.99999999999997158, 14.33493731733947563 ) ) ;
#5500 = CYLINDRICAL_SURFACE ( 'NONE', #23652, 30.00000000000000711 ) ;
#5501 = FACE_OUTER_BOUND ( 'NONE', #1270, .T. ) ;
#5502 = CARTESIAN_POINT ( 'NONE',  ( -100.7734535825088500, 16.03295912088740494, -40.53558337403661938 ) ) ;
#5503 = DIRECTION ( 'NONE',  ( 0.000000000000000000, -1.000000000000000000, 0.000000000000000000 ) ) ;
#5504 = CARTESIAN_POINT ( 'NONE',  ( -213.1075012329537230, -39.99999999999991473, -13.71589010951953647 ) ) ;
#5505 = DIRECTION ( 'NONE',  ( -1.836970198721030427E-16, 1.000000000000000000, -1.682156097916904327E-16 ) ) ;
#5506 = CARTESIAN_POINT ( 'NONE',  ( -91.56559293963836410, 22.67402823373189946, -0.000000000000000000 ) ) ;
#5507 = CARTESIAN_POINT ( 'NONE',  ( -208.1127848780264742, -15.00245453012673202, -40.00000000000002132 ) ) ;
#5508 = CARTESIAN_POINT ( 'NONE',  ( 14.38125909742181285, -10.73282306404727393, 10.73282306404716380 ) ) ;
#5509 = CARTESIAN_POINT ( 'NONE',  ( 4.995406935893293543, -15.24977328854832592, 0.000000000000000000 ) ) ;
#5510 = CARTESIAN_POINT ( 'NONE',  ( 163.1118516004056573, -19.27778845538787422, 19.27778845538743724 ) ) ;
#5511 = CARTESIAN_POINT ( 'NONE',  ( 136.1360204305621266, -3.419521671106983309E-13, 35.03383547441296741 ) ) ;
#5512 = CARTESIAN_POINT ( 'NONE',  ( -30.26275506840325136, 57.76657404653985139, 1.198031551616126178 ) ) ;
#5513 = CARTESIAN_POINT ( 'NONE',  ( 163.1118516004056573, 12.73709011382478273, 2.449293598294708485E-15 ) ) ;
#5514 = ORIENTED_EDGE ( 'NONE', *, *, #17819, .T. ) ;
#5515 = CIRCLE ( 'NONE', #7624, 15.00000000000000178 ) ;
#5516 = CARTESIAN_POINT ( 'NONE',  ( 90.68848816917943623, -21.08311784259292665, 9.291443204823380597 ) ) ;
#5517 = CARTESIAN_POINT ( 'NONE',  ( -199.9999999999999432, -42.45148791632019680, -35.57044988732180002 ) ) ;
#5518 = CARTESIAN_POINT ( 'NONE',  ( 91.82158438592158234, 44.40256751092336884, -12.16597498400043342 ) ) ;
#5519 = CARTESIAN_POINT ( 'NONE',  ( -91.56559293963834989, -7.976292724337646577E-14, 17.32597176626811120 ) ) ;
#5520 = CARTESIAN_POINT ( 'NONE',  ( -30.26275506840324070, 1.198031551616030033, -1.198031551616006496 ) ) ;
#5521 = CARTESIAN_POINT ( 'NONE',  ( -30.26275506840324425, 1.694272468446254232, -40.00000000000002132 ) ) ;
#5522 = DIRECTION ( 'NONE',  ( -1.000000000000000000, -1.836970198721030181E-16, -1.232595164407830946E-32 ) ) ;
#5523 = CARTESIAN_POINT ( 'NONE',  ( 199.9999999999998295, 10.02997355460652429, 16.14748021227288532 ) ) ;
#5524 = CARTESIAN_POINT ( 'NONE',  ( -77.55658273862232477, -1.402866402507712218, -22.13039188814530789 ) ) ;
#5525 = CARTESIAN_POINT ( 'NONE',  ( 57.59792236341147031, -1.722363176415055985, 1.722363176415024677 ) ) ;
#5526 = CARTESIAN_POINT ( 'NONE',  ( 130.8568914410475088, 24.07718906446937623, -32.49135343045455215 ) ) ;
#5527 = AXIS2_PLACEMENT_3D ( 'NONE', #15478, #13360, #17734 ) ;
#5528 = FACE_OUTER_BOUND ( 'NONE', #14582, .T. ) ;
#5529 = CARTESIAN_POINT ( 'NONE',  ( 19.06497207195981147, 1.521599808664285085E-13, -14.19242893257840521 ) ) ;
#5530 = CARTESIAN_POINT ( 'NONE',  ( 4.995406935893300648, -10.78321810387790514, -67.35176059880241439 ) ) ;
#5532 = CARTESIAN_POINT ( 'NONE',  ( 19.06497207195981858, 10.03556273973516078, -66.60410523465806421 ) ) ;
#5531 = CARTESIAN_POINT ( 'NONE',  ( -280.0000000000000568, 14.14213562373127431, -42.42640687119274645 ) ) ;
#5533 = CARTESIAN_POINT ( 'NONE',  ( 19.06497207195980792, 10.03556273973447155, -10.03556273973422286 ) ) ;
#5534 = CARTESIAN_POINT ( 'NONE',  ( -211.2619052429883482, 0.000000000000000000, -75.00000000000000000 ) ) ;
#5535 = DIRECTION ( 'NONE',  ( 0.000000000000000000, 1.000000000000000000, 0.000000000000000000 ) ) ;
#5537 = CARTESIAN_POINT ( 'NONE',  ( 151.7948205124836534, -39.99999999999987921, -33.23291073765567916 ) ) ;
#5536 = CARTESIAN_POINT ( 'NONE',  ( -105.3755690713226585, 12.89780903124349720, 43.67073346367994446 ) ) ;
#5538 = CARTESIAN_POINT ( 'NONE',  ( 19.06497207195981858, -10.03556273973469715, 66.60410523465813526 ) ) ;
#5539 = CARTESIAN_POINT ( 'NONE',  ( 199.9999999999999432, -14.14213562373115884, 14.14213562373085153 ) ) ;
#5540 = CARTESIAN_POINT ( 'NONE',  ( -86.96347745069644475, 18.24025645688350750, 40.00000000000002132 ) ) ;
#5541 = EDGE_LOOP ( 'NONE', ( #2625, #9743, #15449, #16581 ) ) ;
#5542 = CARTESIAN_POINT ( 'NONE',  ( -213.1075012329537230, 9.698598906450410340, 9.698598906450483170 ) ) ;
#5543 = CARTESIAN_POINT ( 'NONE',  ( -70.70793901134142345, 22.66153234904986746, 9.386714043133100205 ) ) ;
#5544 = CARTESIAN_POINT ( 'NONE',  ( 23.58679727196918918, 23.29637218066034521, 42.79169916605225410 ) ) ;
#5545 = CARTESIAN_POINT ( 'NONE',  ( -280.0000000000000568, -20.00000000000006750, 40.00000000000002132 ) ) ;
#5546 = ORIENTED_EDGE ( 'NONE', *, *, #1431, .F. ) ;
#5547 = CARTESIAN_POINT ( 'NONE',  ( -194.4222775680590871, -48.65439176089972051, 14.07715774765395267 ) ) ;
#5548 = CARTESIAN_POINT ( 'NONE',  ( 199.9999999999999716, -6.704437273156823807, -17.78382994799445527 ) ) ;
#5549 = CARTESIAN_POINT ( 'NONE',  ( 23.36927571439213480, -13.80130822340191443, 46.80992244775416111 ) ) ;
#5550 = CARTESIAN_POINT ( 'NONE',  ( 20.16956056503097372, 13.95858718339115434, -47.86583268168163130 ) ) ;
#5551 = CARTESIAN_POINT ( 'NONE',  ( 199.0056007646616933, 10.55815519723130969, -16.98307562551513072 ) ) ;
#5552 = UNCERTAINTY_MEASURE_WITH_UNIT (LENGTH_MEASURE( 1.000000000000000082E-05 ), #5889, 'distance_accuracy_value', 'NONE');
#5553 = CARTESIAN_POINT ( 'NONE',  ( -93.02511667906934179, -20.50052124204830406, -8.946512270084891583 ) ) ;
#5554 = CARTESIAN_POINT ( 'NONE',  ( -162.0762913951020892, -3.568845385355699554E-14, 1.694272876828323948 ) ) ;
#5555 = CARTESIAN_POINT ( 'NONE',  ( 151.7948205124836250, 1.439163438361279259E-13, -33.23291073765553705 ) ) ;
#5556 = ADVANCED_FACE ( 'NONE', ( #19962, #24088, #13968, #2143, #12112, #18221, #10254, #24364 ), #22103, .T. ) ;
#5557 = DIRECTION ( 'NONE',  ( -1.000000000000000000, -0.000000000000000000, -0.000000000000000000 ) ) ;
#5558 = CARTESIAN_POINT ( 'NONE',  ( -238.4067589809705794, -40.96449428006345528, 40.00000000000002132 ) ) ;
#5559 = VECTOR ( 'NONE', #14133, 1000.000000000000000 ) ;
#5561 = CARTESIAN_POINT ( 'NONE',  ( -614.3679688017556373, 29.30921813701808176, -27.22223345538390404 ) ) ;
#5560 = CARTESIAN_POINT ( 'NONE',  ( 83.06440094991440048, -9.006081069352781299, -24.44702070095364377 ) ) ;
#5562 = EDGE_CURVE ( 'NONE', #15457, #16014, #295, .T. ) ;
#5563 = CARTESIAN_POINT ( 'NONE',  ( 192.4448373802100889, 20.00000000003945644, 0.000000000000000000 ) ) ;
#5564 = CARTESIAN_POINT ( 'NONE',  ( -86.96347745069645896, 21.75974354311648895, -0.000000000000000000 ) ) ;
#5565 = VECTOR ( 'NONE', #20104, 1000.000000000000000 ) ;
#5566 = CARTESIAN_POINT ( 'NONE',  ( -100.7734535825088358, -22.67402823373193499, 0.000000000000000000 ) ) ;
#5567 = CARTESIAN_POINT ( 'NONE',  ( -208.1127848780265026, 5.403397259664334602E-13, -55.00245453012672670 ) ) ;
#5568 = CARTESIAN_POINT ( 'NONE',  ( 163.1118516004056573, -2.556006622855449647E-13, 27.26290988616872824 ) ) ;
#5569 = CARTESIAN_POINT ( 'NONE',  ( -238.4067589809705794, -0.6820004457913585449, -0.6820004457913265705 ) ) ;
#5570 = EDGE_CURVE ( 'NONE', #22478, #19077, #3683, .T. ) ;
#5571 = EDGE_CURVE ( 'NONE', #7340, #1564, #11979, .T. ) ;
#5572 = ORIENTED_EDGE ( 'NONE', *, *, #17908, .F. ) ;
#5573 = CARTESIAN_POINT ( 'NONE',  ( -200.0000000000000000, 69.99999999999998579, 0.000000000000000000 ) ) ;
#5574 = DIRECTION ( 'NONE',  ( 1.000000000000000000, 1.836970198721030181E-16, 0.000000000000000000 ) ) ;
#5575 = CARTESIAN_POINT ( 'NONE',  ( -188.2995950289364089, 46.99046209955525200, -13.82811170417133617 ) ) ;
#5576 = VERTEX_POINT ( 'NONE', #16097 ) ;
#5577 = ORIENTED_EDGE ( 'NONE', *, *, #4779, .T. ) ;
#5578 = CARTESIAN_POINT ( 'NONE',  ( -89.92902785008901390, -20.17328762787336061, 8.734793929541309510 ) ) ;
#5579 = CARTESIAN_POINT ( 'NONE',  ( 22.01478053668312640, -47.29427690643675675, -13.87318432394964773 ) ) ;
#5580 = VERTEX_POINT ( 'NONE', #11841 ) ;
#5581 = CARTESIAN_POINT ( 'NONE',  ( 4.995406935893288214, 15.24977328854832770, -40.00000000000002132 ) ) ;
#5582 = DIRECTION ( 'NONE',  ( 0.000000000000000000, 0.3028247695821854046, -0.9530462522498561739 ) ) ;
#5583 = ORIENTED_EDGE ( 'NONE', *, *, #9954, .F. ) ;
#5584 = CARTESIAN_POINT ( 'NONE',  ( 200.0000000000000284, -9.508146755684434126, 16.46234680784547777 ) ) ;
#5585 = AXIS2_PLACEMENT_3D ( 'NONE', #16615, #10501, #10769 ) ;
#5586 = CARTESIAN_POINT ( 'NONE',  ( -265.6482238768269326, 4.898587196589409082E-15, 39.99999999999997158 ) ) ;
#5587 = CARTESIAN_POINT ( 'NONE',  ( -91.56559293963834989, 12.25131212657480440, 12.25131212657486834 ) ) ;
#5588 = CARTESIAN_POINT ( 'NONE',  ( -215.0000000000000284, 63.70262460423102624, -57.69613583541415380 ) ) ;
#5589 = CARTESIAN_POINT ( 'NONE',  ( 19.06497207195981147, -4.605042221739098431E-14, 14.19242893257840521 ) ) ;
#5590 = CARTESIAN_POINT ( 'NONE',  ( -162.0762913951020892, 1.198031840456041497, -57.76657433537918251 ) ) ;
#5591 = CARTESIAN_POINT ( 'NONE',  ( -351.0000000000000568, -4.857225732735059864E-14, 0.000000000000000000 ) ) ;
#5592 = CARTESIAN_POINT ( 'NONE',  ( -259.2033419157646676, -1.438356298054549103E-14, -9.517827891722632216 ) ) ;
#5593 = CARTESIAN_POINT ( 'NONE',  ( -30.26275506840324070, 1.218738420030236455E-14, -1.694272468446259783 ) ) ;
#5594 = CARTESIAN_POINT ( 'NONE',  ( 151.7948205124836534, -39.99999999999992184, -6.767089262349454515 ) ) ;
#5595 = CARTESIAN_POINT ( 'NONE',  ( -200.0000000000000000, -45.06067021511792348, -22.35311919176578499 ) ) ;
#5596 = CARTESIAN_POINT ( 'NONE',  ( -100.7734535825088500, 16.03295912088713848, -16.03295912088698927 ) ) ;
#5597 = DIRECTION ( 'NONE',  ( -0.01051738777841000790, -0.3995761382614314572, 0.9166396752739868203 ) ) ;
#5598 = CARTESIAN_POINT ( 'NONE',  ( 184.8905102610680444, -41.77492675555986779, -14.79361573936407304 ) ) ;
#5599 = DIRECTION ( 'NONE',  ( 0.000000000000000000, 1.000000000000000000, 0.000000000000000000 ) ) ;
#5600 = DIRECTION ( 'NONE',  ( 1.000000000000000000, 1.836970198721030181E-16, -0.000000000000000000 ) ) ;
#5601 = CARTESIAN_POINT ( 'NONE',  ( 192.4448373802100889, -1.741373372144848397E-13, 20.00000000003942091 ) ) ;
#5602 = CARTESIAN_POINT ( 'NONE',  ( 151.7948205124836534, -39.99999999999987921, -33.23291073765567916 ) ) ;
#5603 = CARTESIAN_POINT ( 'NONE',  ( -208.1127848780265026, 38.89260858015724409, 38.89260858015741462 ) ) ;
#5604 = CIRCLE ( 'NONE', #10729, 69.99999999999992895 ) ;
#5605 = CARTESIAN_POINT ( 'NONE',  ( -280.0000000000000000, 14.14213562373078581, 14.14213562373108424 ) ) ;
#5606 = CARTESIAN_POINT ( 'NONE',  ( -194.7884774423998238, -18.40784251728203458, -44.44046305925559892 ) ) ;
#5607 = CARTESIAN_POINT ( 'NONE',  ( 146.6084372240433993, -3.357462877844280890E-13, 34.62501878078305850 ) ) ;
#5608 = ORIENTED_EDGE ( 'NONE', *, *, #21741, .F. ) ;
#5609 = CARTESIAN_POINT ( 'NONE',  ( 130.8568914410475088, 32.49135343045448820, 24.07718906446946860 ) ) ;
#5610 = CARTESIAN_POINT ( 'NONE',  ( -208.1127848780265026, -15.00245453012673202, 0.000000000000000000 ) ) ;
#5611 = CARTESIAN_POINT ( 'NONE',  ( -716.9846540392142060, 52.50000000000007816, 52.49999999999999289 ) ) ;
#5612 = CARTESIAN_POINT ( 'NONE',  ( -56.48582580120559982, -6.472252184283581400, -50.09629031063973059 ) ) ;
#5613 = CARTESIAN_POINT ( 'NONE',  ( -86.86493150570900923, 7.943527260525790723, 19.77569912837828880 ) ) ;
#5614 = ORIENTED_EDGE ( 'NONE', *, *, #16291, .F. ) ;
#5615 = CARTESIAN_POINT ( 'NONE',  ( 200.0000000000000000, 16.22959744068430155, -9.888235504304919488 ) ) ;
#5616 = CARTESIAN_POINT ( 'NONE',  ( 199.0221430437530898, -19.77959184285664307, -3.052687890358243283 ) ) ;
#5617 = CARTESIAN_POINT ( 'NONE',  ( -0.5869797817581398069, 18.21245090265434996, 43.96874597320426403 ) ) ;
#5618 = EDGE_LOOP ( 'NONE', ( #9317, #7959, #10627, #13945 ) ) ;
#5619 = ORIENTED_EDGE ( 'NONE', *, *, #5245, .T. ) ;
#5620 = CARTESIAN_POINT ( 'NONE',  ( 57.59792236341147031, 37.56421063658187620, 2.449293598294708485E-15 ) ) ;
#5621 = CARTESIAN_POINT ( 'NONE',  ( -259.2033419157646676, 6.730120644403521979, -6.730120644403498886 ) ) ;
#5622 = CARTESIAN_POINT ( 'NONE',  ( -91.56559293963836410, 39.99999999999994316, 17.32597176626825330 ) ) ;
#5623 = CARTESIAN_POINT ( 'NONE',  ( 199.0053211804427633, 14.13331159297750617, -14.14343255912447361 ) ) ;
#5624 = DIRECTION ( 'NONE',  ( 1.000000000000000000, 1.303213150798907793E-16, 2.465190328815661892E-32 ) ) ;
#5625 = CARTESIAN_POINT ( 'NONE',  ( 4.995406935893283773, 40.00000000000017764, -15.24977328854790848 ) ) ;
#5626 = CARTESIAN_POINT ( 'NONE',  ( 200.0000000000002274, -14.59760583945227808, 12.17906594671359244 ) ) ;
#5627 = CARTESIAN_POINT ( 'NONE',  ( -170.8329924482306410, 37.82183460435096123, 15.66631684693926907 ) ) ;
#5628 = CARTESIAN_POINT ( 'NONE',  ( 2.303792037523120673, -18.40682559463839496, -44.43800799080462127 ) ) ;
#5629 = CARTESIAN_POINT ( 'NONE',  ( -30.26275506840323359, -1.198031551615522439, -57.76657404653986561 ) ) ;
#5630 = CARTESIAN_POINT ( 'NONE',  ( -77.59261320674056606, -21.93453874212654853, 2.779275804850804388 ) ) ;
#5631 = DIRECTION ( 'NONE',  ( 1.000000000000000000, 1.836970198721030427E-16, -0.000000000000000000 ) ) ;
#5632 = CARTESIAN_POINT ( 'NONE',  ( -105.3895334812064988, -20.30817960290562141, -6.678845697774401735 ) ) ;
#5633 = CARTESIAN_POINT ( 'NONE',  ( 91.82158438592159655, -22.79471317813468900, 40.00000000000002132 ) ) ;
#5634 = CARTESIAN_POINT ( 'NONE',  ( 136.1360204305621266, -4.966164525587039691, -2.449293598294708485E-15 ) ) ;
#5635 = CARTESIAN_POINT ( 'NONE',  ( 91.82158438592158234, 12.16597498397773869, -12.16597498397759303 ) ) ;
#5636 = CARTESIAN_POINT ( 'NONE',  ( 151.7948205124836250, 33.23291073765556547, 0.000000000000000000 ) ) ;
#5637 = CARTESIAN_POINT ( 'NONE',  ( -105.5018627849130723, 19.74131065641399729, 7.980562150497299001 ) ) ;
#5638 = EDGE_CURVE ( 'NONE', #24441, #2026, #20384, .T. ) ;
#5639 = CARTESIAN_POINT ( 'NONE',  ( 163.1118516004056573, -2.556006622855449647E-13, 27.26290988616872824 ) ) ;
#5640 = CARTESIAN_POINT ( 'NONE',  ( -213.1075012329537230, 66.26714140136188291, 9.698598906438215650 ) ) ;
#5641 = CARTESIAN_POINT ( 'NONE',  ( -100.7734535825088358, 17.32597176626809343, 2.449293598294708485E-15 ) ) ;
#5642 = ORIENTED_EDGE ( 'NONE', *, *, #23903, .T. ) ;
#5643 = CARTESIAN_POINT ( 'NONE',  ( 98.29820294267354086, -18.47759065023110736, 7.653668647303992323 ) ) ;
#5644 = FACE_OUTER_BOUND ( 'NONE', #2789, .T. ) ;
#5645 = CARTESIAN_POINT ( 'NONE',  ( 136.1360204305621551, 3.511608612530801032, -53.05693388239316022 ) ) ;
#5646 = CARTESIAN_POINT ( 'NONE',  ( 151.7948205124836250, 1.807796684091926154E-15, 6.767089262349031742 ) ) ;
#5647 = CARTESIAN_POINT ( 'NONE',  ( -198.0356074513804572, 10.87444709759730088, -10.87444709759707173 ) ) ;
#5648 = DIRECTION ( 'NONE',  ( 1.303213150798907793E-16, -1.000000000000000000, 0.000000000000000000 ) ) ;
#5649 = EDGE_CURVE ( 'NONE', #19014, #6051, #9567, .T. ) ;
#5650 = CARTESIAN_POINT ( 'NONE',  ( 4.995406935893288214, 15.24977328854832770, -40.00000000000002132 ) ) ;
#5651 = FACE_BOUND ( 'NONE', #7221, .T. ) ;
#5652 = CARTESIAN_POINT ( 'NONE',  ( 200.0000000000001990, -4.022463818607304731, 18.57981244883409744 ) ) ;
#5653 = CARTESIAN_POINT ( 'NONE',  ( -77.59243545043536017, 2.773626963377854526, -21.93550214427983391 ) ) ;
#5654 = B_SPLINE_CURVE_WITH_KNOTS ( 'NONE', 3,
 ( #14116, #4018, #2149, #148, #7717, #2023, #3743, #15827, #24093, #11848, #12118, #20243, #19969, #10125, #1750, #5868 ),
 .UNSPECIFIED., .F., .F.,
 ( 4, 2, 2, 2, 2, 2, 2, 4 ),
 ( 1.329418552447366687E-15, 0.004250215530321975466, 0.006375323295482298799, 0.008500431060642620398, 0.01275064659096327400, 0.01381320047354344174, 0.01487575435612360948, 0.01700086212128394322 ),
 .UNSPECIFIED. ) ;
#5655 = CARTESIAN_POINT ( 'NONE',  ( 170.2234770963711128, -17.36149277827010096, 17.36149277826970660 ) ) ;
#5656 = CARTESIAN_POINT ( 'NONE',  ( 0.2972598230770100991, -38.42060263243632079, -38.42060263243699580 ) ) ;
#5657 = CARTESIAN_POINT ( 'NONE',  ( -114.7505577291900352, 21.95690638031361530, -2.633416689372234831 ) ) ;
#5658 = CARTESIAN_POINT ( 'NONE',  ( -213.1075012329537230, 1.045191102001431893E-13, -13.71589010951911902 ) ) ;
#5659 = CARTESIAN_POINT ( 'NONE',  ( -238.4067589809705794, -28.96627169325303797, -28.96627169325349627 ) ) ;
#5661 = CARTESIAN_POINT ( 'NONE',  ( -30.26275506840324070, 1.198031551616724366, -57.76657404653984429 ) ) ;
#5660 = CARTESIAN_POINT ( 'NONE',  ( 14.38125909742182529, -39.01709431150879936, -39.01709431150948859 ) ) ;
#5662 = CARTESIAN_POINT ( 'NONE',  ( -86.96347745069644475, -43.67073346367964604, -12.89780903124457545 ) ) ;
#5663 = DIRECTION ( 'NONE',  ( -1.000000000000000000, -1.836970198721030181E-16, 0.000000000000000000 ) ) ;
#5664 = FACE_OUTER_BOUND ( 'NONE', #8219, .T. ) ;
#5666 = CARTESIAN_POINT ( 'NONE',  ( 163.1118516004056573, 1.251511021549353291E-13, -27.26290988616872824 ) ) ;
#5665 = CARTESIAN_POINT ( 'NONE',  ( -86.96347745069644475, 41.18208027870576871, 15.38646221621837107 ) ) ;
#5667 = CARTESIAN_POINT ( 'NONE',  ( -105.3755690713226585, 43.67073346367970288, 12.89780903124427702 ) ) ;
#5668 = CARTESIAN_POINT ( 'NONE',  ( 4.995406935893289102, 10.78321810389013002, -10.78321810388986712 ) ) ;
#5669 = CARTESIAN_POINT ( 'NONE',  ( -162.0762913951021176, 1.694272876828294194, 40.00000000000002132 ) ) ;
#5670 = ORIENTED_EDGE ( 'NONE', *, *, #25498, .F. ) ;
#5671 = CARTESIAN_POINT ( 'NONE',  ( -198.0356074513804572, 39.15871834505912119, -17.40982414986464377 ) ) ;
#5672 = FACE_OUTER_BOUND ( 'NONE', #12887, .T. ) ;
#5673 = DIRECTION ( 'NONE',  ( -1.000000000000000000, 0.000000000000000000, 0.000000000000000000 ) ) ;
#5674 = CARTESIAN_POINT ( 'NONE',  ( 19.06497207195980792, 14.19242893257840876, 0.000000000000000000 ) ) ;
#5675 = VERTEX_POINT ( 'NONE', #22763 ) ;
#5676 = CARTESIAN_POINT ( 'NONE',  ( -3.971463587461111722, 23.46415232638922888, -43.02522237042865072 ) ) ;
#5677 = CARTESIAN_POINT ( 'NONE',  ( 200.0000000000000568, -17.44062545528135999, -7.562669404541021656 ) ) ;
#5678 = CARTESIAN_POINT ( 'NONE',  ( -3.379936260373897383, -17.94397654175175560, 43.32059152999903517 ) ) ;
#5679 = AXIS2_PLACEMENT_3D ( 'NONE', #3653, #11760, #17871 ) ;
#5680 = CARTESIAN_POINT ( 'NONE',  ( 20.91285618074644503, 23.84652503048867089, -43.54130497317085968 ) ) ;
#5681 = CARTESIAN_POINT ( 'NONE',  ( 199.0062801269303350, 18.72091001596172433, -7.031396878026334285 ) ) ;
#5682 = FACE_OUTER_BOUND ( 'NONE', #20386, .T. ) ;
#5683 = CARTESIAN_POINT ( 'NONE',  ( 136.1360204305621266, 1.473277640373554421E-13, -35.03383547441296741 ) ) ;
#5684 = FACE_OUTER_BOUND ( 'NONE', #14455, .T. ) ;
#5685 = CARTESIAN_POINT ( 'NONE',  ( -91.56559293963834989, 40.53558337403654832, 16.03295912088756481 ) ) ;
#5686 = CARTESIAN_POINT ( 'NONE',  ( 136.1360204305621266, -4.966164525587039691, -2.449293598294708485E-15 ) ) ;
#5688 = CARTESIAN_POINT ( 'NONE',  ( -600.2384622940975305, 37.62094780669912097, -13.59727104935886821 ) ) ;
#5687 = CARTESIAN_POINT ( 'NONE',  ( 59.93546481446576024, -13.19882033562139512, -31.86477106152662131 ) ) ;
#5689 = CARTESIAN_POINT ( 'NONE',  ( -198.0356074513804572, 10.87444709759730088, -10.87444709759707173 ) ) ;
#5690 = CARTESIAN_POINT ( 'NONE',  ( -30.26275506840324070, -1.694272468446265112, 0.000000000000000000 ) ) ;
#5691 = CARTESIAN_POINT ( 'NONE',  ( 184.8905102610680444, -20.92133201514440799, 40.00000000000002132 ) ) ;
#5692 = CARTESIAN_POINT ( 'NONE',  ( -280.0000000000000568, -39.99999999999987210, -20.00000000000043343 ) ) ;
#5693 = CARTESIAN_POINT ( 'NONE',  ( 98.29820294267351244, -10.58389073158543958, 16.98253775142841704 ) ) ;
#5694 = CARTESIAN_POINT ( 'NONE',  ( -259.2033419157646676, 6.730120644403426944, 6.730120644403592145 ) ) ;
#5695 = ORIENTED_EDGE ( 'NONE', *, *, #24587, .F. ) ;
#5696 = CARTESIAN_POINT ( 'NONE',  ( 98.29820294267170766, 13.21553301702797789, -15.06873823044322869 ) ) ;
#5697 = CARTESIAN_POINT ( 'NONE',  ( -105.3755690713226869, 21.75974354311648540, -0.000000000000000000 ) ) ;
#5698 = CARTESIAN_POINT ( 'NONE',  ( -103.9650464695103551, -8.298274100672328402, 20.03380587528770462 ) ) ;
#5699 = PRODUCT_CONTEXT ( 'NONE', #16389, 'mechanical' ) ;
#5700 = ORIENTED_EDGE ( 'NONE', *, *, #12057, .T. ) ;
#5701 = ORIENTED_EDGE ( 'NONE', *, *, #25271, .T. ) ;
#5702 = CARTESIAN_POINT ( 'NONE',  ( -280.0000000000000568, -14.14213562373078226, -42.42640687119295251 ) ) ;
#5703 = CARTESIAN_POINT ( 'NONE',  ( 22.50777602749823814, -43.24633676485594691, -17.91321921096134417 ) ) ;
#5704 = ORIENTED_EDGE ( 'NONE', *, *, #5562, .T. ) ;
#5705 = CARTESIAN_POINT ( 'NONE',  ( 57.59792236341147031, -2.435789363418150000, -40.00000000000002132 ) ) ;
#5706 = B_SPLINE_CURVE_WITH_KNOTS ( 'NONE', 3,
 ( #12677, #2851, #14801, #17189, #18804, #7084, #25068, #3099, #19066, #23195, #15198, #4976 ),
 .UNSPECIFIED., .F., .F.,
 ( 4, 2, 2, 2, 2, 4 ),
 ( 5.597004042492164534E-17, 0.005971690550335823772, 0.008957535825503749535, 0.01045045846308766992, 0.01119691978187959194, 0.01194338110067151397 ),
 .UNSPECIFIED. ) ;
#5707 = FACE_OUTER_BOUND ( 'NONE', #4679, .T. ) ;
#5708 = EDGE_CURVE ( 'NONE', #14842, #19288, #16554, .T. ) ;
#5709 = ORIENTED_EDGE ( 'NONE', *, *, #8830, .F. ) ;
#5710 = CARTESIAN_POINT ( 'NONE',  ( 199.9999999999999716, 18.09021486607068496, 5.826594753398616433 ) ) ;
#5711 = DIRECTION ( 'NONE',  ( -0.3301743741156225598, 0.000000000000000000, -0.9439199556516204570 ) ) ;
#5712 = CARTESIAN_POINT ( 'NONE',  ( 91.82158438592158234, 16.11829626346139577, 16.11829626346143840 ) ) ;
#5713 = ADVANCED_FACE ( 'NONE', ( #22892 ), #6837, .T. ) ;
#5714 = SPHERICAL_SURFACE ( 'NONE', #9315, 15.00000000000000000 ) ;
#5715 = CARTESIAN_POINT ( 'NONE',  ( -30.26275506840324070, -1.147469862568086380E-14, 1.694272468446259783 ) ) ;
#5716 = CARTESIAN_POINT ( 'NONE',  ( 91.82158438592158234, -17.20528682183298486, 0.000000000000000000 ) ) ;
#5717 = CARTESIAN_POINT ( 'NONE',  ( 184.8905102610680444, 13.49065550809826952, -13.49065550809790359 ) ) ;
#5718 = CARTESIAN_POINT ( 'NONE',  ( -190.0000000000000284, -82.49999999999991473, -52.49999999999977973 ) ) ;
#5719 = EDGE_CURVE ( 'NONE', #21182, #22119, #21953, .T. ) ;
#5720 = ADVANCED_FACE ( 'NONE', ( #14161 ), #18148, .T. ) ;
#5721 = DIRECTION ( 'NONE',  ( 0.000000000000000000, 0.000000000000000000, 1.000000000000000000 ) ) ;
#5722 = CARTESIAN_POINT ( 'NONE',  ( 163.1118516004056573, -40.00000000000027711, 27.26290988616830546 ) ) ;
#5723 = CARTESIAN_POINT ( 'NONE',  ( -110.0471271032161553, -8.580892274476465076, 18.26740471935241672 ) ) ;
#5724 = CARTESIAN_POINT ( 'NONE',  ( -135.8532207217289738, -21.81201906317788186, 21.81201906317762962 ) ) ;
#5725 = CARTESIAN_POINT ( 'NONE',  ( -56.48582580120559982, 9.153146818113574668, -40.00000000000002132 ) ) ;
#5726 = CARTESIAN_POINT ( 'NONE',  ( -198.0356074513804572, -39.15871834505905724, -17.40982414986491733 ) ) ;
#5727 = CARTESIAN_POINT ( 'NONE',  ( -626.9846540392142060, 90.00000000000000000, 0.000000000000000000 ) ) ;
#5728 = CARTESIAN_POINT ( 'NONE',  ( -77.90255099906772784, 20.04994828523968664, -8.644468104261312291 ) ) ;
#5729 = DIRECTION ( 'NONE',  ( -1.000000000000000000, -1.836970198721030427E-16, 0.000000000000000000 ) ) ;
#5730 = CARTESIAN_POINT ( 'NONE',  ( -56.48582580120559271, 2.158176344243877536E-14, -9.153146818113587102 ) ) ;
#5731 = CARTESIAN_POINT ( 'NONE',  ( 19.06497207195980792, 66.60410523465817789, 10.03556273973446800 ) ) ;
#5732 = CARTESIAN_POINT ( 'NONE',  ( -105.3755690713226727, 15.38646221621771737, 15.38646221621800514 ) ) ;
#5733 = CARTESIAN_POINT ( 'NONE',  ( -188.2957210513761197, -13.82790368522227986, -46.98905903629284353 ) ) ;
#5734 = CARTESIAN_POINT ( 'NONE',  ( -259.2033419157646676, -21.55415060305824326, -35.01439189186556433 ) ) ;
#5735 = ORIENTED_EDGE ( 'NONE', *, *, #26147, .T. ) ;
#5736 = CARTESIAN_POINT ( 'NONE',  ( 136.1360204305621266, -24.77266263493151044, 24.77266263493093135 ) ) ;
#5737 = CARTESIAN_POINT ( 'NONE',  ( -208.1127848780265026, -10.60833733269551971, 10.60833733269537049 ) ) ;
#5738 = CARTESIAN_POINT ( 'NONE',  ( -190.0000000000000000, -71.50000000000002842, 66.50000000000005684 ) ) ;
#5739 = DIRECTION ( 'NONE',  ( 0.3301743741186746739, 0.9439199556505528665, 0.000000000000000000 ) ) ;
#5740 = CARTESIAN_POINT ( 'NONE',  ( 170.2234770963711128, -45.64576402573167258, -10.92277846919254891 ) ) ;
#5741 = CARTESIAN_POINT ( 'NONE',  ( 73.43374839995014725, -26.88865971588853299, 12.96823619005398420 ) ) ;
#5742 = AXIS2_PLACEMENT_3D ( 'NONE', #3908, #24654, #8404 ) ;
#5743 = ORIENTED_EDGE ( 'NONE', *, *, #23766, .T. ) ;
#5744 = CARTESIAN_POINT ( 'NONE',  ( 199.9999999999999432, 18.09516392985831601, -5.803866375870236460 ) ) ;
#5745 = CARTESIAN_POINT ( 'NONE',  ( 23.09861257792919176, -23.40165480222906069, 42.94075326233394918 ) ) ;
#5746 = CARTESIAN_POINT ( 'NONE',  ( -4.201409602820223910, 23.41774994521163222, 42.95750343186378473 ) ) ;
#5747 = EDGE_LOOP ( 'NONE', ( #1376, #23519, #3680, #15738, #16613, #24918, #22384, #22123 ) ) ;
#5748 = EDGE_LOOP ( 'NONE', ( #7100, #1497 ) ) ;
#5749 = EDGE_CURVE ( 'NONE', #9443, #10429, #17877, .T. ) ;
#5750 = CARTESIAN_POINT ( 'NONE',  ( -208.1127848780264742, 15.00245453012665742, -40.00000000000002132 ) ) ;
#5751 = CARTESIAN_POINT ( 'NONE',  ( -162.0762913951020892, -1.198031840385783919, 1.198031840385741731 ) ) ;
#5752 = CARTESIAN_POINT ( 'NONE',  ( 19.06497207195979726, 39.99999999999997158, 14.19242893257854554 ) ) ;
#5753 = DIRECTION ( 'NONE',  ( 1.000000000000000000, -0.000000000000000000, -0.000000000000000000 ) ) ;
#5754 = EDGE_CURVE ( 'NONE', #19908, #16682, #24077, .T. ) ;
#5755 = DIRECTION ( 'NONE',  ( 0.7071067811865441310, -0.7071067811865507924, 8.659560562354974766E-17 ) ) ;
#5756 = FACE_OUTER_BOUND ( 'NONE', #10224, .T. ) ;
#5757 = CARTESIAN_POINT ( 'NONE',  ( 200.0000000000000568, -15.63904601878861733, 10.81246610429574595 ) ) ;
#5758 = CIRCLE ( 'NONE', #15941, 30.00000000000000355 ) ;
#5759 = CIRCLE ( 'NONE', #1104, 15.00000000000000533 ) ;
#5760 = CARTESIAN_POINT ( 'NONE',  ( 199.0140795438509826, 16.43701665320993044, 11.39707250661459348 ) ) ;
#5761 = CARTESIAN_POINT ( 'NONE',  ( -144.0562564038984021, 10.50946916234533468, 31.27039870030377244 ) ) ;
#5762 = CARTESIAN_POINT ( 'NONE',  ( -4.260882601031005912, -13.81249720866826358, -46.91379881627400295 ) ) ;
#5763 = CARTESIAN_POINT ( 'NONE',  ( -91.56559293963834989, -12.25131212657475466, -12.25131212657495361 ) ) ;
#5764 = DIRECTION ( 'NONE',  ( 0.000000000000000000, -1.000000000000000000, 0.000000000000000000 ) ) ;
#5765 = CARTESIAN_POINT ( 'NONE',  ( 0.2972598230770027716, -38.42060263243656237, -18.14793986248737667 ) ) ;
#5766 = CARTESIAN_POINT ( 'NONE',  ( -105.3755690713226727, -2.472783935621397949E-13, 21.75974354311649961 ) ) ;
#5767 = DIRECTION ( 'NONE',  ( 0.000000000000000000, 0.000000000000000000, 1.000000000000000000 ) ) ;
#5768 = CARTESIAN_POINT ( 'NONE',  ( -208.1127848780265026, -10.60833733269537227, -10.60833733269551793 ) ) ;
#5769 = CARTESIAN_POINT ( 'NONE',  ( -162.0762913951020607, -41.69427287682838568, -2.449293598294708485E-15 ) ) ;
#5770 = VECTOR ( 'NONE', #24556, 1000.000000000000000 ) ;
#5771 = CARTESIAN_POINT ( 'NONE',  ( -259.2033419157646676, 35.01439189186528722, 21.55415060305857011 ) ) ;
#5772 = CARTESIAN_POINT ( 'NONE',  ( -56.48582580120557850, -30.84685318188645198, -2.449293598294708485E-15 ) ) ;
#5773 = CARTESIAN_POINT ( 'NONE',  ( -110.0968994563038450, 12.50898707784705088, 15.90535099103004768 ) ) ;
#5774 = VECTOR ( 'NONE', #11426, 1000.000000000000000 ) ;
#5775 = CARTESIAN_POINT ( 'NONE',  ( 4.995406935893290878, 1.606505379428369110E-13, -15.24977328854832592 ) ) ;
#5776 = CARTESIAN_POINT ( 'NONE',  ( 136.1360204305621551, 3.511608612530801032, -53.05693388239316022 ) ) ;
#5777 = CARTESIAN_POINT ( 'NONE',  ( 192.4448373802101173, -20.00000000003938538, -40.00000000000002132 ) ) ;
#5778 = ORIENTED_EDGE ( 'NONE', *, *, #8487, .T. ) ;
#5779 = CARTESIAN_POINT ( 'NONE',  ( 23.42154907652890472, -42.84253412640328662, 23.32998349128528304 ) ) ;
#5780 = AXIS2_PLACEMENT_3D ( 'NONE', #23440, #21567, #713 ) ;
#5781 = CARTESIAN_POINT ( 'NONE',  ( 133.2080217031554810, 12.38638889282702671, 29.90338805389126264 ) ) ;
#5782 = CARTESIAN_POINT ( 'NONE',  ( 14.38125909742180220, 39.01709431150916885, -17.55144818341463164 ) ) ;
#5783 = CARTESIAN_POINT ( 'NONE',  ( 200.0000000000000000, -39.99999999999991473, -20.00000000000024514 ) ) ;
#5784 = CARTESIAN_POINT ( 'NONE',  ( -162.0762913951020892, 1.198031840385732849, -1.198031840385733515 ) ) ;
#5785 = CARTESIAN_POINT ( 'NONE',  ( -135.8532207217289738, -9.153146818113595984, 0.000000000000000000 ) ) ;
#5786 = CARTESIAN_POINT ( 'NONE',  ( 151.7948205124836534, 6.767089262349062828, -40.00000000000002132 ) ) ;
#5787 = CARTESIAN_POINT ( 'NONE',  ( 170.0000000000000000, 24.95097643317004099, -3.062538285713088282 ) ) ;
#5788 = CARTESIAN_POINT ( 'NONE',  ( 199.9999999999999147, 19.00141375156598045, 0.3223421948013435179 ) ) ;
#5789 = CARTESIAN_POINT ( 'NONE',  ( 199.9999999999999432, -18.37296950073040236, 4.918342949125168673 ) ) ;
#5790 = CARTESIAN_POINT ( 'NONE',  ( -100.7734535825088358, 12.25131212657497848, -12.25131212657469604 ) ) ;
#5791 = CARTESIAN_POINT ( 'NONE',  ( -86.96347745069645896, -12.89780903124443689, 43.67073346367968156 ) ) ;
#5792 = CARTESIAN_POINT ( 'NONE',  ( -105.2302824411781330, 21.33128297465077594, -2.585500233827331851 ) ) ;
#5793 = CARTESIAN_POINT ( 'NONE',  ( -87.10570614286989155, 13.14378919785584010, -16.99508527299807170 ) ) ;
#5794 = CARTESIAN_POINT ( 'NONE',  ( 200.0000000000000000, 14.14213562373142352, -42.42640687119268961 ) ) ;
#5795 = CIRCLE ( 'NONE', #20687, 60.00000000000000000 ) ;
#5797 = CARTESIAN_POINT ( 'NONE',  ( -86.86493150571111244, 8.366608963953098055, -19.60045294882791467 ) ) ;
#5796 = CARTESIAN_POINT ( 'NONE',  ( 199.9999999999999432, -14.14213562373073607, -14.14213562373102206 ) ) ;
#5798 = CARTESIAN_POINT ( 'NONE',  ( -135.8532207217289738, -6.472252184284280396, 6.472252184284099208 ) ) ;
#5799 = CARTESIAN_POINT ( 'NONE',  ( 130.8568914410475372, -34.05028731879786363, 0.000000000000000000 ) ) ;
#5800 = CARTESIAN_POINT ( 'NONE',  ( 199.0233480856092001, 0.0005622888856919192003, 20.00362916157371629 ) ) ;
#5802 = CARTESIAN_POINT ( 'NONE',  ( 163.1118516004056573, -39.99999999999990052, -27.26290988616886679 ) ) ;
#5801 = CARTESIAN_POINT ( 'NONE',  ( 91.82158438592158234, -12.16597498397778843, 12.16597498397750954 ) ) ;
#5803 = CARTESIAN_POINT ( 'NONE',  ( 200.0000000000000000, 42.42640687119290988, 14.14213562373111976 ) ) ;
#5804 = CARTESIAN_POINT ( 'NONE',  ( -162.0762913951020892, 1.198031840385732849, -1.198031840385733515 ) ) ;
#5805 = CARTESIAN_POINT ( 'NONE',  ( 200.0000000000000000, 19.99999999999995737, 40.00000000000002132 ) ) ;
#5807 = EDGE_CURVE ( 'NONE', #2026, #12388, #20258, .T. ) ;
#5806 = VERTEX_POINT ( 'NONE', #12297 ) ;
#5808 = CARTESIAN_POINT ( 'NONE',  ( 1.564253033640332413, -24.39614062124443450, -44.28527310957341712 ) ) ;
#5809 = AXIS2_PLACEMENT_3D ( 'NONE', #11605, #1386, #1515 ) ;
#5810 = CARTESIAN_POINT ( 'NONE',  ( 12.71631587212106140, 43.65709841108841260, 18.08336225573125944 ) ) ;
#5811 = CARTESIAN_POINT ( 'NONE',  ( 27.55177309534125385, 22.48880744263714959, 41.56868263113059925 ) ) ;
#5812 = CARTESIAN_POINT ( 'NONE',  ( 4.995406935893288214, 15.24977328854832770, 0.000000000000000000 ) ) ;
#5813 = ORIENTED_EDGE ( 'NONE', *, *, #15793, .T. ) ;
#5814 = CARTESIAN_POINT ( 'NONE',  ( -188.9478457324744056, -43.31767415847494362, 17.94276812689867029 ) ) ;
#5815 = B_SPLINE_CURVE_WITH_KNOTS ( 'NONE', 3,
 ( #11782, #3411, #9658, #1170, #23632, #19762, #13770, #17892, #23887, #1553 ),
 .UNSPECIFIED., .F., .F.,
 ( 4, 2, 2, 2, 4 ),
 ( 0.7921542097164249174, 0.8508620842112317728, 0.8814014469398914198, 0.9119408096685510667, 0.9406682828395580565 ),
 .UNSPECIFIED. ) ;
#5816 = CARTESIAN_POINT ( 'NONE',  ( 200.0000000000000853, -18.58433719308212773, 4.010382776060092525 ) ) ;
#5817 = CARTESIAN_POINT ( 'NONE',  ( 8.556015491684524576, -14.17785852676789560, 49.31947911770178195 ) ) ;
#5818 = ADVANCED_FACE ( 'NONE', ( #2070 ), #17015, .T. ) ;
#5819 = ADVANCED_FACE ( 'NONE', ( #11118 ), #18842, .T. ) ;
#5820 = CARTESIAN_POINT ( 'NONE',  ( 23.35928221536259386, 13.80178577956188768, -46.81377789283278190 ) ) ;
#5821 = CARTESIAN_POINT ( 'NONE',  ( 199.0163032586025622, -14.59919991228128922, -13.67396374720910757 ) ) ;
#5822 = CARTESIAN_POINT ( 'NONE',  ( -716.9846540392142060, 52.49999999999991473, -82.49999999999998579 ) ) ;
#5823 = CARTESIAN_POINT ( 'NONE',  ( -183.6285492669661323, -17.34367427885804247, 41.87133366546909485 ) ) ;
#5824 = CIRCLE ( 'NONE', #15112, 15.00000000000000000 ) ;
#5825 = CARTESIAN_POINT ( 'NONE',  ( 130.8568914410475088, 32.49135343045448820, 24.07718906446946860 ) ) ;
#5826 = CARTESIAN_POINT ( 'NONE',  ( -100.7734535825088500, -17.32597176626813251, 40.00000000000002132 ) ) ;
#5828 = CARTESIAN_POINT ( 'NONE',  ( -280.0000000000000000, -14.14213562373118549, 14.14213562373078936 ) ) ;
#5827 = DIRECTION ( 'NONE',  ( 0.000000000000000000, 0.000000000000000000, 1.000000000000000000 ) ) ;
#5829 = CARTESIAN_POINT ( 'NONE',  ( -30.26275506840324070, -1.694272468446265112, 0.000000000000000000 ) ) ;
#5830 = CARTESIAN_POINT ( 'NONE',  ( 192.4448373802100889, 20.00000000003945644, 0.000000000000000000 ) ) ;
#5831 = CARTESIAN_POINT ( 'NONE',  ( -86.96347745069644475, -21.75974354311652093, 40.00000000000002132 ) ) ;
#5832 = CARTESIAN_POINT ( 'NONE',  ( -192.9588430854689989, 5.375290060580374156E-13, -54.46834944099972375 ) ) ;
#5833 = CARTESIAN_POINT ( 'NONE',  ( -198.0356074513804572, 1.247057299367198800E-13, -15.37879056873070560 ) ) ;
#5834 = CARTESIAN_POINT ( 'NONE',  ( -86.96347745069644475, 15.38646221621772092, 15.38646221621800336 ) ) ;
#5835 = EDGE_LOOP ( 'NONE', ( #16879, #24612, #16683, #7471, #4991 ) ) ;
#5836 = CARTESIAN_POINT ( 'NONE',  ( 200.0000000000000000, 7.347880794884121511E-14, 0.000000000000000000 ) ) ;
#5837 = CARTESIAN_POINT ( 'NONE',  ( -91.56559293963836410, 22.67402823373189946, -0.000000000000000000 ) ) ;
#5838 = CARTESIAN_POINT ( 'NONE',  ( -192.1166648175281182, 48.16216898722869644, -14.00295691731063030 ) ) ;
#5839 = SHAPE_DEFINITION_REPRESENTATION ( #4036, #9131 ) ;
#5840 = EDGE_LOOP ( 'NONE', ( #10170, #12344, #11680, #5700 ) ) ;
#5841 = VERTEX_POINT ( 'NONE', #11238 ) ;
#5842 = CARTESIAN_POINT ( 'NONE',  ( -213.1075012329537230, -37.98287015391232302, -18.58567234101164800 ) ) ;
#5843 = CARTESIAN_POINT ( 'NONE',  ( 23.39921416754908279, -46.79910576274356515, -13.79910252519598934 ) ) ;
#5844 = ORIENTED_EDGE ( 'NONE', *, *, #9776, .F. ) ;
#5845 = CARTESIAN_POINT ( 'NONE',  ( 91.82158438592158234, -17.20528682183298486, -40.00000000000002132 ) ) ;
#5846 = CARTESIAN_POINT ( 'NONE',  ( 170.0000000000000000, 1.183443619805854272E-13, -24.95097643317000546 ) ) ;
#5847 = ORIENTED_EDGE ( 'NONE', *, *, #14110, .T. ) ;
#5848 = CARTESIAN_POINT ( 'NONE',  ( 199.9999999999999432, 16.89472078740815775, 8.702431973737679627 ) ) ;
#5849 = CARTESIAN_POINT ( 'NONE',  ( -105.2054292635175727, 21.49321519473981823, -0.6786951374309612151 ) ) ;
#5850 = CARTESIAN_POINT ( 'NONE',  ( -238.4067589809705794, 0.6820004457912757223, 0.6820004457913219076 ) ) ;
#5851 = CARTESIAN_POINT ( 'NONE',  ( -189.5227851116976581, -43.46196956062707528, -18.00253723946215700 ) ) ;
#5852 = CARTESIAN_POINT ( 'NONE',  ( -30.26275506840323359, -40.00000000000017053, 41.69427246844613677 ) ) ;
#5853 = CARTESIAN_POINT ( 'NONE',  ( -105.3755690713226585, 18.24025645688349684, 40.00000000000002132 ) ) ;
#5854 = CARTESIAN_POINT ( 'NONE',  ( 151.7948205124836534, -23.49921654115981084, -33.06932595376387951 ) ) ;
#5855 = CARTESIAN_POINT ( 'NONE',  ( -114.4364955367314991, -8.644468109207263495, -20.04994829327655737 ) ) ;
#5856 = CARTESIAN_POINT ( 'NONE',  ( 19.06497207195981858, -40.00000000000007105, 14.19242893257826665 ) ) ;
#5857 = CARTESIAN_POINT ( 'NONE',  ( -100.7734535825088500, -40.00000000000027711, 22.67402823373149801 ) ) ;
#5858 = FACE_BOUND ( 'NONE', #21745, .T. ) ;
#5859 = CARTESIAN_POINT ( 'NONE',  ( -135.8532207217289738, 6.472252184283881604, 50.09629031063969506 ) ) ;
#5860 = CARTESIAN_POINT ( 'NONE',  ( 19.06497207195981503, -14.19242893257840166, 0.000000000000000000 ) ) ;
#5861 = CARTESIAN_POINT ( 'NONE',  ( 200.0000000000000000, -14.14213562373062949, -42.42640687119301646 ) ) ;
#5862 = DIRECTION ( 'NONE',  ( -1.000000000000000000, -0.000000000000000000, -0.000000000000000000 ) ) ;
#5863 = ADVANCED_FACE ( 'NONE', ( #8596 ), #8726, .F. ) ;
#5864 = DIRECTION ( 'NONE',  ( 0.000000000000000000, -4.182618615277681568E-16, 1.000000000000000000 ) ) ;
#5865 = CARTESIAN_POINT ( 'NONE',  ( -280.0000000000000000, -2.609240458947769655E-13, 20.00000000000001421 ) ) ;
#5866 = CARTESIAN_POINT ( 'NONE',  ( 200.0000000000000000, -39.99999999999991473, -20.00000000000024514 ) ) ;
#5867 = CARTESIAN_POINT ( 'NONE',  ( 146.6084372240433709, 32.08495691632064961, -24.48358557860320417 ) ) ;
#5868 = CARTESIAN_POINT ( 'NONE',  ( -114.4364955367322949, 8.644468109217019247, 20.04994829327305794 ) ) ;
#5869 = CARTESIAN_POINT ( 'NONE',  ( -188.3066136396996058, -23.45085387054324144, -43.00728998844858353 ) ) ;
#5870 = CARTESIAN_POINT ( 'NONE',  ( -162.0762913951020892, -1.198031840385783919, 1.198031840385741731 ) ) ;
#5871 = ORIENTED_EDGE ( 'NONE', *, *, #15011, .F. ) ;
#5872 = CARTESIAN_POINT ( 'NONE',  ( 14.38125909742181285, -17.55144818341421598, -39.01709431150935359 ) ) ;
#5873 = FACE_OUTER_BOUND ( 'NONE', #18229, .T. ) ;
#5874 = CARTESIAN_POINT ( 'NONE',  ( 19.06497207195981147, -10.03556273973439517, 10.03556273973429214 ) ) ;
#5875 = LINE ( 'NONE', #15974, #2186 ) ;
#5876 =( BOUNDED_SURFACE ( )  B_SPLINE_SURFACE ( 3, 3, ( 
 ( #16605, #8220, #22609, #5969, #22476, #18467, #10492, #8491, #20076, #24339, #4386, #6103, #4515, #10225, #1853, #113, #14080, #10355, #2380, #14210, #18064, #18333, #12085, #24199, #20207, #22344, #24467, #16338, #20474, #12217 ),
 ( #7951, #14348, #9957, #24738, #2116, #2248, #18194, #14606, #18605, #1985, #6494, #4123, #22735, #20339, #6233, #26215, #16069, #4255, #12345, #12478, #22211, #20604, #384, #24604, #245, #3986, #6357, #8357, #10090, #16478 ),
 ( #26346, #8626, #11024, #16737, #25139, #19134, #16875, #25007, #7148, #6760, #17003, #14872, #2656, #21141, #4785, #3041, #12616, #8892, #787, #12888, #19010, #23007, #21003, #4649, #12752, #6890, #2916, #15006, #521, #23139 ),
 ( #4910, #2785, #917, #20873, #10898, #15264, #13022, #9029, #24869, #17133, #25266, #7016, #15137, #23267, #5043, #6624, #13150, #23393, #21268, #18873, #11149, #19263, #20744, #1044, #10761, #9147, #17262, #18739, #25397, #2513 ),
 ( #10628, #14741, #22872, #653, #8760, #21519, #19643, #17901, #23895, #11271, #11389, #3168, #21643, #19391, #1296, #17386, #11648, #19909, #3681, #7652, #9278, #13273, #1176, #5168, #21395, #23638, #1427, #7396, #25525, #25778 ),
 ( #9405, #15509, #1693, #7274, #15767, #5671, #15390, #23513, #5287, #26048, #21907, #19511, #3416, #13394, #5416, #7528, #17511, #17769, #15636, #13518, #3293, #15901, #7785, #11789, #25650, #9797, #13777, #11518, #25911, #9527 ),
 ( #17635, #19771, #23761, #5542, #13649, #21774, #3547, #1560, #9665, #14181, #16449, #14452, #24168, #10198, #7925, #24574, #5943, #14051, #11924, #20445, #18440, #12450, #18171, #6330, #22579, #3822, #1826, #13914, #88, #16177 ) ),
 .UNSPECIFIED., .T., .F., .F. ) 
 B_SPLINE_SURFACE_WITH_KNOTS ( ( 4, 3, 4 ),
 ( 4, 2, 2, 2, 2, 2, 2, 2, 2, 2, 2, 2, 2, 2, 4 ),
 ( 0.000000000000000000, 0.5000000000000000000, 1.000000000000000000 ),
 ( 0.000000000000000000, 0.1357259735107005372, 0.1651108541090157700, 0.1944957347073310028, 0.3598804999793158710, 0.3867117631979620773, 0.4135430264166082281, 0.5789277916885930964, 0.6062785021374117456, 0.6336292125862302838, 0.8508620842112317728, 0.8814014469398914198, 0.9119408096685510667, 0.9559704048342755334, 1.000000000000000000 ),
 .UNSPECIFIED. ) 
 GEOMETRIC_REPRESENTATION_ITEM ( )  RATIONAL_B_SPLINE_SURFACE ( (
 ( 1.000000000000000000, 1.000000000000000000, 1.000000000000000000, 1.000000000000000000, 1.000000000000000000, 1.000000000000000000, 1.000000000000000000, 1.000000000000000000, 1.000000000000000000, 1.000000000000000000, 1.000000000000000000, 1.000000000000000000, 1.000000000000000000, 1.000000000000000000, 1.000000000000000000, 1.000000000000000000, 1.000000000000000000, 1.000000000000000000, 1.000000000000000000, 1.000000000000000000, 1.000000000000000000, 1.000000000000000000, 1.000000000000000000, 1.000000000000000000, 1.000000000000000000, 1.000000000000000000, 1.000000000000000000, 1.000000000000000000, 1.000000000000000000, 1.000000000000000000),
 ( 0.3333333333333333703, 0.3333333333333333703, 0.3333333333333333703, 0.3333333333333333703, 0.3333333333333333703, 0.3333333333333333703, 0.3333333333333333703, 0.3333333333333333703, 0.3333333333333333703, 0.3333333333333333703, 0.3333333333333333703, 0.3333333333333333703, 0.3333333333333333703, 0.3333333333333333703, 0.3333333333333333703, 0.3333333333333333703, 0.3333333333333333703, 0.3333333333333333703, 0.3333333333333333703, 0.3333333333333333703, 0.3333333333333333703, 0.3333333333333333703, 0.3333333333333333703, 0.3333333333333333703, 0.3333333333333333703, 0.3333333333333333703, 0.3333333333333333703, 0.3333333333333333703, 0.3333333333333333703, 0.3333333333333333703),
 ( 0.3333333333333333703, 0.3333333333333333703, 0.3333333333333333703, 0.3333333333333333703, 0.3333333333333333703, 0.3333333333333333703, 0.3333333333333333703, 0.3333333333333333703, 0.3333333333333333703, 0.3333333333333333703, 0.3333333333333333703, 0.3333333333333333703, 0.3333333333333333703, 0.3333333333333333703, 0.3333333333333333703, 0.3333333333333333703, 0.3333333333333333703, 0.3333333333333333703, 0.3333333333333333703, 0.3333333333333333703, 0.3333333333333333703, 0.3333333333333333703, 0.3333333333333333703, 0.3333333333333333703, 0.3333333333333333703, 0.3333333333333333703, 0.3333333333333333703, 0.3333333333333333703, 0.3333333333333333703, 0.3333333333333333703),
 ( 1.000000000000000000, 1.000000000000000000, 1.000000000000000000, 1.000000000000000000, 1.000000000000000000, 1.000000000000000000, 1.000000000000000000, 1.000000000000000000, 1.000000000000000000, 1.000000000000000000, 1.000000000000000000, 1.000000000000000000, 1.000000000000000000, 1.000000000000000000, 1.000000000000000000, 1.000000000000000000, 1.000000000000000000, 1.000000000000000000, 1.000000000000000000, 1.000000000000000000, 1.000000000000000000, 1.000000000000000000, 1.000000000000000000, 1.000000000000000000, 1.000000000000000000, 1.000000000000000000, 1.000000000000000000, 1.000000000000000000, 1.000000000000000000, 1.000000000000000000),
 ( 0.3333333333333333703, 0.3333333333333333703, 0.3333333333333333703, 0.3333333333333333703, 0.3333333333333333703, 0.3333333333333333703, 0.3333333333333333703, 0.3333333333333333703, 0.3333333333333333703, 0.3333333333333333703, 0.3333333333333333703, 0.3333333333333333703, 0.3333333333333333703, 0.3333333333333333703, 0.3333333333333333703, 0.3333333333333333703, 0.3333333333333333703, 0.3333333333333333703, 0.3333333333333333703, 0.3333333333333333703, 0.3333333333333333703, 0.3333333333333333703, 0.3333333333333333703, 0.3333333333333333703, 0.3333333333333333703, 0.3333333333333333703, 0.3333333333333333703, 0.3333333333333333703, 0.3333333333333333703, 0.3333333333333333703),
 ( 0.3333333333333333703, 0.3333333333333333703, 0.3333333333333333703, 0.3333333333333333703, 0.3333333333333333703, 0.3333333333333333703, 0.3333333333333333703, 0.3333333333333333703, 0.3333333333333333703, 0.3333333333333333703, 0.3333333333333333703, 0.3333333333333333703, 0.3333333333333333703, 0.3333333333333333703, 0.3333333333333333703, 0.3333333333333333703, 0.3333333333333333703, 0.3333333333333333703, 0.3333333333333333703, 0.3333333333333333703, 0.3333333333333333703, 0.3333333333333333703, 0.3333333333333333703, 0.3333333333333333703, 0.3333333333333333703, 0.3333333333333333703, 0.3333333333333333703, 0.3333333333333333703, 0.3333333333333333703, 0.3333333333333333703),
 ( 1.000000000000000000, 1.000000000000000000, 1.000000000000000000, 1.000000000000000000, 1.000000000000000000, 1.000000000000000000, 1.000000000000000000, 1.000000000000000000, 1.000000000000000000, 1.000000000000000000, 1.000000000000000000, 1.000000000000000000, 1.000000000000000000, 1.000000000000000000, 1.000000000000000000, 1.000000000000000000, 1.000000000000000000, 1.000000000000000000, 1.000000000000000000, 1.000000000000000000, 1.000000000000000000, 1.000000000000000000, 1.000000000000000000, 1.000000000000000000, 1.000000000000000000, 1.000000000000000000, 1.000000000000000000, 1.000000000000000000, 1.000000000000000000, 1.000000000000000000) ) ) 
 REPRESENTATION_ITEM ( '' )  SURFACE ( )  );
#5877 = DIRECTION ( 'NONE',  ( 1.000000000000000000, 1.836970198721030181E-16, -0.000000000000000000 ) ) ;
#5878 = CARTESIAN_POINT ( 'NONE',  ( -198.0356074513804572, 10.87444709761036066, -67.44298959253325165 ) ) ;
#5879 = CARTESIAN_POINT ( 'NONE',  ( -87.11136440740810372, 2.379156564867217494, 21.34823163554904824 ) ) ;
#5880 = ORIENTED_EDGE ( 'NONE', *, *, #6304, .T. ) ;
#5881 = CARTESIAN_POINT ( 'NONE',  ( 199.9999999999999716, 18.70042687752384936, -3.380346622114776434 ) ) ;
#5882 = CARTESIAN_POINT ( 'NONE',  ( 23.37394308801977871, -23.33966569535098046, 42.85717664514577763 ) ) ;
#5883 = CARTESIAN_POINT ( 'NONE',  ( -4.580761711670050751, 17.81010960708292501, 42.99740816077149930 ) ) ;
#5884 = ORIENTED_EDGE ( 'NONE', *, *, #9469, .F. ) ;
#5885 = VERTEX_POINT ( 'NONE', #18976 ) ;
#5886 = CARTESIAN_POINT ( 'NONE',  ( 0.2972598230769930572, 14.33493731733933352, 0.000000000000000000 ) ) ;
#5887 = CARTESIAN_POINT ( 'NONE',  ( 199.0093721751683518, -2.288394243462712030, -19.86801947894618792 ) ) ;
#5888 = FACE_OUTER_BOUND ( 'NONE', #17196, .T. ) ;
#5889 =( LENGTH_UNIT ( ) NAMED_UNIT ( * ) SI_UNIT ( .MILLI., .METRE. ) );
#5890 = VECTOR ( 'NONE', #24298, 1000.000000000000000 ) ;
#5891 = CARTESIAN_POINT ( 'NONE',  ( -1.821043593238388603, 43.61003463695197269, -23.89737153267502023 ) ) ;
#5892 = CARTESIAN_POINT ( 'NONE',  ( -280.0000000000000568, 39.99999999999976552, 20.00000000000043343 ) ) ;
#5893 = CARTESIAN_POINT ( 'NONE',  ( 98.29820294267362613, 4.524526698164271110, -19.49240851342956660 ) ) ;
#5894 = CARTESIAN_POINT ( 'NONE',  ( -636.9184764937167529, 28.24694889380673501, -28.32469577109011283 ) ) ;
#5895 = CARTESIAN_POINT ( 'NONE',  ( 190.0000000000000000, -52.49999999999970868, 82.49999999999998579 ) ) ;
#5896 = CARTESIAN_POINT ( 'NONE',  ( 199.0198237862232133, 7.937771492746675150, 18.36232769351375538 ) ) ;
#5897 = CARTESIAN_POINT ( 'NONE',  ( -166.7090608782836227, 15.35183551246269928, 37.06260950135659726 ) ) ;
#5898 = CARTESIAN_POINT ( 'NONE',  ( 5.823571940223811083, -14.15488761396733608, -49.16771748718979751 ) ) ;
#5899 = CARTESIAN_POINT ( 'NONE',  ( -259.2033419157646676, -21.55415060305824326, -21.55415060305857367 ) ) ;
#5900 = EDGE_CURVE ( 'NONE', #2387, #11822, #25107, .T. ) ;
#5901 = CYLINDRICAL_SURFACE ( 'NONE', #2947, 5.000000000000004441 ) ;
#5902 = CARTESIAN_POINT ( 'NONE',  ( 19.06497207195982924, -66.60410523465823474, 10.03556273973400081 ) ) ;
#5903 = CARTESIAN_POINT ( 'NONE',  ( -91.56559293963834989, -40.00000000000027711, 22.67402823373149801 ) ) ;
#5904 = CARTESIAN_POINT ( 'NONE',  ( 136.1360204305621266, 35.03383547441298873, 0.000000000000000000 ) ) ;
#5905 = CARTESIAN_POINT ( 'NONE',  ( -280.0000000000000568, -20.00000000000007105, 40.00000000000002132 ) ) ;
#5906 = CARTESIAN_POINT ( 'NONE',  ( 199.9999999999999432, 14.14213562373113398, -14.14213562373094923 ) ) ;
#5907 = CARTESIAN_POINT ( 'NONE',  ( -135.8532207217289454, -30.84685318188649106, 40.00000000000002132 ) ) ;
#5908 = CARTESIAN_POINT ( 'NONE',  ( -110.0368417077421128, 7.992411109433636973, 18.51665893310612532 ) ) ;
#5909 = CARTESIAN_POINT ( 'NONE',  ( 151.7948205124836534, 39.99999999999970157, 33.23291073765595627 ) ) ;
#5910 = EDGE_CURVE ( 'NONE', #9153, #5885, #12571, .T. ) ;
#5911 = CARTESIAN_POINT ( 'NONE',  ( 57.59792236341147031, -1.722363176415032004, -1.722363176415048880 ) ) ;
#5912 = ADVANCED_FACE ( 'NONE', ( #25747 ), #9499, .F. ) ;
#5913 = CARTESIAN_POINT ( 'NONE',  ( -198.0356074513804572, 15.37879056873067007, 0.000000000000000000 ) ) ;
#5915 = ORIENTED_EDGE ( 'NONE', *, *, #21658, .F. ) ;
#5914 = AXIS2_PLACEMENT_3D ( 'NONE', #24827, #8445, #16564 ) ;
#5916 = CARTESIAN_POINT ( 'NONE',  ( -105.3755690713226727, -21.75974354311652093, 0.000000000000000000 ) ) ;
#5917 = CIRCLE ( 'NONE', #19504, 5.000000000000004441 ) ;
#5918 = CARTESIAN_POINT ( 'NONE',  ( -220.0000000000000284, 66.50000000000001421, -66.50000000000005684 ) ) ;
#5919 = CARTESIAN_POINT ( 'NONE',  ( -91.56559293963834989, 40.53558337403677569, -16.03295912088699993 ) ) ;
#5920 = CARTESIAN_POINT ( 'NONE',  ( -213.1075012329537230, -2.291445344039133686E-13, 53.71589010951915100 ) ) ;
#5921 = CARTESIAN_POINT ( 'NONE',  ( -91.56559293963834989, -16.03295912088728414, 16.03295912088688269 ) ) ;
#5922 = CARTESIAN_POINT ( 'NONE',  ( -280.0000000000000000, -20.00000000000006750, 0.000000000000000000 ) ) ;
#5923 = CARTESIAN_POINT ( 'NONE',  ( -208.1127848780264742, 15.00245453012665742, -40.00000000000002132 ) ) ;
#5924 = PRODUCT_DEFINITION_SHAPE ( 'NONE', 'NONE',  #26361 ) ;
#5925 = CARTESIAN_POINT ( 'NONE',  ( -200.0000000000000000, 61.50000000000009237, -66.50000000000005684 ) ) ;
#5926 = CARTESIAN_POINT ( 'NONE',  ( 200.0000000000000000, 17.99290950227088004, 6.120759354987654000 ) ) ;
#5927 = CARTESIAN_POINT ( 'NONE',  ( 199.9999999999999147, -17.05647522489845969, -8.409730364717644235 ) ) ;
#5928 = CARTESIAN_POINT ( 'NONE',  ( 57.59792236341147031, 26.56190807104720975, -26.56190807104655249 ) ) ;
#5929 = CARTESIAN_POINT ( 'NONE',  ( 91.82158438592159655, -16.11829626346125011, -16.11829626346154853 ) ) ;
#5930 = CARTESIAN_POINT ( 'NONE',  ( 0.2972598230769976091, -10.13633138497479180, 10.13633138497468522 ) ) ;
#5931 = CARTESIAN_POINT ( 'NONE',  ( 180.0000000000000284, -135.7889608577475258, 82.50000000000001421 ) ) ;
#5932 = CARTESIAN_POINT ( 'NONE',  ( 91.82158438592159655, -44.40256751092341858, 12.16597498400012434 ) ) ;
#5933 = DIRECTION ( 'NONE',  ( 4.657398277317546459E-32, -1.682156097916904081E-16, -1.000000000000000000 ) ) ;
#5934 = CARTESIAN_POINT ( 'NONE',  ( -213.1075012329537230, -18.58567234101102272, -37.98287015391260013 ) ) ;
#5935 = CARTESIAN_POINT ( 'NONE',  ( -238.4067589809705794, -28.96627169325313389, -27.60227080167074831 ) ) ;
#5936 = CARTESIAN_POINT ( 'NONE',  ( 199.0195099801769061, 8.518539848973487594, 18.09882726175286649 ) ) ;
#5938 = CARTESIAN_POINT ( 'NONE',  ( 170.2234770963711128, -39.99999999999991473, -24.55285855007201334 ) ) ;
#5937 = CARTESIAN_POINT ( 'NONE',  ( 130.8568914410475372, 4.207082182992923691, -4.207082182992794017 ) ) ;
#5939 = CARTESIAN_POINT ( 'NONE',  ( 0.2972598230769938343, 10.13633138497486286, -10.13633138497461594 ) ) ;
#5940 = CARTESIAN_POINT ( 'NONE',  ( -3.406542234095620625, 43.31371932780143652, -17.94112998239643630 ) ) ;
#5941 = CARTESIAN_POINT ( 'NONE',  ( -56.48582580120559271, 30.84685318188643066, 2.449293598294708485E-15 ) ) ;
#5942 = ORIENTED_EDGE ( 'NONE', *, *, #15794, .F. ) ;
#5943 = CARTESIAN_POINT ( 'NONE',  ( 4.995406935893289102, 10.78321810388998081, 10.78321810389001811 ) ) ;
#5944 = CARTESIAN_POINT ( 'NONE',  ( 98.29820294267314296, 18.47759065023127079, 7.653668647304074923 ) ) ;
#5945 = DIRECTION ( 'NONE',  ( 0.000000000000000000, -0.9767746502210202797, 0.2142691827715867137 ) ) ;
#5946 = CARTESIAN_POINT ( 'NONE',  ( -56.48582580120559271, -9.153146818113595984, 0.000000000000000000 ) ) ;
#5947 = ORIENTED_EDGE ( 'NONE', *, *, #11202, .F. ) ;
#5948 = CARTESIAN_POINT ( 'NONE',  ( -190.0144222802868228, -47.57278142029906576, 13.91469272131868884 ) ) ;
#5949 = CIRCLE ( 'NONE', #22097, 74.99999999999995737 ) ;
#5950 = CARTESIAN_POINT ( 'NONE',  ( 199.9999999999999432, -17.61942792365240607, -7.131405496535110800 ) ) ;
#5951 = CARTESIAN_POINT ( 'NONE',  ( 16.38602454706083122, -24.50452114744929233, 44.43226271088774837 ) ) ;
#5952 = AXIS2_PLACEMENT_3D ( 'NONE', #155, #4026, #18376 ) ;
#5953 = CARTESIAN_POINT ( 'NONE',  ( 17.91733029159796686, 14.04577174276132290, -48.44632265253467551 ) ) ;
#5954 = CARTESIAN_POINT ( 'NONE',  ( 199.0156165598358768, -13.68207045034666969, -14.60203791353019476 ) ) ;
#5955 = CARTESIAN_POINT ( 'NONE',  ( -200.0000000000000000, -61.50000000000001421, 66.50000000000005684 ) ) ;
#5956 = CARTESIAN_POINT ( 'NONE',  ( 184.8905102610680444, 1.070102760522089011E-13, -20.92133201514444352 ) ) ;
#5957 = CARTESIAN_POINT ( 'NONE',  ( -213.1075012329537230, 37.98287015391280619, -37.98287015391192512 ) ) ;
#5958 = CARTESIAN_POINT ( 'NONE',  ( -87.13361725327075646, -1.371494812282539888, 21.49321519333427588 ) ) ;
#5960 = CARTESIAN_POINT ( 'NONE',  ( -162.0762913951020892, 1.198031840385732849, -1.198031840385733515 ) ) ;
#5959 = CARTESIAN_POINT ( 'NONE',  ( -191.2490444017329878, 18.16428715637510294, -43.85246840377958932 ) ) ;
#5961 = CARTESIAN_POINT ( 'NONE',  ( 146.6084372240433993, 34.62501878078308692, 0.000000000000000000 ) ) ;
#5962 = CARTESIAN_POINT ( 'NONE',  ( -56.48582580120559982, 9.153146818113574668, -40.00000000000002132 ) ) ;
#5963 = CARTESIAN_POINT ( 'NONE',  ( -192.9588430854690273, 14.46834944099966336, 40.00000000000002132 ) ) ;
#5964 = CARTESIAN_POINT ( 'NONE',  ( -198.0356074513804572, -39.99999999999948130, -55.37879056874863437 ) ) ;
#5965 = CARTESIAN_POINT ( 'NONE',  ( -192.9588430854690273, 66.79921049721887982, 10.23066800229522677 ) ) ;
#5966 = DIRECTION ( 'NONE',  ( -4.657398277317547006E-32, 1.682156097916904327E-16, 1.000000000000000000 ) ) ;
#5967 = CARTESIAN_POINT ( 'NONE',  ( -238.4067589809705794, 27.60227080167080160, -28.96627169325299533 ) ) ;
#5968 = ORIENTED_EDGE ( 'NONE', *, *, #56, .T. ) ;
#5969 = CARTESIAN_POINT ( 'NONE',  ( -213.1075012329537230, 9.698598906450410340, 9.698598906450483170 ) ) ;
#5970 = CIRCLE ( 'NONE', #8460, 31.79780246617542616 ) ;
#5971 = EDGE_CURVE ( 'NONE', #2425, #3856, #1146, .T. ) ;
#5972 = CARTESIAN_POINT ( 'NONE',  ( -97.73806390046074455, -8.581719943970163911, 20.71810467719253523 ) ) ;
#5973 = ITEM_DEFINED_TRANSFORMATION ( 'NONE', 'NONE', #12984,  #21058 ) ;
#5974 = ORIENTED_EDGE ( 'NONE', *, *, #2171, .T. ) ;
#5975 = ORIENTED_EDGE ( 'NONE', *, *, #3142, .T. ) ;
#5976 = CARTESIAN_POINT ( 'NONE',  ( 151.7948205124836534, -33.06932595376343897, -23.49921654116042902 ) ) ;
#5977 = CARTESIAN_POINT ( 'NONE',  ( 23.84827734669607580, -46.63681169410487115, -13.76599369847224530 ) ) ;
#5978 = ORIENTED_EDGE ( 'NONE', *, *, #26177, .T. ) ;
#5979 = CARTESIAN_POINT ( 'NONE',  ( 163.1118516004056573, -27.26290988616869626, -40.00000000000002132 ) ) ;
#5980 = CARTESIAN_POINT ( 'NONE',  ( -93.01854144619034059, -20.65013722612175329, 8.553566904080200928 ) ) ;
#5981 = ORIENTED_EDGE ( 'NONE', *, *, #18822, .T. ) ;
#5982 = CARTESIAN_POINT ( 'NONE',  ( 199.9999999999998863, 6.967860089407453827, 17.68684069956508154 ) ) ;
#5983 =( BOUNDED_SURFACE ( )  B_SPLINE_SURFACE ( 3, 2, ( 
 ( #6705, #16822, #470 ),
 ( #18821, #10712, #16952 ),
 ( #25088, #4864, #24819 ),
 ( #14427, #20956, #6571 ),
 ( #21089, #6838, #8438 ),
 ( #16687, #14691, #22822 ),
 ( #4599, #18417, #12697 ),
 ( #20825, #10571, #601 ),
 ( #12967, #24959, #22689 ),
 ( #23093, #20691, #14819 ),
 ( #10437, #10841, #14958 ),
 ( #16557, #2872, #16427 ),
 ( #22952, #192, #4730 ),
 ( #8302, #18959, #24554 ),
 ( #6309, #12839, #22558 ),
 ( #739, #12429, #20557 ) ),
 .UNSPECIFIED., .F., .F., .F. ) 
 B_SPLINE_SURFACE_WITH_KNOTS ( ( 4, 2, 2, 2, 2, 2, 2, 4 ),
 ( 3, 3 ),
 ( 0.04143342415519529059, 0.04844520227997907436, 0.05195109134237096277, 0.05545698040476285118, 0.06246875852954662800, 0.06422170306074256874, 0.06597464759193852335, 0.06948053665433040482 ),
 ( 0.000000000000000000, 1.000000000000000000 ),
 .UNSPECIFIED. ) 
 GEOMETRIC_REPRESENTATION_ITEM ( )  RATIONAL_B_SPLINE_SURFACE ( (
 ( 1.000000000000000000, 0.9541700777564864344, 1.000000000000000000),
 ( 1.000000000000000000, 0.9520170179160779567, 1.000000000000000000),
 ( 1.000000000000000000, 0.9503264940267351912, 1.000000000000000000),
 ( 1.000000000000000000, 0.9485966650357424701, 1.000000000000000000),
 ( 1.000000000000000000, 0.9481601953987753850, 1.000000000000000000),
 ( 1.000000000000000000, 0.9475786562871791885, 1.000000000000000000),
 ( 1.000000000000000000, 0.9474333041661833210, 1.000000000000000000),
 ( 1.000000000000000000, 0.9474385324120137009, 1.000000000000000000),
 ( 1.000000000000000000, 0.9480205960577967605, 1.000000000000000000),
 ( 1.000000000000000000, 0.9494433550397415322, 1.000000000000000000),
 ( 1.000000000000000000, 0.9497628485353458716, 1.000000000000000000),
 ( 1.000000000000000000, 0.9504717112743156227, 1.000000000000000000),
 ( 1.000000000000000000, 0.9508623530681812319, 1.000000000000000000),
 ( 1.000000000000000000, 0.9521262215765325942, 1.000000000000000000),
 ( 1.000000000000000000, 0.9530922057186239638, 1.000000000000000000),
 ( 1.000000000000000000, 0.9541700777564561253, 1.000000000000000000) ) ) 
 REPRESENTATION_ITEM ( '' )  SURFACE ( )  );
#5984 = DIRECTION ( 'NONE',  ( 0.000000000000000000, 0.000000000000000000, 1.000000000000000000 ) ) ;
#5985 = CARTESIAN_POINT ( 'NONE',  ( 0.2972598230769886718, 38.42060263243669027, -18.14793986248710667 ) ) ;
#5986 = CARTESIAN_POINT ( 'NONE',  ( -188.3611024622163370, -43.02327292322560481, -23.46270902204799569 ) ) ;
#5987 = CARTESIAN_POINT ( 'NONE',  ( -162.0762913951021176, -40.00000000000005684, 1.694272876828184504 ) ) ;
#5988 = CARTESIAN_POINT ( 'NONE',  ( -198.0356074513804572, 55.37879056871320671, 40.00000000000002132 ) ) ;
#5989 = CARTESIAN_POINT ( 'NONE',  ( -135.8532207217289738, -6.472252184283586729, -50.09629031063973770 ) ) ;
#5990 = CARTESIAN_POINT ( 'NONE',  ( 199.0223319294094892, 2.599958516019920118, 19.83413122362564351 ) ) ;
#5991 = VECTOR ( 'NONE', #15108, 1000.000000000000000 ) ;
#5992 = AXIS2_PLACEMENT_3D ( 'NONE', #1911, #14139, #4045 ) ;
#5993 = CARTESIAN_POINT ( 'NONE',  ( 146.6084372240433993, 1.478241399363601114E-13, -34.62501878078305850 ) ) ;
#5994 = CARTESIAN_POINT ( 'NONE',  ( 200.0000000000000000, -40.00000000000005684, 19.99999999999978328 ) ) ;
#5995 = CIRCLE ( 'NONE', #20876, 34.99999999999999289 ) ;
#5996 = CARTESIAN_POINT ( 'NONE',  ( -91.56559293963834989, -2.543181659092656077E-13, 22.67402823373191723 ) ) ;
#5997 = CARTESIAN_POINT ( 'NONE',  ( 14.38125909742180220, 39.99999999999997158, 15.17850393972647716 ) ) ;
#5998 = FACE_BOUND ( 'NONE', #1825, .T. ) ;
#5999 = CARTESIAN_POINT ( 'NONE',  ( 4.995406935893310418, -67.35176059880237176, 10.78321810387813429 ) ) ;
#6000 = CARTESIAN_POINT ( 'NONE',  ( -105.3755690713226869, 21.75974354311648540, -0.000000000000000000 ) ) ;
#6001 = CARTESIAN_POINT ( 'NONE',  ( 19.06497207195981858, -38.31983398719616218, -18.24870850772777331 ) ) ;
#6002 = LINE ( 'NONE', #17956, #727 ) ;
#6003 = DIRECTION ( 'NONE',  ( -1.000000000000000000, -1.836970198721030181E-16, 0.000000000000000000 ) ) ;
#6004 = CARTESIAN_POINT ( 'NONE',  ( -91.56559293963836410, 39.99999999999976552, 22.67402823373234000 ) ) ;
#6005 = CARTESIAN_POINT ( 'NONE',  ( -91.56559293963834989, -7.976292724337646577E-14, 17.32597176626811120 ) ) ;
#6006 = CARTESIAN_POINT ( 'NONE',  ( 0.2972598230769907257, 66.70487387989857098, 10.13633138497486641 ) ) ;
#6007 = CARTESIAN_POINT ( 'NONE',  ( 91.82158438592158234, 12.16597498397756993, 12.16597498397776356 ) ) ;
#6008 = CARTESIAN_POINT ( 'NONE',  ( -188.3120606736019909, -13.82878088495181323, -46.99497558484008408 ) ) ;
#6009 = CARTESIAN_POINT ( 'NONE',  ( 4.995406935893293543, -10.78321810389005364, 10.78321810388994173 ) ) ;
#6010 = ORIENTED_EDGE ( 'NONE', *, *, #19720, .T. ) ;
#6011 = CARTESIAN_POINT ( 'NONE',  ( -259.2033419157646676, -6.730120644403663199, 6.730120644403451813 ) ) ;
#6012 = CARTESIAN_POINT ( 'NONE',  ( 98.29820294267868519, -19.50609486047250840, 5.170639833975480215 ) ) ;
#6013 = CARTESIAN_POINT ( 'NONE',  ( 98.29820294267493352, -20.00000000000511235, 5.223721743777709619E-12 ) ) ;
#6014 = CARTESIAN_POINT ( 'NONE',  ( -192.9588430854690273, -18.05360324515400094, -38.51493924976961836 ) ) ;
#6015 = DIRECTION ( 'NONE',  ( 0.8802361161597900274, 5.811389476877145599E-17, 0.4745359626076074422 ) ) ;
#6016 = ORIENTED_EDGE ( 'NONE', *, *, #20204, .F. ) ;
#6017 = CIRCLE ( 'NONE', #20890, 30.00000000000005329 ) ;
#6018 = CARTESIAN_POINT ( 'NONE',  ( 199.9999999999999432, 18.08994308216479752, 5.827519331295367699 ) ) ;
#6019 = DIRECTION ( 'NONE',  ( 1.000000000000000000, 1.836970198721030427E-16, -0.000000000000000000 ) ) ;
#6020 = CARTESIAN_POINT ( 'NONE',  ( -4.439300432585279843, 23.37136716947921755, 42.88738538954466151 ) ) ;
#6021 = CIRCLE ( 'NONE', #497, 29.99999999999999645 ) ;
#6022 = ORIENTED_EDGE ( 'NONE', *, *, #23619, .T. ) ;
#6023 = ORIENTED_EDGE ( 'NONE', *, *, #16147, .T. ) ;
#6024 = CARTESIAN_POINT ( 'NONE',  ( 136.1360204305621266, -35.03383547441293899, 0.000000000000000000 ) ) ;
#6025 = CARTESIAN_POINT ( 'NONE',  ( 199.0138211924391385, -10.98290011267725141, -16.71408225681557980 ) ) ;
#6026 = CARTESIAN_POINT ( 'NONE',  ( -105.3844690779178137, -6.703180366840864046, -20.33701293466475946 ) ) ;
#6027 = DIRECTION ( 'NONE',  ( 0.01051738792037367962, -0.3995761383046945725, 0.9166396752534989867 ) ) ;
#6028 = CARTESIAN_POINT ( 'NONE',  ( 18.89824403360310967, 43.99464769172853096, -24.18164459663352517 ) ) ;
#6029 = CARTESIAN_POINT ( 'NONE',  ( -162.0762913951021176, 40.00000000000001421, -1.694272876827905394 ) ) ;
#6030 = DIRECTION ( 'NONE',  ( 0.000000000000000000, 0.000000000000000000, 1.000000000000000000 ) ) ;
#6031 = FACE_OUTER_BOUND ( 'NONE', #6436, .T. ) ;
#6032 = AXIS2_PLACEMENT_3D ( 'NONE', #11312, #25567, #3586 ) ;
#6033 = DIRECTION ( 'NONE',  ( -1.000000000000000000, 0.000000000000000000, 0.000000000000000000 ) ) ;
#6034 = CARTESIAN_POINT ( 'NONE',  ( 199.0194208361885444, 8.684746017668368623, 18.01861981654000999 ) ) ;
#6035 = CARTESIAN_POINT ( 'NONE',  ( -128.3942957220574215, 24.92786587692849665, 10.32546012722446704 ) ) ;
#6036 = CARTESIAN_POINT ( 'NONE',  ( -2.557884977116410941, -13.90734923103991072, -47.52441970260808546 ) ) ;
#6037 = CARTESIAN_POINT ( 'NONE',  ( 4.995406935893305977, -39.06748935135157552, -39.06748935135225764 ) ) ;
#6038 =( BOUNDED_SURFACE ( )  B_SPLINE_SURFACE ( 3, 3, ( 
 ( #17531, #15283, #21413, #11293, #25544, #1317, #7295, #15409, #3314, #21539, #26067, #13933, #5564, #19793, #5690, #21793, #3840, #1448, #22204, #3565, #1580, #16062, #22068, #3979, #21930, #1845, #19661, #9819, #5830, #24188 ),
 ( #11669, #25934, #13795, #11807, #18057, #20069, #7415, #23915, #21665, #9683, #9548, #11943, #12076, #5962, #9948, #20198, #15530, #1710, #14072, #23658, #7675, #3704, #17789, #15788, #5438, #11537, #26208, #1977, #13539, #19927 ),
 ( #7944, #3438, #17657, #25798, #10083, #18187, #13671, #17923, #7546, #7805, #15658, #23784, #15921, #24054, #18729, #10483, #4377, #24730, #14337, #22864, #106, #6615, #12210, #6486, #22337, #14598, #4112, #12468, #22728, #4248 ),
 ( #6096, #18597, #16469, #14468, #14732, #10616, #16597, #18458, #20595, #10218, #513, #8213, #2371, #8080, #8618, #16729, #24860, #16198, #8479, #22469, #14203, #20332, #24332, #375, #4641, #4506, #6349, #2241, #12607, #20466 ),
 ( #2109, #12743, #20736, #20863, #18325, #16331, #10348, #2647, #24460, #6224, #236, #2505, #8348, #10754, #12338, #24593, #22601, #26338, #25871, #13356, #5633, #18865, #25737, #23601, #8752, #5380, #25000, #11478, #9364, #7361 ),
 ( #16868, #16996, #9493, #15472, #13485, #19473, #25616, #21606, #15600, #25131, #6881, #21736, #15730, #8885, #17730, #3379, #15356, #6753, #7615, #19606, #7489, #12880, #646, #23480, #14865, #1392, #779, #4776, #9627, #5252 ),
 ( #21478, #20996, #17598, #3253, #10890, #13740, #22999, #11357, #2778, #23725, #19002, #5506, #13607, #1260, #23855, #17474, #3512, #11612, #19734, #1521, #21866, #3642, #5904, #19867, #22141, #14278, #10295, #12284, #16006, #3922 ) ),
 .UNSPECIFIED., .T., .F., .T. ) 
 B_SPLINE_SURFACE_WITH_KNOTS ( ( 4, 3, 4 ),
 ( 4, 2, 2, 2, 2, 2, 2, 2, 2, 2, 2, 2, 2, 2, 4 ),
 ( 0.000000000000000000, 0.5000000000000000000, 1.000000000000000000 ),
 ( 0.000000000000000000, 0.1357259735107005372, 0.1651108541090157700, 0.1944957347073310028, 0.3598804999793158710, 0.3867117631979620773, 0.4135430264166082281, 0.5789277916885930964, 0.6062785021374117456, 0.6336292125862302838, 0.8508620842112317728, 0.8814014469398914198, 0.9119408096685510667, 0.9559704048342755334, 1.000000000000000000 ),
 .UNSPECIFIED. ) 
 GEOMETRIC_REPRESENTATION_ITEM ( )  RATIONAL_B_SPLINE_SURFACE ( (
 ( 1.000000000000000000, 1.000000000000000000, 1.000000000000000000, 1.000000000000000000, 1.000000000000000000, 1.000000000000000000, 1.000000000000000000, 1.000000000000000000, 1.000000000000000000, 1.000000000000000000, 1.000000000000000000, 1.000000000000000000, 1.000000000000000000, 1.000000000000000000, 1.000000000000000000, 1.000000000000000000, 1.000000000000000000, 1.000000000000000000, 1.000000000000000000, 1.000000000000000000, 1.000000000000000000, 1.000000000000000000, 1.000000000000000000, 1.000000000000000000, 1.000000000000000000, 1.000000000000000000, 1.000000000000000000, 1.000000000000000000, 1.000000000000000000, 1.000000000000000000),
 ( 0.3333333333333333703, 0.3333333333333333703, 0.3333333333333333703, 0.3333333333333333703, 0.3333333333333333703, 0.3333333333333333703, 0.3333333333333333703, 0.3333333333333333703, 0.3333333333333333703, 0.3333333333333333703, 0.3333333333333333703, 0.3333333333333333703, 0.3333333333333333703, 0.3333333333333333703, 0.3333333333333333703, 0.3333333333333333703, 0.3333333333333333703, 0.3333333333333333703, 0.3333333333333333703, 0.3333333333333333703, 0.3333333333333333703, 0.3333333333333333703, 0.3333333333333333703, 0.3333333333333333703, 0.3333333333333333703, 0.3333333333333333703, 0.3333333333333333703, 0.3333333333333333703, 0.3333333333333333703, 0.3333333333333333703),
 ( 0.3333333333333333703, 0.3333333333333333703, 0.3333333333333333703, 0.3333333333333333703, 0.3333333333333333703, 0.3333333333333333703, 0.3333333333333333703, 0.3333333333333333703, 0.3333333333333333703, 0.3333333333333333703, 0.3333333333333333703, 0.3333333333333333703, 0.3333333333333333703, 0.3333333333333333703, 0.3333333333333333703, 0.3333333333333333703, 0.3333333333333333703, 0.3333333333333333703, 0.3333333333333333703, 0.3333333333333333703, 0.3333333333333333703, 0.3333333333333333703, 0.3333333333333333703, 0.3333333333333333703, 0.3333333333333333703, 0.3333333333333333703, 0.3333333333333333703, 0.3333333333333333703, 0.3333333333333333703, 0.3333333333333333703),
 ( 1.000000000000000000, 1.000000000000000000, 1.000000000000000000, 1.000000000000000000, 1.000000000000000000, 1.000000000000000000, 1.000000000000000000, 1.000000000000000000, 1.000000000000000000, 1.000000000000000000, 1.000000000000000000, 1.000000000000000000, 1.000000000000000000, 1.000000000000000000, 1.000000000000000000, 1.000000000000000000, 1.000000000000000000, 1.000000000000000000, 1.000000000000000000, 1.000000000000000000, 1.000000000000000000, 1.000000000000000000, 1.000000000000000000, 1.000000000000000000, 1.000000000000000000, 1.000000000000000000, 1.000000000000000000, 1.000000000000000000, 1.000000000000000000, 1.000000000000000000),
 ( 0.3333333333333333703, 0.3333333333333333703, 0.3333333333333333703, 0.3333333333333333703, 0.3333333333333333703, 0.3333333333333333703, 0.3333333333333333703, 0.3333333333333333703, 0.3333333333333333703, 0.3333333333333333703, 0.3333333333333333703, 0.3333333333333333703, 0.3333333333333333703, 0.3333333333333333703, 0.3333333333333333703, 0.3333333333333333703, 0.3333333333333333703, 0.3333333333333333703, 0.3333333333333333703, 0.3333333333333333703, 0.3333333333333333703, 0.3333333333333333703, 0.3333333333333333703, 0.3333333333333333703, 0.3333333333333333703, 0.3333333333333333703, 0.3333333333333333703, 0.3333333333333333703, 0.3333333333333333703, 0.3333333333333333703),
 ( 0.3333333333333333703, 0.3333333333333333703, 0.3333333333333333703, 0.3333333333333333703, 0.3333333333333333703, 0.3333333333333333703, 0.3333333333333333703, 0.3333333333333333703, 0.3333333333333333703, 0.3333333333333333703, 0.3333333333333333703, 0.3333333333333333703, 0.3333333333333333703, 0.3333333333333333703, 0.3333333333333333703, 0.3333333333333333703, 0.3333333333333333703, 0.3333333333333333703, 0.3333333333333333703, 0.3333333333333333703, 0.3333333333333333703, 0.3333333333333333703, 0.3333333333333333703, 0.3333333333333333703, 0.3333333333333333703, 0.3333333333333333703, 0.3333333333333333703, 0.3333333333333333703, 0.3333333333333333703, 0.3333333333333333703),
 ( 1.000000000000000000, 1.000000000000000000, 1.000000000000000000, 1.000000000000000000, 1.000000000000000000, 1.000000000000000000, 1.000000000000000000, 1.000000000000000000, 1.000000000000000000, 1.000000000000000000, 1.000000000000000000, 1.000000000000000000, 1.000000000000000000, 1.000000000000000000, 1.000000000000000000, 1.000000000000000000, 1.000000000000000000, 1.000000000000000000, 1.000000000000000000, 1.000000000000000000, 1.000000000000000000, 1.000000000000000000, 1.000000000000000000, 1.000000000000000000, 1.000000000000000000, 1.000000000000000000, 1.000000000000000000, 1.000000000000000000, 1.000000000000000000, 1.000000000000000000) ) ) 
 REPRESENTATION_ITEM ( '' )  SURFACE ( )  );
#6039 = CARTESIAN_POINT ( 'NONE',  ( -200.0000000000000568, 19.51623549979305494, 45.81998439131043455 ) ) ;
#6040 = CARTESIAN_POINT ( 'NONE',  ( -280.0000000000000568, -42.42640687119285303, -14.14213562373118371 ) ) ;
#6041 = CARTESIAN_POINT ( 'NONE',  ( 199.9999999999999432, -1.727494763561684666E-13, 20.00000000000010303 ) ) ;
#6042 = CARTESIAN_POINT ( 'NONE',  ( -192.9588430854690273, 18.05360324515473280, -38.51493924976924177 ) ) ;
#6043 = CARTESIAN_POINT ( 'NONE',  ( -86.96347745069643054, -18.24025645688353947, 40.00000000000002132 ) ) ;
#6044 = CARTESIAN_POINT ( 'NONE',  ( -208.1127848780265026, 10.60833733269551615, -10.60833733269529766 ) ) ;
#6045 = CARTESIAN_POINT ( 'NONE',  ( -135.8532207217289738, -30.84685318188647685, -2.449293598294708485E-15 ) ) ;
#6046 = CARTESIAN_POINT ( 'NONE',  ( -114.7366410982253910, 17.62971985773716810, 13.31543432720488518 ) ) ;
#6047 = CARTESIAN_POINT ( 'NONE',  ( -213.1075012329537230, 5.259461644596141978E-13, -53.71589010951915100 ) ) ;
#6048 = CARTESIAN_POINT ( 'NONE',  ( -30.26275506840324070, 1.198031551616013601, 1.198031551616023371 ) ) ;
#6049 = CARTESIAN_POINT ( 'NONE',  ( -280.0000000000000568, -20.00000000000006750, -40.00000000000002132 ) ) ;
#6050 = VERTEX_POINT ( 'NONE', #7620 ) ;
#6051 = VERTEX_POINT ( 'NONE', #15866 ) ;
#6052 = CARTESIAN_POINT ( 'NONE',  ( 130.8568914410475088, -34.05028731879786363, 40.00000000000002132 ) ) ;
#6053 = AXIS2_PLACEMENT_3D ( 'NONE', #9181, #13298, #17294 ) ;
#6054 = EDGE_CURVE ( 'NONE', #1209, #15843, #12725, .T. ) ;
#6055 = CARTESIAN_POINT ( 'NONE',  ( -56.48582580120558561, -1.205267837095813407E-13, 30.84685318188644132 ) ) ;
#6056 = CARTESIAN_POINT ( 'NONE',  ( -208.1127848780264742, 38.89260858015707356, 17.67593391476696141 ) ) ;
#6057 = CARTESIAN_POINT ( 'NONE',  ( 130.8568914410475372, -34.05028731879786363, 0.000000000000000000 ) ) ;
#6058 = FACE_OUTER_BOUND ( 'NONE', #432, .T. ) ;
#6059 = LINE ( 'NONE', #196, #10503 ) ;
#6060 = CARTESIAN_POINT ( 'NONE',  ( 200.0000000000000000, 16.44874601624584187, 9.522804452304930223 ) ) ;
#6061 = ADVANCED_FACE ( 'NONE', ( #3259 ), #8708, .T. ) ;
#6062 = EDGE_CURVE ( 'NONE', #22617, #1078, #16835, .T. ) ;
#6063 = CARTESIAN_POINT ( 'NONE',  ( 200.0000000000000000, -13.87499997850619060, -12.99183991311445929 ) ) ;
#6064 = CARTESIAN_POINT ( 'NONE',  ( 163.1118516004056573, 9.006482792069759213, -9.006482792069505194 ) ) ;
#6065 = CARTESIAN_POINT ( 'NONE',  ( -192.9588430854690273, -66.79921049721887982, -10.23066800229569040 ) ) ;
#6066 = FACE_OUTER_BOUND ( 'NONE', #15547, .T. ) ;
#6067 = CARTESIAN_POINT ( 'NONE',  ( -91.56559293963834989, -2.543181659092656077E-13, 22.67402823373191723 ) ) ;
#6068 = CARTESIAN_POINT ( 'NONE',  ( -238.4067589809705794, -28.96627169325352469, 27.60227080167035041 ) ) ;
#6069 = CARTESIAN_POINT ( 'NONE',  ( -135.8532207217289738, -6.472252184284280396, 6.472252184284099208 ) ) ;
#6070 = CARTESIAN_POINT ( 'NONE',  ( -100.7734535825088500, -44.31723036834885932, -12.25131212657538171 ) ) ;
#6071 = CARTESIAN_POINT ( 'NONE',  ( 163.1118516004056573, 19.27778845538780317, -19.27778845538757224 ) ) ;
#6072 = CARTESIAN_POINT ( 'NONE',  ( 199.0230791219081254, 0.7206054984853534906, 19.99107781132848416 ) ) ;
#6074 = CARTESIAN_POINT ( 'NONE',  ( 151.7948205124836250, 1.807796684091926154E-15, 6.767089262349031742 ) ) ;
#6073 = CARTESIAN_POINT ( 'NONE',  ( 19.06497207195981147, 38.31983398719673772, -38.31983398719579981 ) ) ;
#6075 = CARTESIAN_POINT ( 'NONE',  ( 14.38125909742180220, 39.01709431150892016, 17.55144818341517166 ) ) ;
#6076 = CARTESIAN_POINT ( 'NONE',  ( 23.17367289775338435, 46.88342923877050339, -13.81211338457316806 ) ) ;
#6077 = CARTESIAN_POINT ( 'NONE',  ( 57.59792236341147031, 37.56421063658187620, -40.00000000000002132 ) ) ;
#6078 = ORIENTED_EDGE ( 'NONE', *, *, #8472, .F. ) ;
#6079 = CARTESIAN_POINT ( 'NONE',  ( -162.0762913951020892, 1.694272876828294194, 0.000000000000000000 ) ) ;
#6080 = CARTESIAN_POINT ( 'NONE',  ( -40.07203023070061931, -32.10811084140490834, 16.33025453626358825 ) ) ;
#6081 = CARTESIAN_POINT ( 'NONE',  ( -238.4067589809705794, 0.9644942799825386714, 0.000000000000000000 ) ) ;
#6082 = VERTEX_POINT ( 'NONE', #13338 ) ;
#6083 = CARTESIAN_POINT ( 'NONE',  ( -189.1815713358170399, -43.37724571962257158, 17.96744347545579146 ) ) ;
#6084 = CARTESIAN_POINT ( 'NONE',  ( 199.9999999999999147, -17.05087848619496782, 8.411269650559694000 ) ) ;
#6085 = CARTESIAN_POINT ( 'NONE',  ( 6.202588567996007995, -24.77700748806806175, 44.80189419270405438 ) ) ;
#6086 = CARTESIAN_POINT ( 'NONE',  ( 23.25494099740788556, 17.82744980610155849, -43.03927110441497916 ) ) ;
#6087 = CARTESIAN_POINT ( 'NONE',  ( 199.0097900131551114, -3.258944298918965199, -19.73026277452668609 ) ) ;
#6088 = DIRECTION ( 'NONE',  ( 1.000000000000000000, 0.000000000000000000, 0.000000000000000000 ) ) ;
#6089 = PLANE ( 'NONE',  #12589 ) ;
#6090 = CARTESIAN_POINT ( 'NONE',  ( -114.4388184736403389, -8.352332320002028965, 20.16431396440694002 ) ) ;
#6091 = CARTESIAN_POINT ( 'NONE',  ( 192.4448373802100889, 14.14213562370330379, -14.14213562370292365 ) ) ;
#6092 = CARTESIAN_POINT ( 'NONE',  ( 163.1118516004056573, 27.26290988616876021, 40.00000000000002132 ) ) ;
#6094 = CARTESIAN_POINT ( 'NONE',  ( -100.7734535825088358, -16.03295912088728770, 16.03295912088687913 ) ) ;
#6093 = CARTESIAN_POINT ( 'NONE',  ( -188.2507053403064674, 13.82466505297411885, -46.97353740712659231 ) ) ;
#6095 = CARTESIAN_POINT ( 'NONE',  ( -238.4067589809705794, 0.6820004457912851592, -0.6820004457913123597 ) ) ;
#6096 = CARTESIAN_POINT ( 'NONE',  ( -280.0000000000000000, -20.00000000000006750, -2.449293598294708485E-15 ) ) ;
#6097 = CARTESIAN_POINT ( 'NONE',  ( -100.7734535825088358, 17.32597176626809343, 2.449293598294708485E-15 ) ) ;
#6098 = CARTESIAN_POINT ( 'NONE',  ( -56.48582580120557850, -39.99999999999970868, -30.84685318188687120 ) ) ;
#6099 = CARTESIAN_POINT ( 'NONE',  ( -105.3755690713226585, 41.18208027870598187, -15.38646221621779731 ) ) ;
#6100 = DIRECTION ( 'NONE',  ( 0.000000000000000000, -4.182618615277681568E-16, -1.000000000000000000 ) ) ;
#6101 = CARTESIAN_POINT ( 'NONE',  ( -105.3755690713226585, 43.67073346367988051, -12.89780903124366418 ) ) ;
#6102 = ORIENTED_EDGE ( 'NONE', *, *, #24595, .T. ) ;
#6103 = CARTESIAN_POINT ( 'NONE',  ( -91.56559293963834989, -16.03295912088706388, -16.03295912088710651 ) ) ;
#6104 = CARTESIAN_POINT ( 'NONE',  ( -188.5332406156510388, -13.84065976281315180, -47.07509730618265564 ) ) ;
#6105 = VERTEX_POINT ( 'NONE', #21846 ) ;
#6106 = ORIENTED_EDGE ( 'NONE', *, *, #24953, .T. ) ;
#6107 = CARTESIAN_POINT ( 'NONE',  ( 192.4448373802100889, 14.14213562375893574, -14.14213562375874922 ) ) ;
#6108 = CARTESIAN_POINT ( 'NONE',  ( 60.28378959931642100, -31.18416451518941912, -15.72633063265140407 ) ) ;
#6109 = ORIENTED_EDGE ( 'NONE', *, *, #19079, .F. ) ;
#6110 = CARTESIAN_POINT ( 'NONE',  ( -91.56559293963834989, 17.32597176626809699, -40.00000000000002132 ) ) ;
#6111 = CARTESIAN_POINT ( 'NONE',  ( 190.0000000000000000, -35.78896085774753288, -1.496915739050591872E-14 ) ) ;
#6112 = VERTEX_POINT ( 'NONE', #21459 ) ;
#6113 = CARTESIAN_POINT ( 'NONE',  ( 200.0000000000000000, 9.224923989862913842, 16.61864493261536424 ) ) ;
#6114 = DIRECTION ( 'NONE',  ( 0.000000000000000000, -1.000000000000000000, 0.000000000000000000 ) ) ;
#6115 = CARTESIAN_POINT ( 'NONE',  ( 192.4448373802100889, -14.14213562375876698, -14.14213562375885047 ) ) ;
#6116 = CARTESIAN_POINT ( 'NONE',  ( -188.3392995398489802, -43.01688924973668549, -23.45797413244871166 ) ) ;
#6117 = CARTESIAN_POINT ( 'NONE',  ( -198.0356074513804572, -40.00000000000025580, 55.37879056871310013 ) ) ;
#6118 = CARTESIAN_POINT ( 'NONE',  ( 136.1360204305621551, -35.03383547441293899, 40.00000000000002132 ) ) ;
#6119 = CARTESIAN_POINT ( 'NONE',  ( -259.2033419157646676, -35.01439189186523748, -21.55415060305881170 ) ) ;
#6120 = CARTESIAN_POINT ( 'NONE',  ( 199.0253172846266523, -6.444568167316012008, 18.94088585829734228 ) ) ;
#6121 = CARTESIAN_POINT ( 'NONE',  ( -91.56559293963834989, -39.99999999999995737, -22.67402823373205933 ) ) ;
#6122 = CARTESIAN_POINT ( 'NONE',  ( 163.1118516004056573, -1.695744499706194789E-14, 12.73709011382475254 ) ) ;
#6123 = CARTESIAN_POINT ( 'NONE',  ( -238.4067589809705794, 39.99999999999997158, 0.9644942799827220803 ) ) ;
#6124 = CARTESIAN_POINT ( 'NONE',  ( -162.0762913951021176, -1.694272876828353702, -40.00000000000002132 ) ) ;
#6125 = CARTESIAN_POINT ( 'NONE',  ( 170.2234770963711128, -10.92277846919202666, 10.92277846919193962 ) ) ;
#6126 = CARTESIAN_POINT ( 'NONE',  ( 130.8568914410475372, 34.05028731879791337, 0.000000000000000000 ) ) ;
#6127 = CARTESIAN_POINT ( 'NONE',  ( 184.8905102610680444, -13.49065550809780412, -43.07788698682583828 ) ) ;
#6128 = CARTESIAN_POINT ( 'NONE',  ( -93.02511667906880177, -8.946512270085145602, 20.50052124204815129 ) ) ;
#6129 = CARTESIAN_POINT ( 'NONE',  ( -626.9846540392142060, 90.00000000000000000, 0.000000000000000000 ) ) ;
#6130 = CARTESIAN_POINT ( 'NONE',  ( -56.48582580120559271, -1.062504017861011783E-13, 9.153146818113587102 ) ) ;
#6131 = CARTESIAN_POINT ( 'NONE',  ( 192.4448373802101173, -40.00000000000005684, 19.99999999996046185 ) ) ;
#6132 = CARTESIAN_POINT ( 'NONE',  ( 57.59792236341147031, 54.84617931850881689, -1.722363176414946073 ) ) ;
#6133 = CARTESIAN_POINT ( 'NONE',  ( -91.56559293963836410, 16.03295912088692177, 16.03295912088721664 ) ) ;
#6134 = CARTESIAN_POINT ( 'NONE',  ( -188.2507053402904660, -13.82466505297120740, -46.97353740712224379 ) ) ;
#6135 = CARTESIAN_POINT ( 'NONE',  ( -135.8532207217289738, -21.81201906317758343, -34.75652343174620995 ) ) ;
#6136 = EDGE_LOOP ( 'NONE', ( #20119, #26186, #18384, #23799 ) ) ;
#6137 = CARTESIAN_POINT ( 'NONE',  ( -198.0356074513804572, 10.87444709759730088, -10.87444709759707173 ) ) ;
#6138 = DIRECTION ( 'NONE',  ( -0.7071067811865302533, 8.659560562355141167E-17, -0.7071067811865646702 ) ) ;
#6139 = CARTESIAN_POINT ( 'NONE',  ( -162.0762913951021176, -1.694272876828353702, -40.00000000000002132 ) ) ;
#6140 = DIRECTION ( 'NONE',  ( 0.000000000000000000, 0.000000000000000000, 1.000000000000000000 ) ) ;
#6141 = CARTESIAN_POINT ( 'NONE',  ( 170.2234770963711128, -17.36149277826940462, -39.20704971665412586 ) ) ;
#6142 = DIRECTION ( 'NONE',  ( 0.000000000000000000, 0.000000000000000000, -1.000000000000000000 ) ) ;
#6143 = ORIENTED_EDGE ( 'NONE', *, *, #1201, .T. ) ;
#6144 = CARTESIAN_POINT ( 'NONE',  ( 200.0000000000000000, 16.89533303742294734, 8.701242830477832868 ) ) ;
#6145 = CARTESIAN_POINT ( 'NONE',  ( 7.307793593482389660, -24.85783611765724999, 44.91153572052495235 ) ) ;
#6146 = EDGE_CURVE ( 'NONE', #87, #21399, #1123, .T. ) ;
#6147 = CARTESIAN_POINT ( 'NONE',  ( -5.866564133101844547, 13.69896896866289815, 46.35727274689033806 ) ) ;
#6148 = ORIENTED_EDGE ( 'NONE', *, *, #22583, .T. ) ;
#6149 = VERTEX_POINT ( 'NONE', #1242 ) ;
#6150 = CARTESIAN_POINT ( 'NONE',  ( 146.6084372240433993, -34.62501878078303008, 0.000000000000000000 ) ) ;
#6151 = CARTESIAN_POINT ( 'NONE',  ( 199.0056007646616933, 10.55815519723130969, -16.98307562551513072 ) ) ;
#6152 = CYLINDRICAL_SURFACE ( 'NONE', #914, 30.00000000000000355 ) ;
#6153 = EDGE_CURVE ( 'NONE', #17548, #20820, #8576, .T. ) ;
#6154 = B_SPLINE_CURVE_WITH_KNOTS ( 'NONE', 3,
 ( #1216, #9704, #21686, #7188, #23554, #13692, #11691, #9571, #5327, #9194, #17678, #15304 ),
 .UNSPECIFIED., .F., .F.,
 ( 4, 2, 2, 2, 2, 4 ),
 ( 2.860979249076398407E-17, 0.005971690550335911375, 0.008957535825503855353, 0.01045045846308778267, 0.01119691978187970643, 0.01194338110067163193 ),
 .UNSPECIFIED. ) ;
#6155 = CARTESIAN_POINT ( 'NONE',  ( -105.4741150117390731, -8.366608964594128395, -19.60045294982696973 ) ) ;
#6156 = EDGE_CURVE ( 'NONE', #8862, #24345, #15958, .T. ) ;
#6157 = CARTESIAN_POINT ( 'NONE',  ( 146.6084372240433709, 39.99999999999968026, 34.62501878078347772 ) ) ;
#6158 = CARTESIAN_POINT ( 'NONE',  ( 98.29820294267348402, 6.423630604792454513, -18.95183585406372373 ) ) ;
#6159 = CARTESIAN_POINT ( 'NONE',  ( -653.7331453363653964, 37.62258392649753347, 13.59271614633608571 ) ) ;
#6160 = CARTESIAN_POINT ( 'NONE',  ( -188.2995950289364089, 43.00522595870987885, -23.44932284465868477 ) ) ;
#6161 = CARTESIAN_POINT ( 'NONE',  ( 199.0190933210857906, 9.274233341078666371, 17.72222919763310856 ) ) ;
#6162 = CARTESIAN_POINT ( 'NONE',  ( -185.1929807734386486, 41.48858353734955529, 17.18513398481663756 ) ) ;
#6163 = CARTESIAN_POINT ( 'NONE',  ( 16.10036699868241783, -14.09853761975161390, -48.79524671499645905 ) ) ;
#6164 = CARTESIAN_POINT ( 'NONE',  ( -280.0000000000000000, -14.14213562373088706, -14.14213562373108424 ) ) ;
#6165 = CARTESIAN_POINT ( 'NONE',  ( -716.9846540392142060, -66.50000000000001421, 66.50000000000005684 ) ) ;
#6166 = CARTESIAN_POINT ( 'NONE',  ( -100.7734535825088500, -40.53558337403669753, -16.03295912088728770 ) ) ;
#6167 = CARTESIAN_POINT ( 'NONE',  ( -350.0000000000001137, -4.593501166854460352E-14, 21.53474504356805852 ) ) ;
#6168 = CARTESIAN_POINT ( 'NONE',  ( 130.8568914410475372, 24.07718906447210472, 24.07718906447249907 ) ) ;
#6169 = CARTESIAN_POINT ( 'NONE',  ( 170.2234770963711128, -15.44714144992812876, -2.449293598294708485E-15 ) ) ;
#6170 = DIRECTION ( 'NONE',  ( -1.000000000000000000, 0.000000000000000000, 0.000000000000000000 ) ) ;
#6171 = CARTESIAN_POINT ( 'NONE',  ( 184.8905102610680444, -19.07866798485553872, -40.00000000000002132 ) ) ;
#6172 = DIRECTION ( 'NONE',  ( 0.000000000000000000, 0.000000000000000000, 1.000000000000000000 ) ) ;
#6173 = CARTESIAN_POINT ( 'NONE',  ( 146.6084372240433709, 40.00000000000010658, -5.374981219216549810 ) ) ;
#6174 = CARTESIAN_POINT ( 'NONE',  ( 200.0000000000000000, 42.42640687119288856, -14.14213562373094746 ) ) ;
#6175 = CARTESIAN_POINT ( 'NONE',  ( 170.2234770963711128, -24.55285855007183926, 0.000000000000000000 ) ) ;
#6176 = VERTEX_POINT ( 'NONE', #4825 ) ;
#6177 = ORIENTED_EDGE ( 'NONE', *, *, #17258, .T. ) ;
#6178 = CARTESIAN_POINT ( 'NONE',  ( -56.48582580120559271, -9.153146818113595984, 0.000000000000000000 ) ) ;
#6179 = PRESENTATION_LAYER_ASSIGNMENT (  '', '', ( #8299 ) ) ;
#6180 = CARTESIAN_POINT ( 'NONE',  ( 200.0000000000000000, 39.99999999999999289, 20.00000000000007105 ) ) ;
#6181 = CARTESIAN_POINT ( 'NONE',  ( -208.1127848780264742, 67.17687982763172272, -10.60833733270698254 ) ) ;
#6182 = CARTESIAN_POINT ( 'NONE',  ( 151.7948205124836250, -33.23291073765550863, 0.000000000000000000 ) ) ;
#6183 = CARTESIAN_POINT ( 'NONE',  ( -626.9846540392142060, 75.00000000000000000, -34.99999999999999289 ) ) ;
#6184 = CARTESIAN_POINT ( 'NONE',  ( 199.9999999999998863, 18.69362872516077800, 3.425107952296777114 ) ) ;
#6185 = CARTESIAN_POINT ( 'NONE',  ( 200.0000000000000284, -18.85585617391987867, -2.482101612725928330 ) ) ;
#6186 = VECTOR ( 'NONE', #21766, 1000.000000000000114 ) ;
#6188 = CIRCLE ( 'NONE', #9578, 10.00000000000004796 ) ;
#6187 = CARTESIAN_POINT ( 'NONE',  ( -259.2033419157646676, 21.55415060305860209, -21.55415060305812602 ) ) ;
#6189 = CARTESIAN_POINT ( 'NONE',  ( 163.1118516004056573, -37.29075403953166301, 19.27778845539196695 ) ) ;
#6190 = CARTESIAN_POINT ( 'NONE',  ( -110.0414657791425412, 18.85420805687117607, 7.195370614811373855 ) ) ;
#6191 = CARTESIAN_POINT ( 'NONE',  ( -91.56559293963836410, 39.99999999999976552, 22.67402823373234000 ) ) ;
#6192 = CARTESIAN_POINT ( 'NONE',  ( 192.4448373802101173, -42.42640687116510634, 14.14213562375845257 ) ) ;
#6193 = CARTESIAN_POINT ( 'NONE',  ( -100.7734535825088358, -16.03295912088728770, 16.03295912088687913 ) ) ;
#6194 = CARTESIAN_POINT ( 'NONE',  ( -135.8532207217289738, -34.75652343174615311, 21.81201906317767936 ) ) ;
#6195 = CARTESIAN_POINT ( 'NONE',  ( 199.9999999999999432, 14.14213562373113398, -14.14213562373094923 ) ) ;
#6196 = CARTESIAN_POINT ( 'NONE',  ( 199.0255894194985729, -7.644541030299115469, 18.48648443203342140 ) ) ;
#6197 = ADVANCED_FACE ( 'NONE', ( #21045 ), #429, .T. ) ;
#6199 = CARTESIAN_POINT ( 'NONE',  ( 0.2972598230769956662, 39.99999999999983658, 54.33493731733950938 ) ) ;
#6198 = CARTESIAN_POINT ( 'NONE',  ( -213.1075012329537230, 9.698598906438871126, -66.26714140136179765 ) ) ;
#6200 = CARTESIAN_POINT ( 'NONE',  ( 91.82158438592158234, 44.40256751092319121, 12.16597498400105515 ) ) ;
#6201 = AXIS2_PLACEMENT_3D ( 'NONE', #12823, #10828, #8828 ) ;
#6202 = CARTESIAN_POINT ( 'NONE',  ( 17.65190074000982534, 48.50354960736528653, -14.05440436230914614 ) ) ;
#6203 = CARTESIAN_POINT ( 'NONE',  ( -280.0000000000000568, -20.00000000000006750, -40.00000000000002132 ) ) ;
#6204 = ORIENTED_EDGE ( 'NONE', *, *, #21012, .F. ) ;
#6205 = CARTESIAN_POINT ( 'NONE',  ( -86.96347745069644475, -21.75974354311651737, 0.000000000000000000 ) ) ;
#6206 = CARTESIAN_POINT ( 'NONE',  ( -3.856733984649761915, -43.19294614843409619, 17.89110409353252962 ) ) ;
#6207 = CARTESIAN_POINT ( 'NONE',  ( -213.1075012329537230, 53.71589010953660193, 40.00000000000002132 ) ) ;
#6208 = EDGE_CURVE ( 'NONE', #21682, #17794, #20647, .T. ) ;
#6209 = CIRCLE ( 'NONE', #705, 10.00000000000000000 ) ;
#6210 = ORIENTED_EDGE ( 'NONE', *, *, #3627, .T. ) ;
#6211 = CARTESIAN_POINT ( 'NONE',  ( 18.90082831370066074, 24.18116416851832540, -43.99399836018032062 ) ) ;
#6212 = CARTESIAN_POINT ( 'NONE',  ( 199.9999999999998579, -18.51658467707331113, 4.312655811444462195 ) ) ;
#6213 = CARTESIAN_POINT ( 'NONE',  ( 9.345847406404407920, -14.17927947630302832, 49.32890504404208798 ) ) ;
#6214 = CARTESIAN_POINT ( 'NONE',  ( 6.984886629791395407, 14.16808340396298149, -49.25486234614871961 ) ) ;
#6215 = CARTESIAN_POINT ( 'NONE',  ( 199.0147604500337764, -12.44374936594963899, -15.65999889774876941 ) ) ;
#6216 = CARTESIAN_POINT ( 'NONE',  ( -213.1075012329537230, 1.045191102001431893E-13, -13.71589010951911902 ) ) ;
#6217 = CARTESIAN_POINT ( 'NONE',  ( 141.7948666911895828, -30.38861427224640366, 12.58737617328886316 ) ) ;
#6218 = CARTESIAN_POINT ( 'NONE',  ( -121.8281150764609890, -10.16552078725288588, 22.46071699956211276 ) ) ;
#6219 = CARTESIAN_POINT ( 'NONE',  ( 163.1118516004056573, 37.29075403953132906, 19.27778845539275565 ) ) ;
#6220 = CARTESIAN_POINT ( 'NONE',  ( -208.1127848780265026, -15.00245453012673202, 0.000000000000000000 ) ) ;
#6222 = DIRECTION ( 'NONE',  ( 0.000000000000000000, 1.000000000000000000, 0.000000000000000000 ) ) ;
#6221 = CARTESIAN_POINT ( 'NONE',  ( -189.1288815661742433, 13.87115472124111193, -47.28031329128402405 ) ) ;
#6223 = CARTESIAN_POINT ( 'NONE',  ( -91.56559293963834989, 40.53558337403654832, 16.03295912088756481 ) ) ;
#6225 = VECTOR ( 'NONE', #20829, 1000.000000000000000 ) ;
#6224 = CARTESIAN_POINT ( 'NONE',  ( -105.3755690713226585, -18.24025645688355013, 40.00000000000002132 ) ) ;
#6226 = CARTESIAN_POINT ( 'NONE',  ( 192.4448373802100889, 19.99999999996064304, 2.449293598294708485E-15 ) ) ;
#6227 = CARTESIAN_POINT ( 'NONE',  ( 0.2972598230770030492, -39.99999999999987210, -14.33493731733975451 ) ) ;
#6228 = CARTESIAN_POINT ( 'NONE',  ( -192.9588430854689989, 38.51493924976929861, 38.51493924976947625 ) ) ;
#6229 = PRODUCT_DEFINITION ( 'UNKNOWN', '', #13400, #3119 ) ;
#6230 = CARTESIAN_POINT ( 'NONE',  ( 98.29820294269173075, 19.99999999998819433, -2.308575297063409524E-13 ) ) ;
#6231 = CARTESIAN_POINT ( 'NONE',  ( -105.3755690713226585, 15.38646221621820764, -41.18208027870583265 ) ) ;
#6232 = ORIENTED_EDGE ( 'NONE', *, *, #12307, .F. ) ;
#6233 = CARTESIAN_POINT ( 'NONE',  ( -30.26275506840324070, -27.08623969584595770, 29.48230279907789608 ) ) ;
#6234 = CARTESIAN_POINT ( 'NONE',  ( -93.01854144614468112, 8.553566903488155404, 20.65013722641577942 ) ) ;
#6235 = ORIENTED_EDGE ( 'NONE', *, *, #18921, .F. ) ;
#6236 = ORIENTED_EDGE ( 'NONE', *, *, #22005, .T. ) ;
#6237 = CARTESIAN_POINT ( 'NONE',  ( -105.3755690713226585, -41.18208027870589660, -15.38646221621809040 ) ) ;
#6238 = CARTESIAN_POINT ( 'NONE',  ( 2.332272417556284339, -44.41409500754987505, -24.49123061635837217 ) ) ;
#6239 = EDGE_CURVE ( 'NONE', #25051, #13683, #16823, .T. ) ;
#6240 = EDGE_LOOP ( 'NONE', ( #1237, #23465, #23167, #18848 ) ) ;
#6241 = CARTESIAN_POINT ( 'NONE',  ( 163.1118516004056573, -27.26290988616869626, 0.000000000000000000 ) ) ;
#6242 = CARTESIAN_POINT ( 'NONE',  ( -190.0000000000000000, -71.50000000000002842, 66.50000000000005684 ) ) ;
#6243 = EDGE_LOOP ( 'NONE', ( #984, #9603 ) ) ;
#6244 = CARTESIAN_POINT ( 'NONE',  ( 200.0000000000000000, 16.44874601624584187, 9.522804452304930223 ) ) ;
#6245 = LINE ( 'NONE', #14358, #17485 ) ;
#6246 = CARTESIAN_POINT ( 'NONE',  ( 57.59792236341147031, -1.722363176415032004, -1.722363176415048880 ) ) ;
#6247 = CARTESIAN_POINT ( 'NONE',  ( -188.8532066752250955, -43.29285604501843210, -17.93248812771291512 ) ) ;
#6248 = CARTESIAN_POINT ( 'NONE',  ( 170.2234770963711128, -39.99999999999991473, -24.55285855007201334 ) ) ;
#6249 = CARTESIAN_POINT ( 'NONE',  ( 0.2972598230769930017, 14.33493731733933352, 40.00000000000002132 ) ) ;
#6250 = CARTESIAN_POINT ( 'NONE',  ( -192.9588430854689989, 10.23066800230756712, -10.23066800230735396 ) ) ;
#6251 = CARTESIAN_POINT ( 'NONE',  ( 199.0210534451952924, 5.480999013853959489, 19.23967134089702569 ) ) ;
#6252 = CARTESIAN_POINT ( 'NONE',  ( 170.2234770963711128, -39.99999999999991473, -24.55285855007201334 ) ) ;
#6253 = CARTESIAN_POINT ( 'NONE',  ( 146.6084372240433709, -40.00000000000001421, 5.374981219216829587 ) ) ;
#6254 = CARTESIAN_POINT ( 'NONE',  ( 200.0000000000000000, 39.99999999999999289, 20.00000000000007105 ) ) ;
#6255 = CARTESIAN_POINT ( 'NONE',  ( -190.0000000000000000, -52.49999999999992895, -52.49999999999999289 ) ) ;
#6256 = CARTESIAN_POINT ( 'NONE',  ( 0.2972598230770100991, -38.42060263243686791, 38.42060263243645579 ) ) ;
#6257 = CARTESIAN_POINT ( 'NONE',  ( 170.2234770963711128, 24.55285855007190321, 0.000000000000000000 ) ) ;
#6258 = CARTESIAN_POINT ( 'NONE',  ( 91.82158438592159655, 12.16597498400028776, 44.40256751092339016 ) ) ;
#6259 = CARTESIAN_POINT ( 'NONE',  ( 126.3230993689412571, -11.72464299830483014, -28.30579214049048531 ) ) ;
#6260 = CARTESIAN_POINT ( 'NONE',  ( 7.340276806054861325, -49.28408872342596680, 14.17250878947614545 ) ) ;
#6261 = CARTESIAN_POINT ( 'NONE',  ( 192.4448373802101173, 40.00000000000026290, -19.99999999996018474 ) ) ;
#6262 = CARTESIAN_POINT ( 'NONE',  ( -259.2033419157646676, -1.564921101325656229E-13, 30.48217210827739621 ) ) ;
#6263 = CARTESIAN_POINT ( 'NONE',  ( -280.0000000000000568, 42.42640687119285303, -14.14213562373088351 ) ) ;
#6264 = CARTESIAN_POINT ( 'NONE',  ( -163.5815439473247181, -38.33196286486852955, -12.03526835478797175 ) ) ;
#6265 = CARTESIAN_POINT ( 'NONE',  ( -213.1075012329537230, 9.698598906450543566, -9.698598906450348167 ) ) ;
#6266 = CARTESIAN_POINT ( 'NONE',  ( 170.2234770963711128, -10.92277846919171935, -45.64576402573189995 ) ) ;
#6267 = ORIENTED_EDGE ( 'NONE', *, *, #25724, .F. ) ;
#6268 = CARTESIAN_POINT ( 'NONE',  ( -198.0356074513804572, -17.40982414986427429, -39.15871834505933435 ) ) ;
#6269 = CARTESIAN_POINT ( 'NONE',  ( -87.02160367299343591, -10.86259082821564981, -18.50714494492524054 ) ) ;
#6270 = CARTESIAN_POINT ( 'NONE',  ( 192.4448373802101173, -19.99999999996056843, -40.00000000000002132 ) ) ;
#6271 = CARTESIAN_POINT ( 'NONE',  ( -86.94486753505690046, 19.19951378115808893, 9.473579212373534730 ) ) ;
#6272 = CARTESIAN_POINT ( 'NONE',  ( -4.039451493210483690, -43.00522595894025812, 23.44932283416647323 ) ) ;
#6273 = ORIENTED_EDGE ( 'NONE', *, *, #11560, .F. ) ;
#6274 = EDGE_LOOP ( 'NONE', ( #21808, #4958, #19084, #13556 ) ) ;
#6275 = CARTESIAN_POINT ( 'NONE',  ( 200.0000000000000000, 18.57749355353195497, -3.991677856843532712 ) ) ;
#6276 = CARTESIAN_POINT ( 'NONE',  ( -65.65550967573733487, -11.16467289560236509, -24.04430752631839496 ) ) ;
#6277 = CARTESIAN_POINT ( 'NONE',  ( 17.65190073994290643, 14.05440436231865320, 48.50354960737508492 ) ) ;
#6278 = EDGE_LOOP ( 'NONE', ( #11152, #13148 ) ) ;
#6279 = VERTEX_POINT ( 'NONE', #24780 ) ;
#6280 = DIRECTION ( 'NONE',  ( -1.000000000000000000, -0.000000000000000000, -0.000000000000000000 ) ) ;
#6281 = CARTESIAN_POINT ( 'NONE',  ( 199.0101504891794946, -4.065683697617192394, -19.58013257009994135 ) ) ;
#6282 = CARTESIAN_POINT ( 'NONE',  ( -196.0240759113458466, -44.60678620512906889, 24.63338926175166321 ) ) ;
#6283 = CARTESIAN_POINT ( 'NONE',  ( 169.9999999999999716, -115.7889608577475542, -82.49999999999998579 ) ) ;
#6284 = CARTESIAN_POINT ( 'NONE',  ( 130.8568914410475372, 8.880724697947696879E-14, -5.949712681206690945 ) ) ;
#6285 = CARTESIAN_POINT ( 'NONE',  ( 136.1360204305621266, -3.419521671106983309E-13, 35.03383547441296741 ) ) ;
#6286 = CARTESIAN_POINT ( 'NONE',  ( -635.0888434903920370, 27.60293145401818649, 28.95600705801621544 ) ) ;
#6287 = CARTESIAN_POINT ( 'NONE',  ( -369.0000000000000568, -4.857225732735059864E-14, 0.000000000000000000 ) ) ;
#6288 = CARTESIAN_POINT ( 'NONE',  ( 199.0216355752872914, 4.216131936211398035, 19.55614661669859444 ) ) ;
#6289 = CARTESIAN_POINT ( 'NONE',  ( -190.7345856381787144, 13.94676320010972859, 47.78725959878661200 ) ) ;
#6290 = CARTESIAN_POINT ( 'NONE',  ( 23.17367289775331329, -13.81211338457429427, -46.88342923876911073 ) ) ;
#6291 = CARTESIAN_POINT ( 'NONE',  ( -86.96347745069644475, -12.89780903124395195, -12.89780903124416511 ) ) ;
#6292 = CARTESIAN_POINT ( 'NONE',  ( -103.9474983244999180, 19.92928099173798628, -8.577167319634817488 ) ) ;
#6293 = CARTESIAN_POINT ( 'NONE',  ( 170.2234770963711128, -10.92277846919202666, 10.92277846919193962 ) ) ;
#6294 = DIRECTION ( 'NONE',  ( 0.000000000000000000, -1.000000000000000000, 0.000000000000000000 ) ) ;
#6295 = CARTESIAN_POINT ( 'NONE',  ( 163.1118516004056573, 19.27778845538753316, 19.27778845538783870 ) ) ;
#6296 = CARTESIAN_POINT ( 'NONE',  ( 146.6084372240433709, 34.62501878078307982, 40.00000000000002132 ) ) ;
#6297 = CARTESIAN_POINT ( 'NONE',  ( 184.8905102610680444, 14.79361573936396113, -14.79361573936377461 ) ) ;
#6298 = CARTESIAN_POINT ( 'NONE',  ( -208.1127848780264742, -55.00245453010926866, 40.00000000000002132 ) ) ;
#6299 = CARTESIAN_POINT ( 'NONE',  ( -105.4741150117383057, 8.366608964593771347, 19.60045294982731789 ) ) ;
#6300 = CARTESIAN_POINT ( 'NONE',  ( -280.0000000000000000, 1.605030083646939673E-13, -20.00000000000001421 ) ) ;
#6301 = CARTESIAN_POINT ( 'NONE',  ( 19.06497207195979726, 38.31983398719629719, -18.24870850772750686 ) ) ;
#6302 = CARTESIAN_POINT ( 'NONE',  ( -192.9588430854689989, 14.46834944099965981, 0.000000000000000000 ) ) ;
#6303 = ORIENTED_EDGE ( 'NONE', *, *, #15250, .T. ) ;
#6305 = VERTEX_POINT ( 'NONE', #13685 ) ;
#6304 = EDGE_CURVE ( 'NONE', #7462, #10709, #25090, .T. ) ;
#6306 = CARTESIAN_POINT ( 'NONE',  ( 57.59792236341147031, -2.435789363418150444, 0.000000000000000000 ) ) ;
#6307 = CARTESIAN_POINT ( 'NONE',  ( 156.1979191798868669, 11.34289806466567363, 27.38417834433186471 ) ) ;
#6308 = CARTESIAN_POINT ( 'NONE',  ( -162.0762913951020892, 29.48230308784799902, -29.48230308784730980 ) ) ;
#6309 = CARTESIAN_POINT ( 'NONE',  ( -105.4293522941955814, -20.05597878317656679, -7.324187428710191128 ) ) ;
#6310 = CARTESIAN_POINT ( 'NONE',  ( 163.1118516004056573, -27.26290988616869626, 0.000000000000000000 ) ) ;
#6311 = CARTESIAN_POINT ( 'NONE',  ( -163.5815475691942993, 18.59457173339185232, 35.61501186087235027 ) ) ;
#6312 = CARTESIAN_POINT ( 'NONE',  ( 200.0000000000000000, 18.87777001997802628, 2.191952217553565507 ) ) ;
#6313 = CARTESIAN_POINT ( 'NONE',  ( 199.9999999999999432, -17.32226549516795089, -7.848194971284391031 ) ) ;
#6314 = CARTESIAN_POINT ( 'NONE',  ( -56.48582580120559982, 50.09629031063956717, 6.472252184284792875 ) ) ;
#6315 = CARTESIAN_POINT ( 'NONE',  ( 19.06497207195982568, -38.31983398719592770, -38.31983398719660272 ) ) ;
#6316 = CARTESIAN_POINT ( 'NONE',  ( -110.0305084685578976, 18.59638600693097032, 7.798154251660106340 ) ) ;
#6317 = CARTESIAN_POINT ( 'NONE',  ( 14.38125909742180220, 40.00000000000017764, -15.17850393972591760 ) ) ;
#6318 = CARTESIAN_POINT ( 'NONE',  ( -30.26275506840324070, -29.48230279907817675, 27.08623969584564151 ) ) ;
#6319 = CARTESIAN_POINT ( 'NONE',  ( 170.2234770963711128, -17.36149277827010096, 17.36149277826970660 ) ) ;
#6320 = CARTESIAN_POINT ( 'NONE',  ( 170.2234770963711128, -17.36149277826985937, -17.36149277826995174 ) ) ;
#6321 = CARTESIAN_POINT ( 'NONE',  ( -30.26275506840324070, -29.48230279907780016, -27.08623969584605362 ) ) ;
#6322 = CARTESIAN_POINT ( 'NONE',  ( 199.0254345294016503, -6.947174024697130967, 18.76024293726333170 ) ) ;
#6323 = CIRCLE ( 'NONE', #1660, 20.00000000000001421 ) ;
#6325 = CARTESIAN_POINT ( 'NONE',  ( 146.6084372240433993, 5.715592784339989804E-15, 5.374981219216972583 ) ) ;
#6324 = CARTESIAN_POINT ( 'NONE',  ( -56.48582580120559982, 50.09629031063956717, 6.472252184284792875 ) ) ;
#6326 = CARTESIAN_POINT ( 'NONE',  ( 151.7948205124836534, 33.06932595376333239, 23.49921654116065284 ) ) ;
#6327 = CARTESIAN_POINT ( 'NONE',  ( 23.58679727196860298, 46.73132340480132996, -13.78527791281944737 ) ) ;
#6328 = CARTESIAN_POINT ( 'NONE',  ( -192.9588430854690273, 54.46834944098218756, -40.00000000000002132 ) ) ;
#6329 = CARTESIAN_POINT ( 'NONE',  ( -280.0000000000000000, -14.14213562373098831, -14.14213562373098654 ) ) ;
#6330 = CARTESIAN_POINT ( 'NONE',  ( 146.6084372240433993, -24.48358557860319706, -24.48358557860330720 ) ) ;
#6331 = CARTESIAN_POINT ( 'NONE',  ( -4.027137536849500599, -46.99492183298355030, 13.82877337592804956 ) ) ;
#6332 = CARTESIAN_POINT ( 'NONE',  ( -192.9588430854690273, 54.46834944101718889, 40.00000000000002132 ) ) ;
#6333 = EDGE_LOOP ( 'NONE', ( #11996, #19300, #863, #22353, #19983 ) ) ;
#6334 = CARTESIAN_POINT ( 'NONE',  ( -2.652172544013607247, 23.73409167602034131, -43.38951316025613636 ) ) ;
#6335 = CARTESIAN_POINT ( 'NONE',  ( 130.8568914410475372, -24.07718906447222551, -24.07718906447233209 ) ) ;
#6336 = CARTESIAN_POINT ( 'NONE',  ( -317.0000000000000568, -4.857225732735059864E-14, 0.000000000000000000 ) ) ;
#6337 = CARTESIAN_POINT ( 'NONE',  ( -4.061681315507500223, 23.44498947467636185, -42.99867639910915074 ) ) ;
#6338 = CARTESIAN_POINT ( 'NONE',  ( 199.0079861221352360, 1.294590733001960592, -19.95474696286750671 ) ) ;
#6340 = B_SPLINE_CURVE_WITH_KNOTS ( 'NONE', 3,
 ( #14878, #18746, #20348, #8767, #527, #8632 ),
 .UNSPECIFIED., .F., .F.,
 ( 4, 2, 4 ),
 ( 0.3689590070116580689, 0.3867117631979620773, 0.4044645193949217288 ),
 .UNSPECIFIED. ) ;
#6339 = CARTESIAN_POINT ( 'NONE',  ( -726.9846540392142060, -52.49999999999991473, 82.49999999999998579 ) ) ;
#6341 = LINE ( 'NONE', #4370, #17656 ) ;
#6342 = CARTESIAN_POINT ( 'NONE',  ( -188.8948648269077637, -17.93710299892617854, 43.30399732969031135 ) ) ;
#6343 = VECTOR ( 'NONE', #6138, 1000.000000000000114 ) ;
#6344 = CARTESIAN_POINT ( 'NONE',  ( 192.4448373802101173, -42.42640687122053578, -14.14213562370360577 ) ) ;
#6345 = CARTESIAN_POINT ( 'NONE',  ( -93.12335834970889437, -22.67402823373193499, 0.000000000000000000 ) ) ;
#6347 = CARTESIAN_POINT ( 'NONE',  ( -192.9588430854690273, 38.51493924976913519, 18.05360324515490333 ) ) ;
#6346 = CARTESIAN_POINT ( 'NONE',  ( -195.5008451366929307, 18.44412755962871131, -44.52806290063609396 ) ) ;
#6348 = CARTESIAN_POINT ( 'NONE',  ( -30.26275506840325136, 29.48230279907760121, 27.08623969584625613 ) ) ;
#6349 = CARTESIAN_POINT ( 'NONE',  ( 170.2234770963711128, -15.44714144992812876, -2.449293598294708485E-15 ) ) ;
#6350 = CARTESIAN_POINT ( 'NONE',  ( 146.6084372240433709, 5.374981219216996564, 40.00000000000002132 ) ) ;
#6351 = CARTESIAN_POINT ( 'NONE',  ( -198.0356074513804572, 1.247057299367198800E-13, -15.37879056873070560 ) ) ;
#6352 = CARTESIAN_POINT ( 'NONE',  ( 192.4448373802100889, 14.14213562370310662, 14.14213562370312438 ) ) ;
#6353 = CARTESIAN_POINT ( 'NONE',  ( -93.01741312761465963, 20.82169463873246684, -8.169811846372676101 ) ) ;
#6354 = CARTESIAN_POINT ( 'NONE',  ( -208.1127848780264742, -38.89260858015704514, -38.89260858015768463 ) ) ;
#6355 = CARTESIAN_POINT ( 'NONE',  ( 91.82158438592156813, 40.45024623143950038, 16.11829626348447420 ) ) ;
#6356 = ORIENTED_EDGE ( 'NONE', *, *, #14380, .F. ) ;
#6357 = CARTESIAN_POINT ( 'NONE',  ( 170.2234770963711128, -45.64576402573183600, 10.92277846919191653 ) ) ;
#6358 = B_SPLINE_CURVE_WITH_KNOTS ( 'NONE', 3,
 ( #19455, #13586, #15455, #19584, #1115, #17333, #1374, #25467, #3492, #9605, #4170, #8264, #6145, #10137, #9739, #14256, #8137, #12264, #14127, #10273, #22394, #23969, #26, #5745, #22255, #16253, #5882 ),
 .UNSPECIFIED., .F., .F.,
 ( 4, 2, 1, 1, 2, 2, 2, 2, 2, 2, 2, 2, 1, 2, 4 ),
 ( -5.999999999696028456E-08, 0.0002171475752860094221, 0.0004343551505720157774, 0.0008687703011440240427, 0.001737600602288037104, 0.003475261204576063443, 0.006950582409152111785, 0.01390122481830420934, 0.02085186722745630342, 0.02432718843203235046, 0.02606484903432037745, 0.02693367933546438747, 0.02736809448603639422, 0.02758530206132240106, 0.02780250963660840791 ),
 .UNSPECIFIED. ) ;
#6359 = CARTESIAN_POINT ( 'NONE',  ( -93.01741312761399172, 8.946232117102187686, 20.50009083249028663 ) ) ;
#6360 = CARTESIAN_POINT ( 'NONE',  ( 91.82158438592159655, -16.11829626346147393, 16.11829626346132116 ) ) ;
#6361 = CARTESIAN_POINT ( 'NONE',  ( -3.786831587084357853, -43.07879808621907358, -23.50387725151980689 ) ) ;
#6362 = VERTEX_POINT ( 'NONE', #5320 ) ;
#6363 = CARTESIAN_POINT ( 'NONE',  ( -575.0231298121445889, 90.00000000000000000, 24.99999999999828759 ) ) ;
#6364 = CARTESIAN_POINT ( 'NONE',  ( -199.9999999999999432, -44.88127304973825460, 30.70179486994645401 ) ) ;
#6365 = CIRCLE ( 'NONE', #22104, 15.00000000000000000 ) ;
#6366 = ORIENTED_EDGE ( 'NONE', *, *, #5910, .T. ) ;
#6367 = CARTESIAN_POINT ( 'NONE',  ( 200.0000000000001137, 18.84395317400427317, -2.458366139920278304 ) ) ;
#6368 = CARTESIAN_POINT ( 'NONE',  ( 4.990270234119173587, 14.15117691407241196, -49.14367003637708819 ) ) ;
#6369 = CARTESIAN_POINT ( 'NONE',  ( -185.5190930961063316, -42.39056500339492572, -17.55874694107016154 ) ) ;
#6370 = EDGE_CURVE ( 'NONE', #21146, #2419, #9439, .T. ) ;
#6371 = CARTESIAN_POINT ( 'NONE',  ( -208.1127848780264742, -40.00000000000025580, 55.00245453014408525 ) ) ;
#6372 = CARTESIAN_POINT ( 'NONE',  ( 151.7948205124836534, 6.767089262349056611, 40.00000000000002132 ) ) ;
#6373 = CARTESIAN_POINT ( 'NONE',  ( -192.9588430854690273, -18.05360324515400094, -38.51493924976961836 ) ) ;
#6374 = CARTESIAN_POINT ( 'NONE',  ( 199.0261461916015264, -10.84957391917088110, 16.80813345823991867 ) ) ;
#6375 = ADVANCED_FACE ( 'NONE', ( #3579 ), #5452, .F. ) ;
#6376 = CARTESIAN_POINT ( 'NONE',  ( -280.0000000000000568, -40.00000000000014211, 19.99999999999987210 ) ) ;
#6377 = CARTESIAN_POINT ( 'NONE',  ( -162.0762913951021176, 39.99999999999998579, 1.694272876828463614 ) ) ;
#6378 = CARTESIAN_POINT ( 'NONE',  ( -93.12335834970892279, 16.03295912088714203, -16.03295912088699282 ) ) ;
#6379 = DIRECTION ( 'NONE',  ( -1.000000000000000000, 1.836970198721030181E-16, 0.000000000000000000 ) ) ;
#6380 = EDGE_CURVE ( 'NONE', #5488, #4791, #9064, .T. ) ;
#6381 = CARTESIAN_POINT ( 'NONE',  ( 57.59792236341148453, -37.56421063658185489, -40.00000000000002132 ) ) ;
#6382 = EDGE_CURVE ( 'NONE', #23789, #13093, #9313, .T. ) ;
#6383 = CARTESIAN_POINT ( 'NONE',  ( 146.6084372240433993, -3.800685668858652999, 3.800685668858636568 ) ) ;
#6384 = CARTESIAN_POINT ( 'NONE',  ( -56.48582580120559271, -1.062504017861011783E-13, 9.153146818113587102 ) ) ;
#6385 = VECTOR ( 'NONE', #24052, 1000.000000000000000 ) ;
#6386 = DIRECTION ( 'NONE',  ( -1.836970198721030427E-16, 1.000000000000000000, 4.182618615277681568E-16 ) ) ;
#6387 = CARTESIAN_POINT ( 'NONE',  ( 184.8905102610680444, 39.99999999999983658, 20.92133201514485563 ) ) ;
#6388 = CARTESIAN_POINT ( 'NONE',  ( -213.1075012329537230, -2.291445344039133686E-13, 53.71589010951915100 ) ) ;
#6389 = CARTESIAN_POINT ( 'NONE',  ( 199.0262408397048262, -11.66336112630027877, 16.25405011469380057 ) ) ;
#6390 = CARTESIAN_POINT ( 'NONE',  ( -575.0231298121466352, 75.00000000000000000, -35.00000000000203926 ) ) ;
#6391 = CARTESIAN_POINT ( 'NONE',  ( -114.7469200037860162, -17.46524160228793576, 13.55861222482207396 ) ) ;
#6392 = CARTESIAN_POINT ( 'NONE',  ( 192.4448373802101173, -14.14213562370283128, -42.42640687122081999 ) ) ;
#6393 = VERTEX_POINT ( 'NONE', #3082 ) ;
#6394 = CARTESIAN_POINT ( 'NONE',  ( -77.90255099906769942, 20.29001641120658306, -8.064892378658445438 ) ) ;
#6395 = CARTESIAN_POINT ( 'NONE',  ( 144.1620285550791607, 30.21661402164566823, -12.51613133675856382 ) ) ;
#6396 = CARTESIAN_POINT ( 'NONE',  ( 91.82158438592159655, -22.79471317813468545, -2.449293598294708485E-15 ) ) ;
#6397 = CARTESIAN_POINT ( 'NONE',  ( -175.9235632129417866, -39.35891845656527721, 21.03681927447506794 ) ) ;
#6398 = CARTESIAN_POINT ( 'NONE',  ( -213.1075012329537230, 13.71589010951907994, 0.000000000000000000 ) ) ;
#6399 = SHAPE_REPRESENTATION_RELATIONSHIP ( 'NONE' , 'NONE' ,  #21040, #11792 ) ;
#6400 = ORIENTED_EDGE ( 'NONE', *, *, #24197, .F. ) ;
#6401 = ORIENTED_EDGE ( 'NONE', *, *, #20013, .F. ) ;
#6402 = CARTESIAN_POINT ( 'NONE',  ( 200.0000000000000000, -9.238661743929142744, 16.61727401759219092 ) ) ;
#6403 = CARTESIAN_POINT ( 'NONE',  ( -89.91646883266056989, 8.407637968211338020, -20.29783361036653133 ) ) ;
#6404 = CARTESIAN_POINT ( 'NONE',  ( 22.17571259162627939, 23.59965736304510742, 43.20787961118917764 ) ) ;
#6405 = ORIENTED_EDGE ( 'NONE', *, *, #18921, .T. ) ;
#6406 = VERTEX_POINT ( 'NONE', #11682 ) ;
#6407 = CARTESIAN_POINT ( 'NONE',  ( 192.4448373802101173, -42.42640687122073473, 14.14213562370301780 ) ) ;
#6408 = CARTESIAN_POINT ( 'NONE',  ( 199.0255278052971732, -18.60593281614774952, 7.356242102916651149 ) ) ;
#6409 = CARTESIAN_POINT ( 'NONE',  ( -110.0368417077423118, 7.441767003019926108, 18.74474319002354505 ) ) ;
#6410 = CARTESIAN_POINT ( 'NONE',  ( 57.59792236341147031, -1.722363176415032004, -1.722363176415048880 ) ) ;
#6411 = AXIS2_PLACEMENT_3D ( 'NONE', #24230, #12373, #144 ) ;
#6412 = CARTESIAN_POINT ( 'NONE',  ( -86.96347745069644475, 41.18208027870598187, -15.38646221621779731 ) ) ;
#6413 = FACE_OUTER_BOUND ( 'NONE', #17007, .T. ) ;
#6414 = CARTESIAN_POINT ( 'NONE',  ( -96.94449363885368598, -8.590991631001321238, -20.74048850981448311 ) ) ;
#6415 =( BOUNDED_SURFACE ( )  B_SPLINE_SURFACE ( 3, 3, ( 
 ( #2488, #24985, #25115, #14457, #18850, #8604, #24579, #22981, #22587, #8735, #10601, #4759, #6735, #2762, #8465, #12863, #20981, #10470, #10869, #10739, #4364, #6335, #18445, #16583, #24845, #22456, #20722, #16714, #2228, #629 ),
 ( #12455, #220, #20582, #22713, #24716, #4625, #14718, #8333, #6470, #14584, #18985, #6598, #12592, #763, #12726, #4235, #2629, #16854, #12324, #20453, #2356, #16457, #3394, #21374, #1273, #19111, #15237, #3269, #5395, #9506 ),
 ( #7127, #11127, #1021, #23614, #9257, #25500, #15109, #21495, #12994, #11490, #23370, #17109, #17363, #1405, #19489, #25375, #9378, #15369, #6865, #5145, #3143, #9122, #13251, #14981, #7247, #11246, #19363, #23492, #5019, #17611 ),
 ( #23115, #11001, #894, #4887, #13124, #19620, #1153, #9004, #17487, #11369, #5266, #25629, #13369, #7375, #21245, #15486, #17234, #21619, #2893, #13497, #21116, #25241, #6993, #23244, #3019, #19240, #4433, #13889, #3523, #20525 ),
 ( #25755, #2294, #3794, #7761, #20658, #22156, #12032, #14528, #10405, #21749, #12526, #5919, #6412, #19882, #2430, #7503, #14027, #11897, #15613, #20020, #5518, #18010, #15873, #22023, #18522, #10541, #25884, #3936, #1801, #9640 ),
 ( #302, #9904, #16527, #8405, #22661, #1665, #24655, #23737, #21878, #13622, #11624, #7627, #17743, #19745, #3656, #26155, #1535, #5782, #7899, #15740, #23870, #16018, #5645, #24143, #13751, #11763, #9773, #17873, #26024, #24000 ),
 ( #22920, #9071, #2838, #10812, #5089, #18923, #3089, #10948, #836, #18652, #21316, #24924, #13193, #15186, #6807, #13071, #4570, #707, #15054, #17178, #438, #967, #6936, #8543, #4832, #8811, #25313, #4699, #23183, #2707 ) ),
 .UNSPECIFIED., .T., .F., .F. ) 
 B_SPLINE_SURFACE_WITH_KNOTS ( ( 4, 3, 4 ),
 ( 4, 2, 2, 2, 2, 2, 2, 2, 2, 2, 2, 2, 2, 2, 4 ),
 ( 0.000000000000000000, 0.5000000000000000000, 1.000000000000000000 ),
 ( 0.000000000000000000, 0.1357259735107005372, 0.1651108541090157700, 0.1944957347073310028, 0.3598804999793158710, 0.3867117631979620773, 0.4135430264166082281, 0.5789277916885930964, 0.6062785021374117456, 0.6336292125862302838, 0.8508620842112317728, 0.8814014469398914198, 0.9119408096685510667, 0.9559704048342755334, 1.000000000000000000 ),
 .UNSPECIFIED. ) 
 GEOMETRIC_REPRESENTATION_ITEM ( )  RATIONAL_B_SPLINE_SURFACE ( (
 ( 1.000000000000000000, 1.000000000000000000, 1.000000000000000000, 1.000000000000000000, 1.000000000000000000, 1.000000000000000000, 1.000000000000000000, 1.000000000000000000, 1.000000000000000000, 1.000000000000000000, 1.000000000000000000, 1.000000000000000000, 1.000000000000000000, 1.000000000000000000, 1.000000000000000000, 1.000000000000000000, 1.000000000000000000, 1.000000000000000000, 1.000000000000000000, 1.000000000000000000, 1.000000000000000000, 1.000000000000000000, 1.000000000000000000, 1.000000000000000000, 1.000000000000000000, 1.000000000000000000, 1.000000000000000000, 1.000000000000000000, 1.000000000000000000, 1.000000000000000000),
 ( 0.3333333333333333703, 0.3333333333333333703, 0.3333333333333333703, 0.3333333333333333703, 0.3333333333333333703, 0.3333333333333333703, 0.3333333333333333703, 0.3333333333333333703, 0.3333333333333333703, 0.3333333333333333703, 0.3333333333333333703, 0.3333333333333333703, 0.3333333333333333703, 0.3333333333333333703, 0.3333333333333333703, 0.3333333333333333703, 0.3333333333333333703, 0.3333333333333333703, 0.3333333333333333703, 0.3333333333333333703, 0.3333333333333333703, 0.3333333333333333703, 0.3333333333333333703, 0.3333333333333333703, 0.3333333333333333703, 0.3333333333333333703, 0.3333333333333333703, 0.3333333333333333703, 0.3333333333333333703, 0.3333333333333333703),
 ( 0.3333333333333333703, 0.3333333333333333703, 0.3333333333333333703, 0.3333333333333333703, 0.3333333333333333703, 0.3333333333333333703, 0.3333333333333333703, 0.3333333333333333703, 0.3333333333333333703, 0.3333333333333333703, 0.3333333333333333703, 0.3333333333333333703, 0.3333333333333333703, 0.3333333333333333703, 0.3333333333333333703, 0.3333333333333333703, 0.3333333333333333703, 0.3333333333333333703, 0.3333333333333333703, 0.3333333333333333703, 0.3333333333333333703, 0.3333333333333333703, 0.3333333333333333703, 0.3333333333333333703, 0.3333333333333333703, 0.3333333333333333703, 0.3333333333333333703, 0.3333333333333333703, 0.3333333333333333703, 0.3333333333333333703),
 ( 1.000000000000000000, 1.000000000000000000, 1.000000000000000000, 1.000000000000000000, 1.000000000000000000, 1.000000000000000000, 1.000000000000000000, 1.000000000000000000, 1.000000000000000000, 1.000000000000000000, 1.000000000000000000, 1.000000000000000000, 1.000000000000000000, 1.000000000000000000, 1.000000000000000000, 1.000000000000000000, 1.000000000000000000, 1.000000000000000000, 1.000000000000000000, 1.000000000000000000, 1.000000000000000000, 1.000000000000000000, 1.000000000000000000, 1.000000000000000000, 1.000000000000000000, 1.000000000000000000, 1.000000000000000000, 1.000000000000000000, 1.000000000000000000, 1.000000000000000000),
 ( 0.3333333333333333703, 0.3333333333333333703, 0.3333333333333333703, 0.3333333333333333703, 0.3333333333333333703, 0.3333333333333333703, 0.3333333333333333703, 0.3333333333333333703, 0.3333333333333333703, 0.3333333333333333703, 0.3333333333333333703, 0.3333333333333333703, 0.3333333333333333703, 0.3333333333333333703, 0.3333333333333333703, 0.3333333333333333703, 0.3333333333333333703, 0.3333333333333333703, 0.3333333333333333703, 0.3333333333333333703, 0.3333333333333333703, 0.3333333333333333703, 0.3333333333333333703, 0.3333333333333333703, 0.3333333333333333703, 0.3333333333333333703, 0.3333333333333333703, 0.3333333333333333703, 0.3333333333333333703, 0.3333333333333333703),
 ( 0.3333333333333333703, 0.3333333333333333703, 0.3333333333333333703, 0.3333333333333333703, 0.3333333333333333703, 0.3333333333333333703, 0.3333333333333333703, 0.3333333333333333703, 0.3333333333333333703, 0.3333333333333333703, 0.3333333333333333703, 0.3333333333333333703, 0.3333333333333333703, 0.3333333333333333703, 0.3333333333333333703, 0.3333333333333333703, 0.3333333333333333703, 0.3333333333333333703, 0.3333333333333333703, 0.3333333333333333703, 0.3333333333333333703, 0.3333333333333333703, 0.3333333333333333703, 0.3333333333333333703, 0.3333333333333333703, 0.3333333333333333703, 0.3333333333333333703, 0.3333333333333333703, 0.3333333333333333703, 0.3333333333333333703),
 ( 1.000000000000000000, 1.000000000000000000, 1.000000000000000000, 1.000000000000000000, 1.000000000000000000, 1.000000000000000000, 1.000000000000000000, 1.000000000000000000, 1.000000000000000000, 1.000000000000000000, 1.000000000000000000, 1.000000000000000000, 1.000000000000000000, 1.000000000000000000, 1.000000000000000000, 1.000000000000000000, 1.000000000000000000, 1.000000000000000000, 1.000000000000000000, 1.000000000000000000, 1.000000000000000000, 1.000000000000000000, 1.000000000000000000, 1.000000000000000000, 1.000000000000000000, 1.000000000000000000, 1.000000000000000000, 1.000000000000000000, 1.000000000000000000, 1.000000000000000000) ) ) 
 REPRESENTATION_ITEM ( '' )  SURFACE ( )  );
#6416 = CARTESIAN_POINT ( 'NONE',  ( 151.7948205124836250, 1.012150473917908975E-13, -6.767089262349031742 ) ) ;
#6417 = CARTESIAN_POINT ( 'NONE',  ( -135.8532207217289738, 39.99999999999990763, 9.153146818113990335 ) ) ;
#6418 = CARTESIAN_POINT ( 'NONE',  ( -651.2040234678420347, 35.86671673404443084, 17.72972231506208018 ) ) ;
#6419 = DIRECTION ( 'NONE',  ( 1.000000000000000000, 1.836970198721030181E-16, 0.000000000000000000 ) ) ;
#6420 = CARTESIAN_POINT ( 'NONE',  ( 199.0053389886216451, 13.17958853561047228, -15.05032186847045672 ) ) ;
#6421 = CARTESIAN_POINT ( 'NONE',  ( -173.7925187078237172, 20.60915802531267715, 38.69492115335059879 ) ) ;
#6422 = CARTESIAN_POINT ( 'NONE',  ( -213.1075012329537230, -37.98287015391257881, 18.58567234101111509 ) ) ;
#6423 = CARTESIAN_POINT ( 'NONE',  ( -200.0000000000000000, -66.50000000000001421, -66.50000000000005684 ) ) ;
#6424 = CARTESIAN_POINT ( 'NONE',  ( -105.3755690713226585, 15.38646221621762678, 41.18208027870604582 ) ) ;
#6425 = PLANE ( 'NONE',  #12130 ) ;
#6426 = CARTESIAN_POINT ( 'NONE',  ( 170.2234770963711128, 17.36149277827028925, -39.20704971665377059 ) ) ;
#6427 = CARTESIAN_POINT ( 'NONE',  ( -660.9877162221778235, 44.22876715792673963, 8.378995438794239803 ) ) ;
#6428 = CARTESIAN_POINT ( 'NONE',  ( -162.0762913951020892, -1.694272876828353702, 0.000000000000000000 ) ) ;
#6429 = CARTESIAN_POINT ( 'NONE',  ( -280.0000000000000000, -14.14213562373118549, 14.14213562373078936 ) ) ;
#6430 = CARTESIAN_POINT ( 'NONE',  ( 200.0000000000000000, 20.00000000000013856, 40.00000000000002132 ) ) ;
#6431 = CARTESIAN_POINT ( 'NONE',  ( -109.1264249741457917, -13.72187187121247831, 33.12752917270314157 ) ) ;
#6432 = CARTESIAN_POINT ( 'NONE',  ( -56.48582580120560692, 39.99999999999991473, 9.153146818114004546 ) ) ;
#6433 = CARTESIAN_POINT ( 'NONE',  ( 199.0072917153253229, 3.369890617853546377, -19.72057389405671657 ) ) ;
#6434 = CARTESIAN_POINT ( 'NONE',  ( 110.0479209278585842, -9.419601331808975075, 22.74092928740035191 ) ) ;
#6435 = ORIENTED_EDGE ( 'NONE', *, *, #6869, .T. ) ;
#6436 = EDGE_LOOP ( 'NONE', ( #22771, #14509, #17547, #288 ) ) ;
#6437 = EDGE_LOOP ( 'NONE', ( #20552, #22778 ) ) ;
#6438 = CARTESIAN_POINT ( 'NONE',  ( -208.1127848780265026, 15.00245453012665564, 0.000000000000000000 ) ) ;
#6439 = CARTESIAN_POINT ( 'NONE',  ( 153.3020327024399023, 11.77299484472913527, 28.42252382389429499 ) ) ;
#6440 = AXIS2_PLACEMENT_3D ( 'NONE', #1341, #17551, #15184 ) ;
#6441 = CARTESIAN_POINT ( 'NONE',  ( -30.26275506840323715, 29.48230279907829754, -29.48230279907758344 ) ) ;
#6442 = CARTESIAN_POINT ( 'NONE',  ( 90.68848816921392597, 21.47805809169735269, -8.337973099072662819 ) ) ;
#6443 = DIRECTION ( 'NONE',  ( 0.000000000000000000, 0.000000000000000000, 1.000000000000000000 ) ) ;
#6444 = CARTESIAN_POINT ( 'NONE',  ( -196.0240701931630269, 14.12332411430307921, -48.96019555158512304 ) ) ;
#6445 = CARTESIAN_POINT ( 'NONE',  ( 199.9999999999998863, -2.943496653232010374, -18.77345647985907462 ) ) ;
#6446 = CARTESIAN_POINT ( 'NONE',  ( 200.0000000000000284, 12.52648961991985033, -14.29954643281654469 ) ) ;
#6447 = CARTESIAN_POINT ( 'NONE',  ( -135.8532207217289738, -34.75652343174584757, -21.81201906317816253 ) ) ;
#6448 = CARTESIAN_POINT ( 'NONE',  ( 14.38125909742181285, -10.73282306404712472, -10.73282306404731301 ) ) ;
#6449 = CARTESIAN_POINT ( 'NONE',  ( -114.7831797584708085, 22.13429202244894256, -0.1329151402176787233 ) ) ;
#6450 = CARTESIAN_POINT ( 'NONE',  ( 136.1360204305621551, 39.99999999999968026, 35.03383547441337953 ) ) ;
#6451 = CARTESIAN_POINT ( 'NONE',  ( 57.59792236341147031, -26.56190807104712448, 30.00663442387673285 ) ) ;
#6452 = EDGE_CURVE ( 'NONE', #8800, #22947, #6694, .T. ) ;
#6453 = CARTESIAN_POINT ( 'NONE',  ( 12.01676479903290939, 14.17570730777196530, 49.30523874212529023 ) ) ;
#6454 = CARTESIAN_POINT ( 'NONE',  ( -114.4364955367314991, -8.644468109207263495, -20.04994829327655737 ) ) ;
#6455 = CARTESIAN_POINT ( 'NONE',  ( -56.48582580120558561, -50.09629031063963112, -6.472252184284449150 ) ) ;
#6456 = CARTESIAN_POINT ( 'NONE',  ( 199.0118448083844385, 18.52953444905362090, 7.521846903409109331 ) ) ;
#6458 = CARTESIAN_POINT ( 'NONE',  ( -135.8532207217289738, -1.351063376314938213E-13, 30.84685318188645553 ) ) ;
#6457 = CARTESIAN_POINT ( 'NONE',  ( 192.4448373802100889, 14.14213562370330379, -14.14213562370292365 ) ) ;
#6459 = CARTESIAN_POINT ( 'NONE',  ( -213.1075012329537230, 66.26714140138673770, -9.698598906462034819 ) ) ;
#6460 = VECTOR ( 'NONE', #12832, 1000.000000000000000 ) ;
#6461 = CARTESIAN_POINT ( 'NONE',  ( 23.35901252181226795, 42.86175755505349372, -23.34306388117427389 ) ) ;
#6462 = CARTESIAN_POINT ( 'NONE',  ( 136.1360204305621551, 4.966164525587093870, -40.00000000000002132 ) ) ;
#6463 = CARTESIAN_POINT ( 'NONE',  ( -86.96347745069644475, -15.38646221621786125, -15.38646221621789856 ) ) ;
#6464 = CARTESIAN_POINT ( 'NONE',  ( -192.9588430854690273, 54.46834944101718889, 40.00000000000002132 ) ) ;
#6465 = CARTESIAN_POINT ( 'NONE',  ( -70.33906594828840753, -22.79894061172027264, 9.443630411840176819 ) ) ;
#6466 = CARTESIAN_POINT ( 'NONE',  ( 136.1360204305621551, -35.03383547441293899, 40.00000000000002132 ) ) ;
#6467 = ADVANCED_FACE ( 'NONE', ( #1334 ), #18946, .T. ) ;
#6468 = ORIENTED_EDGE ( 'NONE', *, *, #22744, .F. ) ;
#6469 = CARTESIAN_POINT ( 'NONE',  ( -199.9999999999999432, 30.70179486994649309, 44.88127304973814802 ) ) ;
#6470 = CARTESIAN_POINT ( 'NONE',  ( -135.8532207217289738, -34.75652343174615311, 21.81201906317767936 ) ) ;
#6471 = CARTESIAN_POINT ( 'NONE',  ( -16.87994666116329157, -12.91133298910015270, 42.52193590818846758 ) ) ;
#6472 = EDGE_CURVE ( 'NONE', #6051, #15971, #334, .T. ) ;
#6473 = CARTESIAN_POINT ( 'NONE',  ( -4.031723327955585745, 13.82865651623174763, -46.99313739789371880 ) ) ;
#6474 = CARTESIAN_POINT ( 'NONE',  ( 199.0255278052971732, -18.60593281614774952, 7.356242102916651149 ) ) ;
#6475 = CARTESIAN_POINT ( 'NONE',  ( -100.7734535825088358, -16.03295912088728770, 16.03295912088687913 ) ) ;
#6476 = CARTESIAN_POINT ( 'NONE',  ( 180.0000000000000000, -35.78896085774753288, -1.496915739050591872E-14 ) ) ;
#6477 = CARTESIAN_POINT ( 'NONE',  ( -28.75704569508346964, -35.61514925947763288, -18.59466133783093156 ) ) ;
#6478 = CARTESIAN_POINT ( 'NONE',  ( -198.9233928134166831, -24.80620717265403030, 44.84148042516471833 ) ) ;
#6479 = CARTESIAN_POINT ( 'NONE',  ( -86.96347745069643054, -40.00000000000026290, 21.75974354311608749 ) ) ;
#6480 = EDGE_CURVE ( 'NONE', #26122, #4257, #18309, .T. ) ;
#6481 = CARTESIAN_POINT ( 'NONE',  ( 19.06497207195981858, 10.03556273973516078, -66.60410523465806421 ) ) ;
#6482 = CARTESIAN_POINT ( 'NONE',  ( 0.2972598230769983307, -14.33493731733933352, 0.000000000000000000 ) ) ;
#6484 = CARTESIAN_POINT ( 'NONE',  ( 57.59792236341147031, 54.84617931850878136, 1.722363176415705910 ) ) ;
#6483 = CARTESIAN_POINT ( 'NONE',  ( -188.9266751785346230, 17.94050871568887118, -43.31221945728822931 ) ) ;
#6485 = CARTESIAN_POINT ( 'NONE',  ( -192.9588430854690273, 38.51493924976913519, 18.05360324515490333 ) ) ;
#6486 = CARTESIAN_POINT ( 'NONE',  ( 146.6084372240433709, -5.374981219216942385, -40.00000000000002132 ) ) ;
#6487 = CARTESIAN_POINT ( 'NONE',  ( -100.7734535825088500, 17.32597176626808988, 40.00000000000002132 ) ) ;
#6488 = CARTESIAN_POINT ( 'NONE',  ( -213.1075012329537230, -39.99999999999991473, -13.71589010951953647 ) ) ;
#6489 = CARTESIAN_POINT ( 'NONE',  ( 19.06497207195981858, 10.03556273973424062, 66.60410523465820631 ) ) ;
#6490 = CARTESIAN_POINT ( 'NONE',  ( 98.29820294267327085, -1.310413973320513126, 20.00000000000587264 ) ) ;
#6491 = CARTESIAN_POINT ( 'NONE',  ( 57.59792236341148453, -26.56190807104663421, -26.56190807104710672 ) ) ;
#6492 = CARTESIAN_POINT ( 'NONE',  ( -114.6382724355124623, 5.497872032160218581, 21.35157561685027972 ) ) ;
#6493 = VERTEX_POINT ( 'NONE', #18737 ) ;
#6494 = CARTESIAN_POINT ( 'NONE',  ( -100.7734535825088500, -44.31723036834903695, 12.25131212657476709 ) ) ;
#6495 = FACE_OUTER_BOUND ( 'NONE', #12453, .T. ) ;
#6496 = CARTESIAN_POINT ( 'NONE',  ( 184.8905102610680444, 14.79361573936366092, 41.77492675556006674 ) ) ;
#6497 = CARTESIAN_POINT ( 'NONE',  ( -0.6848998192559355713, -48.06291537635265598, -13.98809697771682004 ) ) ;
#6498 = EDGE_LOOP ( 'NONE', ( #12422, #4061, #18115, #8361, #2320 ) ) ;
#6499 = CARTESIAN_POINT ( 'NONE',  ( -726.9846540392142060, -52.49999999999992895, -52.49999999999999289 ) ) ;
#6500 = CARTESIAN_POINT ( 'NONE',  ( -575.0231298121466352, 75.00000000000000000, -30.00000000000202505 ) ) ;
#6501 = ORIENTED_EDGE ( 'NONE', *, *, #1020, .F. ) ;
#6502 = CARTESIAN_POINT ( 'NONE',  ( 199.9999999999999716, 15.97866926103663765, -10.28159943737610860 ) ) ;
#6503 = DIRECTION ( 'NONE',  ( -0.000000000000000000, -1.000000000000000000, -0.000000000000000000 ) ) ;
#6504 = CARTESIAN_POINT ( 'NONE',  ( -189.1288815661534386, -47.28031329127756521, -13.87115472123938709 ) ) ;
#6505 = CARTESIAN_POINT ( 'NONE',  ( -135.8532207217289738, -1.351063376314938213E-13, 30.84685318188645553 ) ) ;
#6506 = CARTESIAN_POINT ( 'NONE',  ( -280.0000000000000568, 19.99999999999996447, -40.00000000000002132 ) ) ;
#6507 = LINE ( 'NONE', #14617, #7093 ) ;
#6508 = CARTESIAN_POINT ( 'NONE',  ( 199.0257180514102799, -8.261434504147922908, 18.22213678534573589 ) ) ;
#6509 = CARTESIAN_POINT ( 'NONE',  ( 136.1360204305621266, 5.219216885335291329E-15, 4.966164525587064560 ) ) ;
#6510 = CARTESIAN_POINT ( 'NONE',  ( 192.4448373802101173, 40.00000000000012790, -20.00000000003928236 ) ) ;
#6511 = LINE ( 'NONE', #16891, #19344 ) ;
#6512 = CARTESIAN_POINT ( 'NONE',  ( -114.4364955367314707, 8.064892380844273845, -20.29001642038674902 ) ) ;
#6513 = CARTESIAN_POINT ( 'NONE',  ( -213.1075012329536946, -53.71589010951918652, -2.449293598294708485E-15 ) ) ;
#6514 = CARTESIAN_POINT ( 'NONE',  ( 170.2234770963711128, -10.92277846919202666, 10.92277846919193962 ) ) ;
#6515 = CARTESIAN_POINT ( 'NONE',  ( 155.1206158682454088, -11.51471166709232818, -27.79897307351034286 ) ) ;
#6516 = CARTESIAN_POINT ( 'NONE',  ( -105.2502192157478049, 17.39781795296955735, -12.58588914168777251 ) ) ;
#6517 = CARTESIAN_POINT ( 'NONE',  ( -162.0762913951020892, 4.094006889353306706E-13, -41.69427287682835015 ) ) ;
#6518 = CARTESIAN_POINT ( 'NONE',  ( 146.6084372240433709, -40.00000000000001421, 5.374981219216829587 ) ) ;
#6519 = CARTESIAN_POINT ( 'NONE',  ( -213.1075012329537230, 9.698598906450410340, 9.698598906450483170 ) ) ;
#6520 = FACE_BOUND ( 'NONE', #11424, .T. ) ;
#6521 = DIRECTION ( 'NONE',  ( 1.000000000000000000, 1.836970198721030427E-16, -0.000000000000000000 ) ) ;
#6522 = CARTESIAN_POINT ( 'NONE',  ( -162.0762913951020892, -29.48230308784785692, 29.48230308784751230 ) ) ;
#6523 = EDGE_LOOP ( 'NONE', ( #8127, #13309, #1015, #18412 ) ) ;
#6524 = FACE_OUTER_BOUND ( 'NONE', #21947, .T. ) ;
#6525 = CARTESIAN_POINT ( 'NONE',  ( 130.1167162091014404, 29.33455044752968277, -12.15076864148447200 ) ) ;
#6526 = CARTESIAN_POINT ( 'NONE',  ( 136.1360204305621266, 35.03383547441298163, -40.00000000000002132 ) ) ;
#6527 = ADVANCED_FACE ( 'NONE', ( #19839 ), #11022, .T. ) ;
#6528 = CARTESIAN_POINT ( 'NONE',  ( -105.4741150117383057, 8.366608964593771347, 19.60045294982731789 ) ) ;
#6529 = CARTESIAN_POINT ( 'NONE',  ( 199.9999999999999432, -14.14213562373115884, 14.14213562373085153 ) ) ;
#6530 = ORIENTED_EDGE ( 'NONE', *, *, #15786, .T. ) ;
#6531 = VERTEX_POINT ( 'NONE', #16873 ) ;
#6532 = CARTESIAN_POINT ( 'NONE',  ( -103.9474983245025186, 8.577167319634602549, -19.92928099173750311 ) ) ;
#6533 = CARTESIAN_POINT ( 'NONE',  ( -89.91498783736599876, 8.733585467966305416, -20.17141720489794210 ) ) ;
#6534 = CARTESIAN_POINT ( 'NONE',  ( 22.76403192593477343, 17.88468650128198689, 43.17745271018618070 ) ) ;
#6535 = EDGE_CURVE ( 'NONE', #7186, #4564, #11147, .T. ) ;
#6536 = ORIENTED_EDGE ( 'NONE', *, *, #24547, .T. ) ;
#6537 = ORIENTED_EDGE ( 'NONE', *, *, #16385, .F. ) ;
#6538 = CARTESIAN_POINT ( 'NONE',  ( -91.56559293963834989, -44.31723036834903695, 12.25131212657476709 ) ) ;
#6539 = CARTESIAN_POINT ( 'NONE',  ( 199.0258841556672564, -17.79651494919816912, 9.142457329253240061 ) ) ;
#6540 = CARTESIAN_POINT ( 'NONE',  ( -114.7248266913260295, 3.464717969334141667, 21.81737765724340861 ) ) ;
#6541 = EDGE_CURVE ( 'NONE', #9825, #18337, #18740, .T. ) ;
#6542 = CARTESIAN_POINT ( 'NONE',  ( -105.3755690713226727, -15.38646221621786481, -15.38646221621789856 ) ) ;
#6543 = CARTESIAN_POINT ( 'NONE',  ( -105.2285682121444808, 21.34137888092660518, 2.786758726753435500 ) ) ;
#6544 = CARTESIAN_POINT ( 'NONE',  ( -87.13361725327072804, 21.49321519333427233, -1.448021113139547951E-30 ) ) ;
#6545 = CARTESIAN_POINT ( 'NONE',  ( -109.1264249741455217, 33.12752917269229158, -13.72187187124002783 ) ) ;
#6546 = CARTESIAN_POINT ( 'NONE',  ( -259.2033419157646676, 2.741182173978444749E-13, -30.48217210827739621 ) ) ;
#6547 = CARTESIAN_POINT ( 'NONE',  ( -105.3755690713226727, -2.472783935621397949E-13, 21.75974354311649961 ) ) ;
#6548 = DIRECTION ( 'NONE',  ( 0.000000000000000000, -1.000000000000000000, 0.000000000000000000 ) ) ;
#6549 = DIRECTION ( 'NONE',  ( 1.000000000000000000, 0.000000000000000000, 0.000000000000000000 ) ) ;
#6550 = CARTESIAN_POINT ( 'NONE',  ( 199.0056040927672711, 16.99126215759308778, -10.54120702991739122 ) ) ;
#6551 = CARTESIAN_POINT ( 'NONE',  ( -189.1288337602708509, 13.87115233298066030, 47.28029723722608679 ) ) ;
#6552 = CARTESIAN_POINT ( 'NONE',  ( 151.7948205124836250, 23.49921654116328540, 23.49921654116366554 ) ) ;
#6553 = CARTESIAN_POINT ( 'NONE',  ( 160.9163046357249129, -205.7889608577475542, -61.61140153332245006 ) ) ;
#6554 = CARTESIAN_POINT ( 'NONE',  ( -208.1127848780264742, -10.60833733268345469, 67.17687982760682530 ) ) ;
#6555 = CARTESIAN_POINT ( 'NONE',  ( -77.90255099907052738, 8.064892378688679031, 20.29001641119211641 ) ) ;
#6556 = CARTESIAN_POINT ( 'NONE',  ( 130.8568914410475088, 52.36146031193427319, -4.207082182989173802 ) ) ;
#6557 = DIRECTION ( 'NONE',  ( -0.7071067811865501263, 0.7071067811865449082, 8.659560562354902043E-17 ) ) ;
#6558 = CARTESIAN_POINT ( 'NONE',  ( -100.7734535825088500, 22.67402823373189591, -0.000000000000000000 ) ) ;
#6559 = CARTESIAN_POINT ( 'NONE',  ( 0.2972598230769886718, 38.42060263243643448, 18.14793986248763957 ) ) ;
#6560 = CARTESIAN_POINT ( 'NONE',  ( 19.06497207195981503, -14.19242893257840166, 0.000000000000000000 ) ) ;
#6561 = CARTESIAN_POINT ( 'NONE',  ( -88.39148973765139772, 20.15708830332379975, -8.027153355909627308 ) ) ;
#6562 = CARTESIAN_POINT ( 'NONE',  ( -30.26275506840323359, -39.99999999999959499, -41.69427246844670520 ) ) ;
#6563 = CARTESIAN_POINT ( 'NONE',  ( 199.0119122942934098, -7.649365998490048391, -18.47719605185541170 ) ) ;
#6564 = LINE ( 'NONE', #14682, #13263 ) ;
#6565 = ORIENTED_EDGE ( 'NONE', *, *, #16134, .F. ) ;
#6566 = ORIENTED_EDGE ( 'NONE', *, *, #543, .F. ) ;
#6567 = CARTESIAN_POINT ( 'NONE',  ( 136.1360204305621551, 4.966164525587085876, 40.00000000000002132 ) ) ;
#6568 = ADVANCED_FACE ( 'NONE', ( #23391 ), #9703, .T. ) ;
#6569 = PLANE ( 'NONE',  #21469 ) ;
#6570 = CARTESIAN_POINT ( 'NONE',  ( -213.1075012329537230, 37.98287015391280619, -37.98287015391192512 ) ) ;
#6571 = CARTESIAN_POINT ( 'NONE',  ( -114.7248266913117760, -21.81737765723738320, 3.464717969335482373 ) ) ;
#6572 = CARTESIAN_POINT ( 'NONE',  ( -626.9846540392097722, 90.00000000000000000, 54.99999999999995737 ) ) ;
#6573 = PRODUCT_DEFINITION_SHAPE ( 'NONE', 'NONE',  #26367 ) ;
#6574 = DIRECTION ( 'NONE',  ( 0.000000000000000000, 0.000000000000000000, -1.000000000000000000 ) ) ;
#6575 = CARTESIAN_POINT ( 'NONE',  ( 199.9999999999999716, -3.557237102606629620, -18.66704445460036865 ) ) ;
#6576 = B_SPLINE_CURVE_WITH_KNOTS ( 'NONE', 3,
 ( #23225, #5130, #9107, #6714, #2878, #14828 ),
 .UNSPECIFIED., .F., .F.,
 ( 4, 2, 4 ),
 ( 0.000000000000000000, 0.004167810130244177513, 0.008335620260488355027 ),
 .UNSPECIFIED. ) ;
#6577 = CARTESIAN_POINT ( 'NONE',  ( 200.0000000000000284, 4.312859453180151625, -18.51524271434543323 ) ) ;
#6578 = CARTESIAN_POINT ( 'NONE',  ( -238.4067589809705794, -27.60227080167029001, -28.96627169325357798 ) ) ;
#6579 = CARTESIAN_POINT ( 'NONE',  ( -30.26275506840324070, -1.198031551616016266, -1.198031551616031587 ) ) ;
#6580 = CARTESIAN_POINT ( 'NONE',  ( 170.0000000000000284, -22.62041470344884431, 9.369682556672202622 ) ) ;
#6581 = CARTESIAN_POINT ( 'NONE',  ( -86.96347745069645896, 39.99999999999977973, 21.75974354311691883 ) ) ;
#6582 = CARTESIAN_POINT ( 'NONE',  ( -89.92902785008683963, -8.088236460650220394, 20.44110050034126758 ) ) ;
#6583 = CARTESIAN_POINT ( 'NONE',  ( 22.82385994800817386, 13.83113328680598464, 47.01156385802197235 ) ) ;
#6584 = CARTESIAN_POINT ( 'NONE',  ( 199.9999999999999432, -14.14213562373115884, 14.14213562373085153 ) ) ;
#6585 = CARTESIAN_POINT ( 'NONE',  ( 199.9999999999999432, -14.14213562373093680, 14.14213562373082311 ) ) ;
#6587 = CARTESIAN_POINT ( 'NONE',  ( -105.3755690713226727, -8.549198663894545631E-14, 18.24025645688352881 ) ) ;
#6586 = CARTESIAN_POINT ( 'NONE',  ( -91.56559293963834989, -44.31723036834885932, -12.25131212657538171 ) ) ;
#6588 = CARTESIAN_POINT ( 'NONE',  ( 22.78333232259046071, 43.17211919388257257, -17.88247728649356461 ) ) ;
#6589 = CARTESIAN_POINT ( 'NONE',  ( -213.1075012329537230, 13.71589010951907994, 0.000000000000000000 ) ) ;
#6590 = CARTESIAN_POINT ( 'NONE',  ( 0.2972598230769990524, -18.14793986248724522, 38.42060263243662632 ) ) ;
#6591 = CARTESIAN_POINT ( 'NONE',  ( -198.0356074513804572, 15.37879056873066830, 40.00000000000002132 ) ) ;
#6592 = CARTESIAN_POINT ( 'NONE',  ( -4.439300432583311640, -42.88738538954532942, 23.37136716947943071 ) ) ;
#6593 = AXIS2_PLACEMENT_3D ( 'NONE', #5918, #21748, #15485 ) ;
#6594 = CIRCLE ( 'NONE', #21470, 5.000000000000011546 ) ;
#6595 = CARTESIAN_POINT ( 'NONE',  ( 136.1360204305621551, 4.966164525587085876, 40.00000000000002132 ) ) ;
#6596 = ORIENTED_EDGE ( 'NONE', *, *, #19245, .F. ) ;
#6597 = CARTESIAN_POINT ( 'NONE',  ( -199.9999999999999432, 35.57044988732131685, 42.45148791631880414 ) ) ;
#6598 = CARTESIAN_POINT ( 'NONE',  ( -91.56559293963834989, -44.31723036834903695, 12.25131212657476709 ) ) ;
#6599 = CARTESIAN_POINT ( 'NONE',  ( -4.421177063218048708, -23.37490463203918267, 42.89273859401259870 ) ) ;
#6600 = CARTESIAN_POINT ( 'NONE',  ( -4.076660308449207903, 23.44206949513791116, -42.99426297939334773 ) ) ;
#6601 = CARTESIAN_POINT ( 'NONE',  ( 199.0214947048457077, -19.49260886005912141, -4.535603965114707314 ) ) ;
#6602 = CARTESIAN_POINT ( 'NONE',  ( -213.1075012329537230, 37.98287015391211696, 18.58567234101190735 ) ) ;
#6603 = CARTESIAN_POINT ( 'NONE',  ( -82.24465949241034934, -20.03613703209230579, 2.525178489117738678 ) ) ;
#6604 = DIRECTION ( 'NONE',  ( 0.000000000000000000, 1.000000000000000000, 0.000000000000000000 ) ) ;
#6605 = CARTESIAN_POINT ( 'NONE',  ( -192.9370379451729036, -14.03127537977607453, 48.35015161801144501 ) ) ;
#6606 = CARTESIAN_POINT ( 'NONE',  ( 19.06497207195981147, 1.521599808664285085E-13, -14.19242893257840521 ) ) ;
#6607 = CARTESIAN_POINT ( 'NONE',  ( 146.6084372240433709, -52.76785682606510619, -3.800685668859292043 ) ) ;
#6608 = CARTESIAN_POINT ( 'NONE',  ( -105.3755690713226585, 43.67073346367988051, -12.89780903124366418 ) ) ;
#6609 = CIRCLE ( 'NONE', #16820, 69.99999999999998579 ) ;
#6610 = AXIS2_PLACEMENT_3D ( 'NONE', #19276, #5557, #17148 ) ;
#6612 = CARTESIAN_POINT ( 'NONE',  ( -238.4067589809705794, 28.96627169325354956, -28.96627169325289231 ) ) ;
#6611 = CARTESIAN_POINT ( 'NONE',  ( 146.6084372240433993, 24.48358557860307272, 24.48358557860347418 ) ) ;
#6613 = CARTESIAN_POINT ( 'NONE',  ( -105.3755690713226585, 12.89780903124349720, 43.67073346367994446 ) ) ;
#6614 = EDGE_CURVE ( 'NONE', #15079, #1078, #23514, .T. ) ;
#6615 = CARTESIAN_POINT ( 'NONE',  ( 130.8568914410475088, -5.949712681206664300, -40.00000000000002132 ) ) ;
#6616 = CARTESIAN_POINT ( 'NONE',  ( 130.8568914410475088, 5.949712681206712261, 40.00000000000002132 ) ) ;
#6617 = CARTESIAN_POINT ( 'NONE',  ( 91.82158438592159655, -40.00000000000017764, 17.20528682183258340 ) ) ;
#6618 = CARTESIAN_POINT ( 'NONE',  ( -213.1075012329537230, 9.698598906450410340, 9.698598906450483170 ) ) ;
#6619 = CARTESIAN_POINT ( 'NONE',  ( -105.4741150117378936, 19.60045294982725750, -8.366608964594151487 ) ) ;
#6620 = CARTESIAN_POINT ( 'NONE',  ( -105.3755690713226727, -12.89780903124395550, -12.89780903124416511 ) ) ;
#6621 = CARTESIAN_POINT ( 'NONE',  ( -114.7756899093956946, 1.373957298918453418, 22.09342955265359620 ) ) ;
#6622 = EDGE_LOOP ( 'NONE', ( #10364, #7395, #22213, #26292, #9192, #24198, #17046, #1460, #10674 ) ) ;
#6623 = AXIS2_PLACEMENT_3D ( 'NONE', #16430, #10715, #472 ) ;
#6624 = CARTESIAN_POINT ( 'NONE',  ( 0.2972598230769959993, 38.42060263243659080, 38.42060263243672580 ) ) ;
#6625 = CARTESIAN_POINT ( 'NONE',  ( -96.94449363884535842, 8.590991631016400731, 20.74048850978408964 ) ) ;
#6626 = AXIS2_PLACEMENT_3D ( 'NONE', #14781, #13060, #22649 ) ;
#6627 = CARTESIAN_POINT ( 'NONE',  ( 19.06497207195982568, -38.31983398719646061, 38.31983398719606271 ) ) ;
#6628 = CARTESIAN_POINT ( 'NONE',  ( 20.16956056503547856, -43.71646652951510958, -23.97604322319288528 ) ) ;
#6629 = EDGE_CURVE ( 'NONE', #19209, #8490, #7252, .T. ) ;
#6630 = EDGE_LOOP ( 'NONE', ( #25495, #11988 ) ) ;
#6631 = DIRECTION ( 'NONE',  ( -1.000000000000000000, 1.836970198721030181E-16, 0.000000000000000000 ) ) ;
#6632 = CARTESIAN_POINT ( 'NONE',  ( -200.0000000000000000, -35.57044988732172186, 42.45148791632026075 ) ) ;
#6633 = EDGE_CURVE ( 'NONE', #25845, #3723, #11178, .T. ) ;
#6634 = CARTESIAN_POINT ( 'NONE',  ( 200.0000000000000284, 8.678546691382686973, -16.90316441639222944 ) ) ;
#6635 = DIRECTION ( 'NONE',  ( -1.000000000000000000, -1.836970198721030181E-16, 0.000000000000000000 ) ) ;
#6636 = CARTESIAN_POINT ( 'NONE',  ( 4.995406935893288214, 55.24977328853207581, 40.00000000000002132 ) ) ;
#6637 = CARTESIAN_POINT ( 'NONE',  ( -56.48582580120559982, -34.75652343174584047, -21.81201906317815187 ) ) ;
#6638 = CARTESIAN_POINT ( 'NONE',  ( 199.0112867096082141, 18.93484222638594616, 6.440921653838688421 ) ) ;
#6639 = AXIS2_PLACEMENT_3D ( 'NONE', #23295, #5195, #5071 ) ;
#6640 = CARTESIAN_POINT ( 'NONE',  ( -30.26275506840324070, -29.48230279907817675, 27.08623969584564151 ) ) ;
#6641 = CARTESIAN_POINT ( 'NONE',  ( -238.4067589809705794, 39.99999999999983658, 40.96449428006354765 ) ) ;
#6642 = CARTESIAN_POINT ( 'NONE',  ( 146.6084372240433709, 40.00000000000017053, -34.62501878078291639 ) ) ;
#6643 = CARTESIAN_POINT ( 'NONE',  ( -3.903133374353591645, 47.03983734332609146, -13.83543723425202465 ) ) ;
#6644 = CARTESIAN_POINT ( 'NONE',  ( -213.1075012329537230, -13.71589010951915810, 0.000000000000000000 ) ) ;
#6645 = CARTESIAN_POINT ( 'NONE',  ( -597.0972138806185967, 39.91563328523288590, 2.647040059433892978 ) ) ;
#6646 = CARTESIAN_POINT ( 'NONE',  ( -259.2033419157646676, -30.48217210827744239, -2.449293598294708485E-15 ) ) ;
#6647 = CARTESIAN_POINT ( 'NONE',  ( 4.995406935893301537, -10.78321810390187530, 67.35176059882529387 ) ) ;
#6648 = CARTESIAN_POINT ( 'NONE',  ( 133.2080217031555662, -12.38638889282717415, -29.90338805389119869 ) ) ;
#6649 = CARTESIAN_POINT ( 'NONE',  ( -114.7827252410365020, 16.13252424104745941, -15.16659028662510877 ) ) ;
#6650 = CARTESIAN_POINT ( 'NONE',  ( -198.0356074513804572, 40.00000000000056843, -55.37879056871282302 ) ) ;
#6651 = CARTESIAN_POINT ( 'NONE',  ( -105.3755690713226585, 39.99999999999993605, 18.24025645688366737 ) ) ;
#6652 = CARTESIAN_POINT ( 'NONE',  ( 57.59792236341147031, -1.722363176415032004, -1.722363176415048880 ) ) ;
#6653 = FACE_BOUND ( 'NONE', #16421, .T. ) ;
#6654 = CYLINDRICAL_SURFACE ( 'NONE', #17239, 29.99999999999999645 ) ;
#6655 = CARTESIAN_POINT ( 'NONE',  ( 4.995406935893305977, -39.06748935135212264, 39.06748935135171763 ) ) ;
#6656 = ORIENTED_EDGE ( 'NONE', *, *, #11169, .F. ) ;
#6658 = CARTESIAN_POINT ( 'NONE',  ( -62.79433447044806371, 25.93934121804208104, -9.335111860717981713 ) ) ;
#6657 = CARTESIAN_POINT ( 'NONE',  ( 130.8568914410475372, 24.07718906447210472, 24.07718906447249907 ) ) ;
#6659 = DIRECTION ( 'NONE',  ( -1.000000000000000000, -0.000000000000000000, -0.000000000000000000 ) ) ;
#6660 = CARTESIAN_POINT ( 'NONE',  ( -56.48582580120558561, -30.84685318188645553, -40.00000000000002132 ) ) ;
#6661 = DIRECTION ( 'NONE',  ( 0.000000000000000000, 0.000000000000000000, 1.000000000000000000 ) ) ;
#6662 = DIRECTION ( 'NONE',  ( 0.000000000000000000, -1.000000000000000000, 0.000000000000000000 ) ) ;
#6663 = ORIENTED_EDGE ( 'NONE', *, *, #13817, .F. ) ;
#6664 = ORIENTED_EDGE ( 'NONE', *, *, #7740, .T. ) ;
#6665 = CARTESIAN_POINT ( 'NONE',  ( 48.46159092537990887, -11.89574569450918062, 37.63079858261905741 ) ) ;
#6666 = CARTESIAN_POINT ( 'NONE',  ( -100.0957100001467381, 8.517115559260357571, -20.56213589538073094 ) ) ;
#6667 = CARTESIAN_POINT ( 'NONE',  ( 12.96694272570842799, 14.15914421029697579, 49.19577900137000626 ) ) ;
#6668 = ORIENTED_EDGE ( 'NONE', *, *, #5390, .T. ) ;
#6669 = AXIS2_PLACEMENT_3D ( 'NONE', #15860, #1652, #14147 ) ;
#6670 = ORIENTED_EDGE ( 'NONE', *, *, #14441, .F. ) ;
#6671 = CARTESIAN_POINT ( 'NONE',  ( -91.56559293963834989, -16.03295912088716335, 40.53558337403673306 ) ) ;
#6672 = CARTESIAN_POINT ( 'NONE',  ( 199.0193324171001450, -17.94164708558885124, -8.847044913458905313 ) ) ;
#6673 = CARTESIAN_POINT ( 'NONE',  ( -105.4741150117371262, -7.943527260734682294, 19.77569912955828357 ) ) ;
#6674 = CARTESIAN_POINT ( 'NONE',  ( 170.2234770963711128, -45.64576402573183600, 10.92277846919191653 ) ) ;
#6675 = PLANE ( 'NONE',  #14841 ) ;
#6676 = CARTESIAN_POINT ( 'NONE',  ( -86.96347745069645896, 39.99999999999994316, 18.24025645688366737 ) ) ;
#6677 = DIRECTION ( 'NONE',  ( 1.303213150798907793E-16, -1.000000000000000000, 0.000000000000000000 ) ) ;
#6678 = CARTESIAN_POINT ( 'NONE',  ( -575.0231298121466352, 75.00000000000000000, -25.00000000000201794 ) ) ;
#6679 = CARTESIAN_POINT ( 'NONE',  ( -100.7734535825088358, 1.654174317907124744E-13, -17.32597176626811120 ) ) ;
#6680 = CARTESIAN_POINT ( 'NONE',  ( -30.26275506840325136, 40.00000000000003553, -1.694272468445841007 ) ) ;
#6681 = CARTESIAN_POINT ( 'NONE',  ( -655.3024676147620085, 38.75379567404313974, 9.955511827537780079 ) ) ;
#6682 = LINE ( 'NONE', #18932, #9406 ) ;
#6683 = CARTESIAN_POINT ( 'NONE',  ( 199.0127395736742244, 17.77917978336349236, 9.157720830221606434 ) ) ;
#6684 = CARTESIAN_POINT ( 'NONE',  ( -187.3036811847924810, 13.75782060303311738, 46.64553187116074895 ) ) ;
#6685 = B_SPLINE_CURVE_WITH_KNOTS ( 'NONE', 3,
 ( #7940, #5958, #20462, #14067, #22464, #775 ),
 .UNSPECIFIED., .F., .F.,
 ( 4, 2, 4 ),
 ( 0.000000000000000000, 0.004089982295592885925, 0.008179964591185771849 ),
 .UNSPECIFIED. ) ;
#6686 = CARTESIAN_POINT ( 'NONE',  ( -208.1127848780265026, -10.60833733269537227, -10.60833733269551793 ) ) ;
#6687 = CARTESIAN_POINT ( 'NONE',  ( -105.4741150117383057, 8.366608964593771347, 19.60045294982731789 ) ) ;
#6688 = CARTESIAN_POINT ( 'NONE',  ( -259.2033419157646676, 35.01439189186528722, 21.55415060305857011 ) ) ;
#6689 = CARTESIAN_POINT ( 'NONE',  ( -77.56366795221718746, 1.395416561020218715, 22.09173432935380887 ) ) ;
#6690 = CARTESIAN_POINT ( 'NONE',  ( -135.8532207217289738, 6.472252184284583265, -50.09629031063960980 ) ) ;
#6691 = CARTESIAN_POINT ( 'NONE',  ( -626.9846540392142060, 95.00000000000000000, 0.000000000000000000 ) ) ;
#6692 = CARTESIAN_POINT ( 'NONE',  ( 98.29820294273291381, -18.47759065023123526, -7.653668647304108674 ) ) ;
#6693 = CARTESIAN_POINT ( 'NONE',  ( 4.995406935893283773, 39.06748935135171052, 17.50105314357239195 ) ) ;
#6694 = B_SPLINE_CURVE_WITH_KNOTS ( 'NONE', 3,
 ( #13553, #25683, #5578, #7431, #15545, #15422, #11182, #11306, #25813, #13430, #7064, #21806 ),
 .UNSPECIFIED., .F., .F.,
 ( 4, 2, 2, 2, 2, 4 ),
 ( 1.158526472511095878E-15, 0.004680202113614856732, 0.009360404227228554669, 0.01170050528403540277, 0.01404060634084225261, 0.01872080845445590891 ),
 .UNSPECIFIED. ) ;
#6695 = CARTESIAN_POINT ( 'NONE',  ( -56.48582580120559982, 9.153146818113574668, 40.00000000000002132 ) ) ;
#6696 = CARTESIAN_POINT ( 'NONE',  ( -592.1138474530150688, 44.89957181662549601, -3.064942242840709152 ) ) ;
#6697 = EDGE_LOOP ( 'NONE', ( #2378, #25082, #21556, #6663 ) ) ;
#6698 = CARTESIAN_POINT ( 'NONE',  ( -105.3755690713226585, -40.00000000000027711, 21.75974354311608749 ) ) ;
#6699 = CARTESIAN_POINT ( 'NONE',  ( 199.0059792703121389, 8.401033297471425243, -18.14527037458064385 ) ) ;
#6700 = DIRECTION ( 'NONE',  ( -1.357111460130037815E-16, 0.7387770694782699321, -0.6739498806388346530 ) ) ;
#6701 = ORIENTED_EDGE ( 'NONE', *, *, #14853, .F. ) ;
#6702 = ORIENTED_EDGE ( 'NONE', *, *, #25837, .F. ) ;
#6703 = CARTESIAN_POINT ( 'NONE',  ( -135.8532207217289738, 30.84685318188643066, 2.449293598294708485E-15 ) ) ;
#6704 = DIRECTION ( 'NONE',  ( -1.000000000000000000, 0.000000000000000000, 0.000000000000000000 ) ) ;
#6705 = CARTESIAN_POINT ( 'NONE',  ( -105.4741150117398405, -19.77569912953930142, 7.943527260776874321 ) ) ;
#6706 = EDGE_CURVE ( 'NONE', #961, #13948, #1603, .T. ) ;
#6707 = CARTESIAN_POINT ( 'NONE',  ( -109.1264249741452090, 13.72187187126506025, -33.12752917268247188 ) ) ;
#6708 = CARTESIAN_POINT ( 'NONE',  ( 0.2972598230770030492, -40.00000000000007816, 14.33493731733919496 ) ) ;
#6709 = CARTESIAN_POINT ( 'NONE',  ( 199.9999999999998010, 5.803429233430792422, -18.09525674440013177 ) ) ;
#6710 = EDGE_CURVE ( 'NONE', #16682, #19908, #14923, .T. ) ;
#6711 = CARTESIAN_POINT ( 'NONE',  ( -105.2054292635176864, 1.371497798096047660, -21.49321519473980757 ) ) ;
#6712 = CARTESIAN_POINT ( 'NONE',  ( 170.2234770963711128, -45.64576402573167258, -10.92277846919254891 ) ) ;
#6713 = CARTESIAN_POINT ( 'NONE',  ( -238.4067589809705794, -0.6820004457913585449, -0.6820004457913265705 ) ) ;
#6714 = CARTESIAN_POINT ( 'NONE',  ( -77.70105001122996669, -18.98740555847804856, -11.20619870950665309 ) ) ;
#6715 = CARTESIAN_POINT ( 'NONE',  ( 0.2972598230769883387, 40.00000000000017053, -14.33493731733891607 ) ) ;
#6716 = CARTESIAN_POINT ( 'NONE',  ( 57.59792236341147031, 1.722363176415040886, 1.722363176415060426 ) ) ;
#6717 = CARTESIAN_POINT ( 'NONE',  ( -3.903133374380808984, 13.83543723414519810, 47.03983734341694856 ) ) ;
#6718 = CARTESIAN_POINT ( 'NONE',  ( 192.4448373802100889, -14.14213562375896061, 14.14213562375865330 ) ) ;
#6719 = ADVANCED_FACE ( 'NONE', ( #13680 ), #11400, .T. ) ;
#6720 = ADVANCED_FACE ( 'NONE', ( #11547 ), #25548, .T. ) ;
#6721 = CARTESIAN_POINT ( 'NONE',  ( 136.1360204305621266, -3.511608612530682905, 3.511608612530666917 ) ) ;
#6722 = CARTESIAN_POINT ( 'NONE',  ( 199.0132120035298442, 17.35012746940816797, 9.967304425461927408 ) ) ;
#6724 = CARTESIAN_POINT ( 'NONE',  ( -30.26275506840324070, -1.147469862568086380E-14, 1.694272468446259783 ) ) ;
#6723 = CARTESIAN_POINT ( 'NONE',  ( -192.9588430854689989, 10.23066800230756712, -10.23066800230735396 ) ) ;
#6725 = CARTESIAN_POINT ( 'NONE',  ( 67.79414719560435287, 30.31905270963685339, -10.30785037341317611 ) ) ;
#6726 = CARTESIAN_POINT ( 'NONE',  ( 163.1118516004056573, -27.26290988616869626, -40.00000000000002132 ) ) ;
#6727 = CARTESIAN_POINT ( 'NONE',  ( 19.06497207195980792, 10.03556273973433299, 10.03556273973436319 ) ) ;
#6728 = CARTESIAN_POINT ( 'NONE',  ( 151.7948205124836250, -33.23291073765550863, 0.000000000000000000 ) ) ;
#6729 = ORIENTED_EDGE ( 'NONE', *, *, #18576, .F. ) ;
#6730 =( BOUNDED_SURFACE ( )  B_SPLINE_SURFACE ( 3, 3, ( 
 ( #9123, #1154, #17235, #13125, #15487, #21620, #9507, #9258, #19364, #11247, #23371, #3144, #21246, #9379, #7376, #11491, #17364, #5267, #25501, #11002, #7248, #5396, #15370, #11128, #19241, #19490, #2894, #1406, #1022, #12995 ),
 ( #15110, #13370, #25376, #895, #23245, #5146, #15239, #21496, #13498, #3395, #19621, #19112, #13252, #21375, #17612, #25756, #7504, #23116, #4888, #21117, #25242, #9005, #17110, #14028, #12170, #9774, #22024, #1666, #19883, #5783 ),
 ( #3937, #64, #1802, #4067, #9905, #3795, #26295, #26025, #1933, #22157, #20152, #22291, #19746, #23738, #18146, #18011, #13890, #17874, #26157, #16019, #7762, #7900, #11898, #21879, #20289, #24002, #24144, #15874, #2068, #11625 ),
 ( #15741, #10175, #20021, #5920, #3657, #12033, #18279, #10039, #15614, #8035, #16154, #5519, #24285, #6055, #14159, #13623, #21750, #3524, #1536, #9641, #17744, #25885, #7628, #23871, #5646, #13752, #11764, #15055, #12939, #24415 ),
 ( #20929, #21054, #2708, #24925, #968, #7073, #21317, #2839, #4833, #23061, #8812, #14922, #6676, #13072, #2960, #23313, #10949, #17054, #19055, #22428, #837, #19185, #8946, #16789, #4700, #23184, #14293, #13194, #14791, #6180 ),
 ( #4964, #25188, #15187, #6937, #574, #19305, #9072, #8173, #16288, #21188, #22921, #11070, #2565, #10813, #12806, #4203, #8679, #18924, #17179, #16923, #12667, #25314, #5090, #708, #3090, #11190, #20794, #10682, #18793, #25057 ),
 ( #6808, #5331, #17554, #21689, #15556, #1346, #13440, #21954, #7569, #19433, #9448, #9322, #15682, #7192, #5715, #25692, #11316, #11562, #3728, #13695, #19556, #21818, #9574, #1090, #7442, #23681, #3335, #5460, #9198, #19682 ) ),
 .UNSPECIFIED., .T., .F., .T. ) 
 B_SPLINE_SURFACE_WITH_KNOTS ( ( 4, 3, 4 ),
 ( 4, 2, 2, 2, 2, 2, 2, 2, 2, 2, 2, 2, 2, 2, 4 ),
 ( 0.000000000000000000, 0.5000000000000000000, 1.000000000000000000 ),
 ( 0.000000000000000000, 0.1357259735107005372, 0.1651108541090157700, 0.1944957347073310028, 0.3598804999793158710, 0.3867117631979620773, 0.4135430264166082281, 0.5789277916885930964, 0.6062785021374117456, 0.6336292125862302838, 0.8508620842112317728, 0.8814014469398914198, 0.9119408096685510667, 0.9559704048342755334, 1.000000000000000000 ),
 .UNSPECIFIED. ) 
 GEOMETRIC_REPRESENTATION_ITEM ( )  RATIONAL_B_SPLINE_SURFACE ( (
 ( 1.000000000000000000, 1.000000000000000000, 1.000000000000000000, 1.000000000000000000, 1.000000000000000000, 1.000000000000000000, 1.000000000000000000, 1.000000000000000000, 1.000000000000000000, 1.000000000000000000, 1.000000000000000000, 1.000000000000000000, 1.000000000000000000, 1.000000000000000000, 1.000000000000000000, 1.000000000000000000, 1.000000000000000000, 1.000000000000000000, 1.000000000000000000, 1.000000000000000000, 1.000000000000000000, 1.000000000000000000, 1.000000000000000000, 1.000000000000000000, 1.000000000000000000, 1.000000000000000000, 1.000000000000000000, 1.000000000000000000, 1.000000000000000000, 1.000000000000000000),
 ( 0.3333333333333333703, 0.3333333333333333703, 0.3333333333333333703, 0.3333333333333333703, 0.3333333333333333703, 0.3333333333333333703, 0.3333333333333333703, 0.3333333333333333703, 0.3333333333333333703, 0.3333333333333333703, 0.3333333333333333703, 0.3333333333333333703, 0.3333333333333333703, 0.3333333333333333703, 0.3333333333333333703, 0.3333333333333333703, 0.3333333333333333703, 0.3333333333333333703, 0.3333333333333333703, 0.3333333333333333703, 0.3333333333333333703, 0.3333333333333333703, 0.3333333333333333703, 0.3333333333333333703, 0.3333333333333333703, 0.3333333333333333703, 0.3333333333333333703, 0.3333333333333333703, 0.3333333333333333703, 0.3333333333333333703),
 ( 0.3333333333333333703, 0.3333333333333333703, 0.3333333333333333703, 0.3333333333333333703, 0.3333333333333333703, 0.3333333333333333703, 0.3333333333333333703, 0.3333333333333333703, 0.3333333333333333703, 0.3333333333333333703, 0.3333333333333333703, 0.3333333333333333703, 0.3333333333333333703, 0.3333333333333333703, 0.3333333333333333703, 0.3333333333333333703, 0.3333333333333333703, 0.3333333333333333703, 0.3333333333333333703, 0.3333333333333333703, 0.3333333333333333703, 0.3333333333333333703, 0.3333333333333333703, 0.3333333333333333703, 0.3333333333333333703, 0.3333333333333333703, 0.3333333333333333703, 0.3333333333333333703, 0.3333333333333333703, 0.3333333333333333703),
 ( 1.000000000000000000, 1.000000000000000000, 1.000000000000000000, 1.000000000000000000, 1.000000000000000000, 1.000000000000000000, 1.000000000000000000, 1.000000000000000000, 1.000000000000000000, 1.000000000000000000, 1.000000000000000000, 1.000000000000000000, 1.000000000000000000, 1.000000000000000000, 1.000000000000000000, 1.000000000000000000, 1.000000000000000000, 1.000000000000000000, 1.000000000000000000, 1.000000000000000000, 1.000000000000000000, 1.000000000000000000, 1.000000000000000000, 1.000000000000000000, 1.000000000000000000, 1.000000000000000000, 1.000000000000000000, 1.000000000000000000, 1.000000000000000000, 1.000000000000000000),
 ( 0.3333333333333333703, 0.3333333333333333703, 0.3333333333333333703, 0.3333333333333333703, 0.3333333333333333703, 0.3333333333333333703, 0.3333333333333333703, 0.3333333333333333703, 0.3333333333333333703, 0.3333333333333333703, 0.3333333333333333703, 0.3333333333333333703, 0.3333333333333333703, 0.3333333333333333703, 0.3333333333333333703, 0.3333333333333333703, 0.3333333333333333703, 0.3333333333333333703, 0.3333333333333333703, 0.3333333333333333703, 0.3333333333333333703, 0.3333333333333333703, 0.3333333333333333703, 0.3333333333333333703, 0.3333333333333333703, 0.3333333333333333703, 0.3333333333333333703, 0.3333333333333333703, 0.3333333333333333703, 0.3333333333333333703),
 ( 0.3333333333333333703, 0.3333333333333333703, 0.3333333333333333703, 0.3333333333333333703, 0.3333333333333333703, 0.3333333333333333703, 0.3333333333333333703, 0.3333333333333333703, 0.3333333333333333703, 0.3333333333333333703, 0.3333333333333333703, 0.3333333333333333703, 0.3333333333333333703, 0.3333333333333333703, 0.3333333333333333703, 0.3333333333333333703, 0.3333333333333333703, 0.3333333333333333703, 0.3333333333333333703, 0.3333333333333333703, 0.3333333333333333703, 0.3333333333333333703, 0.3333333333333333703, 0.3333333333333333703, 0.3333333333333333703, 0.3333333333333333703, 0.3333333333333333703, 0.3333333333333333703, 0.3333333333333333703, 0.3333333333333333703),
 ( 1.000000000000000000, 1.000000000000000000, 1.000000000000000000, 1.000000000000000000, 1.000000000000000000, 1.000000000000000000, 1.000000000000000000, 1.000000000000000000, 1.000000000000000000, 1.000000000000000000, 1.000000000000000000, 1.000000000000000000, 1.000000000000000000, 1.000000000000000000, 1.000000000000000000, 1.000000000000000000, 1.000000000000000000, 1.000000000000000000, 1.000000000000000000, 1.000000000000000000, 1.000000000000000000, 1.000000000000000000, 1.000000000000000000, 1.000000000000000000, 1.000000000000000000, 1.000000000000000000, 1.000000000000000000, 1.000000000000000000, 1.000000000000000000, 1.000000000000000000) ) ) 
 REPRESENTATION_ITEM ( '' )  SURFACE ( )  );
#6731 = CARTESIAN_POINT ( 'NONE',  ( 6.615221834162048786, -49.23097633541600260, 14.16446777330088658 ) ) ;
#6732 = CARTESIAN_POINT ( 'NONE',  ( 0.2972598230769930017, 14.33493731733933352, 40.00000000000002132 ) ) ;
#6733 = ORIENTED_EDGE ( 'NONE', *, *, #26161, .F. ) ;
#6734 = CARTESIAN_POINT ( 'NONE',  ( -726.9846540392142060, -66.50000000000001421, 71.50000000000005684 ) ) ;
#6735 = CARTESIAN_POINT ( 'NONE',  ( -86.96347745069644475, -15.38646221621786125, -15.38646221621789856 ) ) ;
#6736 = CARTESIAN_POINT ( 'NONE',  ( -47.45115950054488252, -14.84795788660673388, 29.80449331795290746 ) ) ;
#6737 = CARTESIAN_POINT ( 'NONE',  ( -30.26275506840324070, 1.198031551616013601, 1.198031551616023371 ) ) ;
#6738 = CARTESIAN_POINT ( 'NONE',  ( -2.164901439688427409, 13.92557459412259391, -47.64638340556017226 ) ) ;
#6739 = CARTESIAN_POINT ( 'NONE',  ( 199.0205186365099905, -18.88915341724846542, -6.581556047429298673 ) ) ;
#6740 = CARTESIAN_POINT ( 'NONE',  ( 146.6084372240433709, 3.800685668858042821, 52.76785682606522698 ) ) ;
#6741 = CYLINDRICAL_SURFACE ( 'NONE', #10700, 5.000000000000004441 ) ;
#6742 = CYLINDRICAL_SURFACE ( 'NONE', #24945, 5.000000000000004441 ) ;
#6744 = CIRCLE ( 'NONE', #9286, 30.00000000000003908 ) ;
#6743 = CARTESIAN_POINT ( 'NONE',  ( -188.3066136396993784, -13.82848859481211967, 46.99300418776426369 ) ) ;
#6745 = CARTESIAN_POINT ( 'NONE',  ( -162.0762913951020892, -1.198031840385767266, -1.198031840385758384 ) ) ;
#6746 = B_SPLINE_CURVE_WITH_KNOTS ( 'NONE', 3,
 ( #2431, #14653, #23185, #8680, #16790, #8407 ),
 .UNSPECIFIED., .F., .F.,
 ( 4, 2, 4 ),
 ( 0.3689590070116580689, 0.3867117631979620773, 0.4044645193949217843 ),
 .UNSPECIFIED. ) ;
#6747 = CARTESIAN_POINT ( 'NONE',  ( 151.7948205124835681, 51.78348778862537927, 4.785054706298732086 ) ) ;
#6748 = CARTESIAN_POINT ( 'NONE',  ( 170.2234770963711128, -45.64576402573167258, -10.92277846919254891 ) ) ;
#6749 = CARTESIAN_POINT ( 'NONE',  ( 163.1118516004056573, 19.27778845538753316, 19.27778845538783870 ) ) ;
#6751 = CARTESIAN_POINT ( 'NONE',  ( -56.48582580120559271, 21.81201906317798489, -21.81201906317746619 ) ) ;
#6750 = CARTESIAN_POINT ( 'NONE',  ( -238.4067589809705794, -0.6820004457913585449, -0.6820004457913265705 ) ) ;
#6752 = CARTESIAN_POINT ( 'NONE',  ( 192.4448373802100889, -14.14213562375896061, 14.14213562375865330 ) ) ;
#6753 = CARTESIAN_POINT ( 'NONE',  ( 14.38125909742181285, -15.17850393972633505, 40.00000000000002132 ) ) ;
#6754 = CARTESIAN_POINT ( 'NONE',  ( -100.7734535825088500, -22.67402823373193499, -40.00000000000002132 ) ) ;
#6755 = CARTESIAN_POINT ( 'NONE',  ( 19.06497207195980792, 10.03556273973433299, 10.03556273973436319 ) ) ;
#6756 = DIRECTION ( 'NONE',  ( 1.000000000000000000, -1.836970198721030181E-16, -0.000000000000000000 ) ) ;
#6757 = CARTESIAN_POINT ( 'NONE',  ( -162.0762913951020892, -1.198031840315659124, -57.76657433523998009 ) ) ;
#6758 = CARTESIAN_POINT ( 'NONE',  ( -166.3490444790731431, 36.43931842064077387, -19.13701437385414295 ) ) ;
#6759 = ORIENTED_EDGE ( 'NONE', *, *, #24291, .T. ) ;
#6760 = CARTESIAN_POINT ( 'NONE',  ( -105.3755690713226585, -15.38646221621796251, 41.18208027870593924 ) ) ;
#6761 = LINE ( 'NONE', #3169, #9504 ) ;
#6762 = CARTESIAN_POINT ( 'NONE',  ( -198.0356074513804288, -39.15871834505936278, 39.15871834505892224 ) ) ;
#6763 = CARTESIAN_POINT ( 'NONE',  ( 11.71430589700012526, -49.28686712665649594, -14.17293196763931462 ) ) ;
#6764 = ORIENTED_EDGE ( 'NONE', *, *, #9798, .T. ) ;
#6765 = CARTESIAN_POINT ( 'NONE',  ( -102.4068193528139972, -20.44188272012875984, 8.088405365068716435 ) ) ;
#6766 = CARTESIAN_POINT ( 'NONE',  ( -82.24286367748180737, -12.41697925881799947, -15.97558298110162411 ) ) ;
#6767 = CARTESIAN_POINT ( 'NONE',  ( 199.9999999999998010, 6.097523047862603462, -17.99825575681430223 ) ) ;
#6768 = DIRECTION ( 'NONE',  ( 0.000000000000000000, 0.000000000000000000, 1.000000000000000000 ) ) ;
#6769 = AXIS2_PLACEMENT_3D ( 'NONE', #6336, #22588, #12593 ) ;
#6770 = CARTESIAN_POINT ( 'NONE',  ( 199.9999999999999432, 19.99999999999996092, 2.449293598294708485E-15 ) ) ;
#6771 = CARTESIAN_POINT ( 'NONE',  ( 19.06497207195980792, 10.03556273973447155, -10.03556273973422286 ) ) ;
#6772 = CARTESIAN_POINT ( 'NONE',  ( 199.0103760074104002, 19.48024492545154018, 4.564568505664855280 ) ) ;
#6773 = CARTESIAN_POINT ( 'NONE',  ( 14.38125909742183062, -67.30136555895943218, -10.73282306403629605 ) ) ;
#6774 = CARTESIAN_POINT ( 'NONE',  ( 151.7948205124836534, -40.00000000000001421, 6.767089262348889633 ) ) ;
#6775 = CARTESIAN_POINT ( 'NONE',  ( -238.4067589809705794, -4.716212492215116094E-14, 0.9644942799825824142 ) ) ;
#6776 = CARTESIAN_POINT ( 'NONE',  ( -196.0240701931631691, -24.63338802862617172, -44.60678453686448108 ) ) ;
#6777 = CARTESIAN_POINT ( 'NONE',  ( 14.38125909742182884, -55.17850393972636169, -2.449293598294708485E-15 ) ) ;
#6779 = CARTESIAN_POINT ( 'NONE',  ( -30.26275506840324070, -1.198031551616032919, 1.198031551616014712 ) ) ;
#6778 = CARTESIAN_POINT ( 'NONE',  ( 23.05038679986266459, -17.85133178553819988, -43.09692730307060060 ) ) ;
#6780 = CARTESIAN_POINT ( 'NONE',  ( -30.26275506840322649, -41.69427246844630019, -2.449293598294708485E-15 ) ) ;
#6781 = CARTESIAN_POINT ( 'NONE',  ( -198.0356074513804572, -10.87444709760996986, 67.44298959253333692 ) ) ;
#6782 = CARTESIAN_POINT ( 'NONE',  ( -105.3755690713226727, -2.472783935621397949E-13, 21.75974354311649961 ) ) ;
#6783 = CARTESIAN_POINT ( 'NONE',  ( -105.3394646353463600, 10.54672847198930796, -18.62482576791553868 ) ) ;
#6784 = CARTESIAN_POINT ( 'NONE',  ( 136.1360204305621551, 39.99999999999968026, 35.03383547441337953 ) ) ;
#6785 = CARTESIAN_POINT ( 'NONE',  ( -626.9846540392097722, 90.00000000000000000, 65.00000000000002842 ) ) ;
#6786 = FACE_BOUND ( 'NONE', #7595, .T. ) ;
#6787 = CARTESIAN_POINT ( 'NONE',  ( -102.4068193528165693, -8.735227608996721571, -20.17396017424868759 ) ) ;
#6788 = CARTESIAN_POINT ( 'NONE',  ( 14.38125909742183062, -67.30136555898262429, 10.73282306405838682 ) ) ;
#6789 = EDGE_LOOP ( 'NONE', ( #922, #13297, #29, #8963, #21305, #5042, #3190 ) ) ;
#6791 = CARTESIAN_POINT ( 'NONE',  ( -189.4799804244524637, 23.69387126430460455, -43.33513910317138595 ) ) ;
#6790 = CARTESIAN_POINT ( 'NONE',  ( 91.82158438592158234, 12.16597498397756993, 12.16597498397776356 ) ) ;
#6792 = DIRECTION ( 'NONE',  ( 0.000000000000000000, 0.000000000000000000, 1.000000000000000000 ) ) ;
#6793 = CARTESIAN_POINT ( 'NONE',  ( 91.82158438592159655, -22.79471317813468545, -40.00000000000002132 ) ) ;
#6794 = AXIS2_PLACEMENT_3D ( 'NONE', #19130, #6756, #13017 ) ;
#6795 = CARTESIAN_POINT ( 'NONE',  ( -126.6834154283321112, -24.04426794716115623, 11.16464792285850471 ) ) ;
#6796 = CARTESIAN_POINT ( 'NONE',  ( 170.2234770963711128, -17.36149277827010096, 17.36149277826970660 ) ) ;
#6797 = ORIENTED_EDGE ( 'NONE', *, *, #18157, .F. ) ;
#6798 = ORIENTED_EDGE ( 'NONE', *, *, #11501, .T. ) ;
#6799 = CARTESIAN_POINT ( 'NONE',  ( 199.9999999999999432, -8.412025548490841942, 17.05051154412392123 ) ) ;
#6800 = CARTESIAN_POINT ( 'NONE',  ( -103.9663809734325497, 8.574562933842363677, -19.92521373320581546 ) ) ;
#6801 = EDGE_LOOP ( 'NONE', ( #22734, #13558, #23865, #16077, #3711, #10171, #25272, #15979, #10431, #7557 ) ) ;
#6802 = VERTEX_POINT ( 'NONE', #26077 ) ;
#6803 = CARTESIAN_POINT ( 'NONE',  ( 19.06497207195980792, -18.24870850772763475, 38.31983398719622613 ) ) ;
#6804 = CARTESIAN_POINT ( 'NONE',  ( 199.0176767632675023, -16.26464645690579758, -11.64139296301337190 ) ) ;
#6805 = DIRECTION ( 'NONE',  ( 7.916033913021854848E-32, -4.182618615277681568E-16, -1.000000000000000000 ) ) ;
#6806 = CARTESIAN_POINT ( 'NONE',  ( 184.8905102610680444, -14.79361573936379415, -14.79361573936387941 ) ) ;
#6807 = CARTESIAN_POINT ( 'NONE',  ( -30.26275506840324070, 1.198031551616013601, 1.198031551616023371 ) ) ;
#6808 = CARTESIAN_POINT ( 'NONE',  ( -280.0000000000000000, 1.839446121267387017E-14, -20.00000000000001421 ) ) ;
#6809 = EDGE_CURVE ( 'NONE', #2387, #1721, #17460, .T. ) ;
#6810 = CARTESIAN_POINT ( 'NONE',  ( -88.38011429793466789, -8.298859913938862576, -20.03522015793668842 ) ) ;
#6811 = AXIS2_PLACEMENT_3D ( 'NONE', #25173, #24906, #8931 ) ;
#6812 = CARTESIAN_POINT ( 'NONE',  ( 57.59792236341148453, -40.00000000000003553, 2.435789363417741438 ) ) ;
#6813 = CARTESIAN_POINT ( 'NONE',  ( -86.96347745069645896, 39.99999999999977973, 21.75974354311691883 ) ) ;
#6814 = CARTESIAN_POINT ( 'NONE',  ( -82.28544635048413625, 18.14459473659407962, 8.922251332909290511 ) ) ;
#6815 = DIRECTION ( 'NONE',  ( 0.000000000000000000, -1.000000000000000000, 0.000000000000000000 ) ) ;
#6816 = CARTESIAN_POINT ( 'NONE',  ( 199.0057363775755448, 17.49143510765091492, -9.692886659233986180 ) ) ;
#6817 = CARTESIAN_POINT ( 'NONE',  ( -188.2956751479415232, 13.82790121914897341, 46.98904240251096809 ) ) ;
#6818 = CARTESIAN_POINT ( 'NONE',  ( -213.1075012329537230, -9.698598906450422774, -9.698598906450550672 ) ) ;
#6819 = CARTESIAN_POINT ( 'NONE',  ( 98.29820294270297154, 18.47759065022021474, -7.653668647299666006 ) ) ;
#6820 = CARTESIAN_POINT ( 'NONE',  ( -135.8532207217289738, 34.75652343174594705, 21.81201906317792449 ) ) ;
#6821 = CARTESIAN_POINT ( 'NONE',  ( -86.90968602926041342, -19.36074508460288257, 9.002619558043598147 ) ) ;
#6822 = CARTESIAN_POINT ( 'NONE',  ( -192.9588430854689705, -38.51493924976909966, -38.51493924976973915 ) ) ;
#6823 = CARTESIAN_POINT ( 'NONE',  ( -629.4215712140579626, 28.28427124746185228, 34.99999999999999289 ) ) ;
#6824 = CARTESIAN_POINT ( 'NONE',  ( 4.995406935893294431, -15.24977328854832415, 40.00000000000002132 ) ) ;
#6825 = CARTESIAN_POINT ( 'NONE',  ( -135.8532207217289738, 50.09629031063956006, 6.472252184284782217 ) ) ;
#6826 = CARTESIAN_POINT ( 'NONE',  ( 91.82158438592156813, 17.20528682183302038, 40.00000000000002132 ) ) ;
#6827 = CARTESIAN_POINT ( 'NONE',  ( 180.0000000000000000, -35.78896085774750446, -65.91016826501511616 ) ) ;
#6828 = VERTEX_POINT ( 'NONE', #26217 ) ;
#6829 = CARTESIAN_POINT ( 'NONE',  ( -280.0000000000000568, -40.00000000000028422, 19.99999999999959499 ) ) ;
#6830 = CARTESIAN_POINT ( 'NONE',  ( 199.0063920675446525, 6.513768699308227106, -18.94368432171033945 ) ) ;
#6831 = DIRECTION ( 'NONE',  ( 0.000000000000000000, 0.000000000000000000, 1.000000000000000000 ) ) ;
#6832 = ORIENTED_EDGE ( 'NONE', *, *, #19629, .F. ) ;
#6833 = ORIENTED_EDGE ( 'NONE', *, *, #3799, .F. ) ;
#6834 = ORIENTED_EDGE ( 'NONE', *, *, #23543, .F. ) ;
#6835 = CARTESIAN_POINT ( 'NONE',  ( -56.48582580120559982, 30.84685318188643421, 40.00000000000002132 ) ) ;
#6836 = SURFACE_STYLE_FILL_AREA ( #12836 ) ;
#6837 =( BOUNDED_SURFACE ( )  B_SPLINE_SURFACE ( 3, 3, ( 
 ( #272, #14626, #24498, #2403, #22632, #8380, #24627, #10653, #25029, #6782, #4809, #4407, #16633, #6384, #14501, #12640, #20629, #18628, #411, #13541, #25161, #21541, #21162, #23159, #17406, #5063, #3315, #15284, #23535, #3441 ),
 ( #23660, #15029, #9426, #9302, #21667, #11413, #17285, #7417, #19535, #4938, #1320, #6912, #13044, #19663, #3064, #19156, #11045, #15532, #23415, #2935, #17533, #21290, #13169, #15410, #5191, #11295, #7296, #11166, #25671, #7045 ),
 ( #11539, #25547, #5306, #19282, #940, #17154, #1065, #13418, #1450, #5440, #17025, #9172, #9049, #25288, #15162, #23287, #13293, #25419, #7168, #21414, #3187, #19413, #1197, #17659, #14075, #15923, #25800, #18189, #3842, #16201 ),
 ( #24334, #22339, #24056, #7548, #5567, #12078, #5832, #7807, #12212, #26340, #17791, #20200, #17925, #26069, #9822, #23917, #13935, #9550, #22070, #9685, #11946, #1712, #20071, #1847, #4115, #9950, #8082, #15790, #15660, #16064 ),
 ( #5692, #22206, #18059, #24191, #20334, #5964, #26210, #7946, #1979, #10085, #25936, #3981, #7678, #6098, #14205, #23786, #13673, #21795, #3567, #13797, #11671, #19795, #1582, #21932, #11809, #3707, #19929, #10220, #24732, #8350 ),
 ( #10618, #20468, #24462, #6488, #16731, #18732, #22603, #22730, #12609, #108, #16471, #18599, #20597, #515, #8620, #6227, #24862, #2243, #14470, #8215, #6617, #12745, #16333, #14340, #14734, #20865, #16599, #4508, #10350, #24596 ),
 ( #2111, #22866, #22471, #4250, #14600, #6351, #4643, #2373, #20738, #2649, #2507, #377, #18327, #12340, #18460, #8482, #238, #4379, #12470, #10485, #23873, #15743, #3659, #18013, #7764, #26297, #11766, #12035, #14295, #1804 ) ),
 .UNSPECIFIED., .T., .F., .F. ) 
 B_SPLINE_SURFACE_WITH_KNOTS ( ( 4, 3, 4 ),
 ( 4, 2, 2, 2, 2, 2, 2, 2, 2, 2, 2, 2, 2, 2, 4 ),
 ( 0.000000000000000000, 0.5000000000000000000, 1.000000000000000000 ),
 ( 0.000000000000000000, 0.1357259735107005372, 0.1651108541090157700, 0.1944957347073310028, 0.3598804999793158710, 0.3867117631979620773, 0.4135430264166082281, 0.5789277916885930964, 0.6062785021374117456, 0.6336292125862302838, 0.8508620842112317728, 0.8814014469398914198, 0.9119408096685510667, 0.9559704048342755334, 1.000000000000000000 ),
 .UNSPECIFIED. ) 
 GEOMETRIC_REPRESENTATION_ITEM ( )  RATIONAL_B_SPLINE_SURFACE ( (
 ( 1.000000000000000000, 1.000000000000000000, 1.000000000000000000, 1.000000000000000000, 1.000000000000000000, 1.000000000000000000, 1.000000000000000000, 1.000000000000000000, 1.000000000000000000, 1.000000000000000000, 1.000000000000000000, 1.000000000000000000, 1.000000000000000000, 1.000000000000000000, 1.000000000000000000, 1.000000000000000000, 1.000000000000000000, 1.000000000000000000, 1.000000000000000000, 1.000000000000000000, 1.000000000000000000, 1.000000000000000000, 1.000000000000000000, 1.000000000000000000, 1.000000000000000000, 1.000000000000000000, 1.000000000000000000, 1.000000000000000000, 1.000000000000000000, 1.000000000000000000),
 ( 0.3333333333333333703, 0.3333333333333333703, 0.3333333333333333703, 0.3333333333333333703, 0.3333333333333333703, 0.3333333333333333703, 0.3333333333333333703, 0.3333333333333333703, 0.3333333333333333703, 0.3333333333333333703, 0.3333333333333333703, 0.3333333333333333703, 0.3333333333333333703, 0.3333333333333333703, 0.3333333333333333703, 0.3333333333333333703, 0.3333333333333333703, 0.3333333333333333703, 0.3333333333333333703, 0.3333333333333333703, 0.3333333333333333703, 0.3333333333333333703, 0.3333333333333333703, 0.3333333333333333703, 0.3333333333333333703, 0.3333333333333333703, 0.3333333333333333703, 0.3333333333333333703, 0.3333333333333333703, 0.3333333333333333703),
 ( 0.3333333333333333703, 0.3333333333333333703, 0.3333333333333333703, 0.3333333333333333703, 0.3333333333333333703, 0.3333333333333333703, 0.3333333333333333703, 0.3333333333333333703, 0.3333333333333333703, 0.3333333333333333703, 0.3333333333333333703, 0.3333333333333333703, 0.3333333333333333703, 0.3333333333333333703, 0.3333333333333333703, 0.3333333333333333703, 0.3333333333333333703, 0.3333333333333333703, 0.3333333333333333703, 0.3333333333333333703, 0.3333333333333333703, 0.3333333333333333703, 0.3333333333333333703, 0.3333333333333333703, 0.3333333333333333703, 0.3333333333333333703, 0.3333333333333333703, 0.3333333333333333703, 0.3333333333333333703, 0.3333333333333333703),
 ( 1.000000000000000000, 1.000000000000000000, 1.000000000000000000, 1.000000000000000000, 1.000000000000000000, 1.000000000000000000, 1.000000000000000000, 1.000000000000000000, 1.000000000000000000, 1.000000000000000000, 1.000000000000000000, 1.000000000000000000, 1.000000000000000000, 1.000000000000000000, 1.000000000000000000, 1.000000000000000000, 1.000000000000000000, 1.000000000000000000, 1.000000000000000000, 1.000000000000000000, 1.000000000000000000, 1.000000000000000000, 1.000000000000000000, 1.000000000000000000, 1.000000000000000000, 1.000000000000000000, 1.000000000000000000, 1.000000000000000000, 1.000000000000000000, 1.000000000000000000),
 ( 0.3333333333333333703, 0.3333333333333333703, 0.3333333333333333703, 0.3333333333333333703, 0.3333333333333333703, 0.3333333333333333703, 0.3333333333333333703, 0.3333333333333333703, 0.3333333333333333703, 0.3333333333333333703, 0.3333333333333333703, 0.3333333333333333703, 0.3333333333333333703, 0.3333333333333333703, 0.3333333333333333703, 0.3333333333333333703, 0.3333333333333333703, 0.3333333333333333703, 0.3333333333333333703, 0.3333333333333333703, 0.3333333333333333703, 0.3333333333333333703, 0.3333333333333333703, 0.3333333333333333703, 0.3333333333333333703, 0.3333333333333333703, 0.3333333333333333703, 0.3333333333333333703, 0.3333333333333333703, 0.3333333333333333703),
 ( 0.3333333333333333703, 0.3333333333333333703, 0.3333333333333333703, 0.3333333333333333703, 0.3333333333333333703, 0.3333333333333333703, 0.3333333333333333703, 0.3333333333333333703, 0.3333333333333333703, 0.3333333333333333703, 0.3333333333333333703, 0.3333333333333333703, 0.3333333333333333703, 0.3333333333333333703, 0.3333333333333333703, 0.3333333333333333703, 0.3333333333333333703, 0.3333333333333333703, 0.3333333333333333703, 0.3333333333333333703, 0.3333333333333333703, 0.3333333333333333703, 0.3333333333333333703, 0.3333333333333333703, 0.3333333333333333703, 0.3333333333333333703, 0.3333333333333333703, 0.3333333333333333703, 0.3333333333333333703, 0.3333333333333333703),
 ( 1.000000000000000000, 1.000000000000000000, 1.000000000000000000, 1.000000000000000000, 1.000000000000000000, 1.000000000000000000, 1.000000000000000000, 1.000000000000000000, 1.000000000000000000, 1.000000000000000000, 1.000000000000000000, 1.000000000000000000, 1.000000000000000000, 1.000000000000000000, 1.000000000000000000, 1.000000000000000000, 1.000000000000000000, 1.000000000000000000, 1.000000000000000000, 1.000000000000000000, 1.000000000000000000, 1.000000000000000000, 1.000000000000000000, 1.000000000000000000, 1.000000000000000000, 1.000000000000000000, 1.000000000000000000, 1.000000000000000000, 1.000000000000000000, 1.000000000000000000) ) ) 
 REPRESENTATION_ITEM ( '' )  SURFACE ( )  );
#6838 = CARTESIAN_POINT ( 'NONE',  ( -110.0947178154516877, -20.04333087340630115, 2.529241932050243058 ) ) ;
#6839 = CARTESIAN_POINT ( 'NONE',  ( -199.9999999999999716, 51.72223107510019702, 14.31382256974095490 ) ) ;
#6840 = CARTESIAN_POINT ( 'NONE',  ( -105.3755690713226585, -39.99999999999996447, -21.75974354311664527 ) ) ;
#6841 = CARTESIAN_POINT ( 'NONE',  ( 199.9999999999998863, 9.229831349313808886, -16.61069465220444386 ) ) ;
#6842 = AXIS2_PLACEMENT_3D ( 'NONE', #9932, #8063, #18038 ) ;
#6843 = CARTESIAN_POINT ( 'NONE',  ( 199.9999999999999147, 8.398447161810446815, -17.04410699012685271 ) ) ;
#6844 = VECTOR ( 'NONE', #7582, 1000.000000000000000 ) ;
#6845 = CARTESIAN_POINT ( 'NONE',  ( -208.1127848780264742, -17.67593391476605547, -38.89260858015755673 ) ) ;
#6846 = CARTESIAN_POINT ( 'NONE',  ( 170.2234770963711128, -10.92277846919235529, 45.64576402573175073 ) ) ;
#6847 = AXIS2_PLACEMENT_3D ( 'NONE', #3591, #9845, #19089 ) ;
#6848 = CARTESIAN_POINT ( 'NONE',  ( 210.0000000000000284, 72.72568232011447265, -59.67546976104962653 ) ) ;
#6849 = CARTESIAN_POINT ( 'NONE',  ( -100.7734535825088500, -39.99999999999986500, -17.32597176626853397 ) ) ;
#6850 = DIRECTION ( 'NONE',  ( 0.000000000000000000, 1.000000000000000000, 0.000000000000000000 ) ) ;
#6851 = CARTESIAN_POINT ( 'NONE',  ( 0.2972598230769983307, -14.33493731733933352, 0.000000000000000000 ) ) ;
#6852 = CARTESIAN_POINT ( 'NONE',  ( -238.4067589809705794, -28.96627169325343942, 28.96627169325309126 ) ) ;
#6853 = CARTESIAN_POINT ( 'NONE',  ( 199.0055953282818564, 16.96762334911333880, -10.59856222037965345 ) ) ;
#6855 = CARTESIAN_POINT ( 'NONE',  ( -100.7734535825088358, 6.065416334915073333E-14, -22.67402823373191723 ) ) ;
#6854 = CARTESIAN_POINT ( 'NONE',  ( 4.995406935893289102, 10.78321810389013002, -10.78321810388986712 ) ) ;
#6856 = CARTESIAN_POINT ( 'NONE',  ( -259.2033419157646676, -9.517827891722680178, 0.000000000000000000 ) ) ;
#6857 = CARTESIAN_POINT ( 'NONE',  ( 146.6084372240433993, -24.48358557860319706, -24.48358557860330720 ) ) ;
#6858 = CARTESIAN_POINT ( 'NONE',  ( -259.2033419157646676, 30.48217210827734647, 40.00000000000002132 ) ) ;
#6859 = EDGE_LOOP ( 'NONE', ( #21551, #9429, #11241, #12552 ) ) ;
#6860 = EDGE_CURVE ( 'NONE', #17170, #17304, #5995, .T. ) ;
#6861 = CARTESIAN_POINT ( 'NONE',  ( -2.557884977069448063, -43.43882039328137523, 23.77085849409481000 ) ) ;
#6862 = VECTOR ( 'NONE', #25820, 1000.000000000000114 ) ;
#6863 = CARTESIAN_POINT ( 'NONE',  ( -105.3755690713226585, -21.75974354311652448, -40.00000000000002132 ) ) ;
#6864 = DIRECTION ( 'NONE',  ( 0.000000000000000000, -0.3656393565653622280, 0.9307566067079341421 ) ) ;
#6865 = CARTESIAN_POINT ( 'NONE',  ( 19.06497207195981858, 10.03556273973424062, 66.60410523465820631 ) ) ;
#6866 = CARTESIAN_POINT ( 'NONE',  ( -62.69292774211698571, -9.343531400666156728, 25.97703433363412628 ) ) ;
#6867 = CARTESIAN_POINT ( 'NONE',  ( -77.60240544034114407, 21.88152835081340797, 3.050660596052795714 ) ) ;
#6868 = EDGE_CURVE ( 'NONE', #9833, #25465, #15521, .T. ) ;
#6869 = EDGE_CURVE ( 'NONE', #4791, #6305, #9382, .T. ) ;
#6870 = CARTESIAN_POINT ( 'NONE',  ( -7.726389047741937688, 17.45517700520669280, -42.14052505958233041 ) ) ;
#6871 = CARTESIAN_POINT ( 'NONE',  ( 199.0235864634049108, -19.99353228191618825, 0.6599136639449380004 ) ) ;
#6872 = CARTESIAN_POINT ( 'NONE',  ( 130.8568914410475372, -24.07718906447255947, 24.07718906447199458 ) ) ;
#6873 = DIRECTION ( 'NONE',  ( 0.000000000000000000, -1.000000000000000000, 0.000000000000000000 ) ) ;
#6874 = CARTESIAN_POINT ( 'NONE',  ( -188.3611024622287857, -13.83140737835751821, 47.01268868735293438 ) ) ;
#6875 = CARTESIAN_POINT ( 'NONE',  ( 151.7948205124836534, 23.49921654116009506, 33.06932595376371609 ) ) ;
#6876 = CARTESIAN_POINT ( 'NONE',  ( 200.0000000000000000, -14.14213562373046784, -42.42640687119298804 ) ) ;
#6877 = AXIS2_PLACEMENT_3D ( 'NONE', #1695, #9800, #17905 ) ;
#6879 = CARTESIAN_POINT ( 'NONE',  ( -208.1127848780264742, 67.17687982763172272, -10.60833733270698254 ) ) ;
#6878 = CARTESIAN_POINT ( 'NONE',  ( -200.4318156386405008, 14.17468120671562737, -49.29858106685321673 ) ) ;
#6880 = CARTESIAN_POINT ( 'NONE',  ( -280.0000000000000568, -14.14213562373049449, -42.42640687119305198 ) ) ;
#6881 = CARTESIAN_POINT ( 'NONE',  ( -100.7734535825088500, 22.67402823373189946, 40.00000000000002132 ) ) ;
#6882 = CARTESIAN_POINT ( 'NONE',  ( 4.995406935893289102, 55.24977328856464709, -40.00000000000002132 ) ) ;
#6883 = B_SPLINE_CURVE_WITH_KNOTS ( 'NONE', 3,
 ( #21090, #602, #10714, #12698, #19217, #741, #23094, #25091, #16824, #19090 ),
 .UNSPECIFIED., .F., .F.,
 ( 4, 2, 2, 2, 4 ),
 ( 0.7921542097164085972, 0.8508620842112317728, 0.8814014469398914198, 0.9119408096685510667, 0.9406682828394935525 ),
 .UNSPECIFIED. ) ;
#6884 = CARTESIAN_POINT ( 'NONE',  ( -162.0762913951020892, 1.198031840385716418, 1.198031840385750169 ) ) ;
#6885 =( BOUNDED_CURVE ( )  B_SPLINE_CURVE ( 3, ( #2465, #18964, #474, #8580 ),
 .UNSPECIFIED., .F., .F. ) 
 B_SPLINE_CURVE_WITH_KNOTS ( ( 4, 4 ),
 ( 0.01388163287021778290, 0.02359082919309994641 ),
 .UNSPECIFIED. ) 
 CURVE ( )  GEOMETRIC_REPRESENTATION_ITEM ( )  RATIONAL_B_SPLINE_CURVE ( ( 1.000000000000000000, 0.8672072324488997452, 0.7608653435686203448, 0.6809743333591616876 ) ) 
 REPRESENTATION_ITEM ( '' )  );
#6886 = PLANE ( 'NONE',  #25922 ) ;
#6887 = CARTESIAN_POINT ( 'NONE',  ( -135.8532207217289738, -21.81201906317806305, 34.75652343174590442 ) ) ;
#6888 = CARTESIAN_POINT ( 'NONE',  ( -188.3120147333423233, 46.99495896211633550, -13.82877842034795002 ) ) ;
#6889 = EDGE_LOOP ( 'NONE', ( #827, #7372 ) ) ;
#6890 = CARTESIAN_POINT ( 'NONE',  ( 163.1118516004056573, -19.27778845539233998, 37.29075403953149959 ) ) ;
#6891 = EDGE_CURVE ( 'NONE', #24783, #6149, #10356, .T. ) ;
#6892 = CARTESIAN_POINT ( 'NONE',  ( -82.23726319241512783, -15.17211809665081290, -13.38817034152228480 ) ) ;
#6893 = CARTESIAN_POINT ( 'NONE',  ( -105.3755690713226585, 15.38646221621762678, 41.18208027870604582 ) ) ;
#6894 = CARTESIAN_POINT ( 'NONE',  ( -47.45115950031290453, -31.57405104348713110, -10.57586762648235634 ) ) ;
#6895 = ORIENTED_EDGE ( 'NONE', *, *, #25351, .F. ) ;
#6896 = CARTESIAN_POINT ( 'NONE',  ( -151.4802849341727438, -31.86309571749480796, 16.17241510390670456 ) ) ;
#6897 = CARTESIAN_POINT ( 'NONE',  ( -110.0961828203647741, -12.41698901629497520, -15.97557204180744961 ) ) ;
#6898 = CARTESIAN_POINT ( 'NONE',  ( 200.0000000000001705, 6.971423609723053971, -17.67803530771774589 ) ) ;
#6899 = CARTESIAN_POINT ( 'NONE',  ( -200.0000000000000000, 0.000000000000000000, 0.000000000000000000 ) ) ;
#6900 = CARTESIAN_POINT ( 'NONE',  ( -135.8532207217289738, 30.84685318188643777, -40.00000000000002132 ) ) ;
#6901 = DIRECTION ( 'NONE',  ( 0.000000000000000000, 0.9767746502210202797, -0.2142691827715865471 ) ) ;
#6902 = CARTESIAN_POINT ( 'NONE',  ( 199.0183491629479988, 10.55513269831597079, 16.99244513920028510 ) ) ;
#6903 = CARTESIAN_POINT ( 'NONE',  ( -259.2033419157646676, 6.730120644403426944, 6.730120644403592145 ) ) ;
#6904 = CARTESIAN_POINT ( 'NONE',  ( 192.4448373802100889, -3.692737725850373501E-14, 19.99999999996060751 ) ) ;
#6905 = CARTESIAN_POINT ( 'NONE',  ( 130.8568914410475088, 40.00000000000002842, 5.949712681206834830 ) ) ;
#6906 = CARTESIAN_POINT ( 'NONE',  ( -3.763361371728497051, 47.08953757622920477, -13.84281709279659189 ) ) ;
#6907 = CARTESIAN_POINT ( 'NONE',  ( 91.82158438592156813, 17.20528682183302038, -40.00000000000002132 ) ) ;
#6909 = CARTESIAN_POINT ( 'NONE',  ( -616.1677987530077871, 28.57178177696692245, 27.99862729771767889 ) ) ;
#6908 = CARTESIAN_POINT ( 'NONE',  ( 22.57783252600391322, -17.90541116499574414, -43.22748647439809133 ) ) ;
#6910 = CARTESIAN_POINT ( 'NONE',  ( -105.3755690713226585, -18.24025645688355013, 40.00000000000002132 ) ) ;
#6911 = CARTESIAN_POINT ( 'NONE',  ( 91.82158438592156813, 40.45024623143950038, 16.11829626348447420 ) ) ;
#6912 = CARTESIAN_POINT ( 'NONE',  ( -91.56559293963836410, 39.99999999999976552, 22.67402823373234000 ) ) ;
#6913 = CARTESIAN_POINT ( 'NONE',  ( -110.0574180502660653, 18.01801597164610413, -9.169691069488823842 ) ) ;
#6914 = CARTESIAN_POINT ( 'NONE',  ( 14.38125909742182529, -39.99999999999944578, -55.17850393971050238 ) ) ;
#6915 = CARTESIAN_POINT ( 'NONE',  ( 163.1118516004056573, -19.27778845538761132, -19.27778845538770724 ) ) ;
#6916 = DIRECTION ( 'NONE',  ( 0.000000000000000000, 0.000000000000000000, 1.000000000000000000 ) ) ;
#6917 = CARTESIAN_POINT ( 'NONE',  ( 19.06497207195980792, 10.03556273973447155, -10.03556273973422286 ) ) ;
#6918 = CARTESIAN_POINT ( 'NONE',  ( 163.1118516004056573, 19.27778845539212327, 37.29075403953164169 ) ) ;
#6919 = ORIENTED_EDGE ( 'NONE', *, *, #15646, .T. ) ;
#6921 = CARTESIAN_POINT ( 'NONE',  ( -5.866564133101147327, 42.46617576964662533, -23.09290806363647874 ) ) ;
#6920 = CARTESIAN_POINT ( 'NONE',  ( -86.91014751117377557, 19.35827336066830995, -9.009177718430029458 ) ) ;
#6922 = DIRECTION ( 'NONE',  ( 0.000000000000000000, 0.000000000000000000, 1.000000000000000000 ) ) ;
#6923 = CARTESIAN_POINT ( 'NONE',  ( 151.7948205124836534, -6.767089262349006873, 40.00000000000002132 ) ) ;
#6924 = CARTESIAN_POINT ( 'NONE',  ( -114.5450021253294892, 9.945938879699479429, -19.55077795857054213 ) ) ;
#6925 = CARTESIAN_POINT ( 'NONE',  ( -189.5227390968178725, 43.46195835885794168, -18.00253259953321461 ) ) ;
#6926 = VERTEX_POINT ( 'NONE', #4124 ) ;
#6927 = VERTEX_POINT ( 'NONE', #4517 ) ;
#6928 = CARTESIAN_POINT ( 'NONE',  ( 199.9999999999999432, -5.384370329785186371, 18.23197071264586810 ) ) ;
#6929 = CARTESIAN_POINT ( 'NONE',  ( 98.29820294267857150, 5.170639833979637778, 19.50609486047177299 ) ) ;
#6930 = ORIENTED_EDGE ( 'NONE', *, *, #15342, .F. ) ;
#6931 = ORIENTED_EDGE ( 'NONE', *, *, #11657, .T. ) ;
#6932 = CARTESIAN_POINT ( 'NONE',  ( -105.3755690713226585, -43.67073346367983788, 12.89780903124397149 ) ) ;
#6933 = CARTESIAN_POINT ( 'NONE',  ( 199.0228518427889242, -19.96294788386713037, -1.312843269464072815 ) ) ;
#6934 = CARTESIAN_POINT ( 'NONE',  ( -110.0368417077423118, -7.441767002991612756, 18.74474319003509137 ) ) ;
#6935 = CARTESIAN_POINT ( 'NONE',  ( 130.8568914410475372, -24.07718906447222551, -24.07718906447233209 ) ) ;
#6936 = CARTESIAN_POINT ( 'NONE',  ( 136.1360204305621266, -24.77266263493116583, -24.77266263493127951 ) ) ;
#6937 = CARTESIAN_POINT ( 'NONE',  ( -213.1075012329537230, 39.99999999999992895, 13.71589010951925935 ) ) ;
#6938 = CYLINDRICAL_SURFACE ( 'NONE', #15983, 5.000000000000004441 ) ;
#6939 = DIRECTION ( 'NONE',  ( -0.000000000000000000, 1.000000000000000000, -0.000000000000000000 ) ) ;
#6940 = CARTESIAN_POINT ( 'NONE',  ( 200.0000000000000000, -40.00000000000019185, 19.99999999999968381 ) ) ;
#6941 = CARTESIAN_POINT ( 'NONE',  ( 184.8905102610680444, 40.00000000000025580, -19.07866798485515503 ) ) ;
#6942 = CARTESIAN_POINT ( 'NONE',  ( -82.24337801438862527, 15.81455109355221111, 12.55991608931321224 ) ) ;
#6943 = PLANE ( 'NONE',  #1766 ) ;
#6944 = CARTESIAN_POINT ( 'NONE',  ( 199.0055466334479206, 16.72508833076945223, -10.95857635003404873 ) ) ;
#6945 = CARTESIAN_POINT ( 'NONE',  ( -175.9235632132996443, 39.35891845671766731, -21.03681927240882743 ) ) ;
#6946 = CARTESIAN_POINT ( 'NONE',  ( -238.4067589809705794, -0.6820004457913585449, -0.6820004457913265705 ) ) ;
#6947 = FACE_OUTER_BOUND ( 'NONE', #24785, .T. ) ;
#6948 = PLANE ( 'NONE',  #10594 ) ;
#6949 = CARTESIAN_POINT ( 'NONE',  ( -77.59802414163006290, 21.90520607601874659, 2.969683337867993878 ) ) ;
#6950 = CARTESIAN_POINT ( 'NONE',  ( 19.06497207195981858, -10.03556273973377166, -66.60410523465827737 ) ) ;
#6951 = CARTESIAN_POINT ( 'NONE',  ( -658.1673319222918508, 42.09494090835337232, 16.06443073066892779 ) ) ;
#6952 = CARTESIAN_POINT ( 'NONE',  ( -77.90255099906772784, 8.644468104261493480, 20.04994828523958361 ) ) ;
#6953 = ADVANCED_FACE ( 'NONE', ( #6495 ), #22311, .T. ) ;
#6954 = EDGE_LOOP ( 'NONE', ( #6267, #5844, #14388, #18509 ) ) ;
#6955 = CARTESIAN_POINT ( 'NONE',  ( 0.2972598230769907257, 66.70487387989869887, -10.13633138497392494 ) ) ;
#6956 = CARTESIAN_POINT ( 'NONE',  ( -30.26275506840324070, -1.694272468446265112, 0.000000000000000000 ) ) ;
#6957 = CARTESIAN_POINT ( 'NONE',  ( -592.2265799526504679, 44.81207692804512988, 4.151637030843666309 ) ) ;
#6958 = EDGE_LOOP ( 'NONE', ( #20047, #1295, #8364, #21718 ) ) ;
#6959 = CARTESIAN_POINT ( 'NONE',  ( 19.06497207195982924, -39.99999999999945288, -54.19242893257885640 ) ) ;
#6960 = CARTESIAN_POINT ( 'NONE',  ( 199.0110600102923115, -5.983788757275610770, -19.08445727264177094 ) ) ;
#6961 = EDGE_CURVE ( 'NONE', #23006, #20872, #25251, .T. ) ;
#6962 = FACE_OUTER_BOUND ( 'NONE', #15182, .T. ) ;
#6963 = VERTEX_POINT ( 'NONE', #522 ) ;
#6964 = VERTEX_POINT ( 'NONE', #24870 ) ;
#6965 = VERTEX_POINT ( 'NONE', #12753 ) ;
#6966 = CARTESIAN_POINT ( 'NONE',  ( 4.995406935893288214, 55.24977328854835434, 2.449293598294708485E-15 ) ) ;
#6967 = EDGE_CURVE ( 'NONE', #12692, #10794, #6761, .T. ) ;
#6968 = CARTESIAN_POINT ( 'NONE',  ( -190.0000000000000000, 66.50000000000009948, -66.50000000000005684 ) ) ;
#6969 = EDGE_CURVE ( 'NONE', #1593, #18580, #1177, .T. ) ;
#6970 = AXIS2_PLACEMENT_3D ( 'NONE', #3548, #25913, #23896 ) ;
#6971 = CARTESIAN_POINT ( 'NONE',  ( -716.9846540392142060, 66.50000000000009948, -61.50000000000004974 ) ) ;
#6972 = CARTESIAN_POINT ( 'NONE',  ( -208.1127848780264742, -40.00000000000011369, 15.00245453012655439 ) ) ;
#6973 = CARTESIAN_POINT ( 'NONE',  ( 199.9999999999998295, 1.074487055219422560, -18.97158139261448540 ) ) ;
#6974 = DIRECTION ( 'NONE',  ( -1.000000000000000000, -1.836970198721030181E-16, 0.000000000000000000 ) ) ;
#6975 = CARTESIAN_POINT ( 'NONE',  ( 146.6084372240433709, -24.48358557860284179, -32.08495691632087699 ) ) ;
#6976 = CARTESIAN_POINT ( 'NONE',  ( 146.6084372240433993, 24.48358557860307272, 24.48358557860347418 ) ) ;
#6977 = CARTESIAN_POINT ( 'NONE',  ( -88.37548150066159280, 20.03288105173027844, 8.297891025033743873 ) ) ;
#6978 = CARTESIAN_POINT ( 'NONE',  ( 136.1360204305621266, 7.947488714877270288E-14, -4.966164525587064560 ) ) ;
#6979 = CARTESIAN_POINT ( 'NONE',  ( -86.96347745069644475, 15.38646221621772092, 15.38646221621800336 ) ) ;
#6980 = CARTESIAN_POINT ( 'NONE',  ( 57.59792236341147031, 2.435789363418171760, 0.000000000000000000 ) ) ;
#6981 = CARTESIAN_POINT ( 'NONE',  ( 184.8905102610680444, -13.49065550809810965, 13.49065550809799596 ) ) ;
#6982 = CARTESIAN_POINT ( 'NONE',  ( -135.8532207217289738, 9.153146818113546246, -0.000000000000000000 ) ) ;
#6984 = CARTESIAN_POINT ( 'NONE',  ( 19.06497207195981147, -4.605042221739098431E-14, 14.19242893257840521 ) ) ;
#6983 = CARTESIAN_POINT ( 'NONE',  ( 146.6084372240433709, -24.48358557860284179, -32.08495691632087699 ) ) ;
#6985 = CARTESIAN_POINT ( 'NONE',  ( -135.8532207217289738, -9.153146818113595984, 0.000000000000000000 ) ) ;
#6986 = CARTESIAN_POINT ( 'NONE',  ( -208.1127848780264742, 10.60833733270764867, 67.17687982763166588 ) ) ;
#6987 = CARTESIAN_POINT ( 'NONE',  ( 136.1360204305621551, -35.03383547441293899, 40.00000000000002132 ) ) ;
#6988 = EDGE_LOOP ( 'NONE', ( #4306, #1368, #2701, #10269 ) ) ;
#6989 = CARTESIAN_POINT ( 'NONE',  ( 20.17262239844370697, -43.80323544018611415, 18.14389419513820201 ) ) ;
#6990 =( BOUNDED_SURFACE ( )  B_SPLINE_SURFACE ( 3, 3, ( 
 ( #6429, #2058, #20005, #24272, #6044, #10164, #8287, #22545, #4325, #2314, #12416, #10422, #14547, #12546, #8964, #10829, #20678, #13090, #25074, #11087, #24807, #19203, #590, #9090, #14943, #2585, #16676, #21074, #18810, #25334 ),
 ( #12683, #15072, #12825, #20946, #4719, #8697, #2724, #4451, #18944, #4586, #725, #22939, #16808, #23078, #24946, #6559, #6693, #12955, #17197, #14807, #14674, #4983, #2447, #22810, #21207, #4850, #985, #10699, #7091, #10558 ),
 ( #20813, #17073, #8829, #16939, #15205, #18671, #457, #8561, #6825, #2859, #10966, #23203, #19073, #855, #25207, #6955, #2979, #5108, #15577, #1238, #17328, #5609, #17702, #5229, #11583, #13581, #5354, #7463, #23701, #5481 ),
 ( #11719, #19450, #1624, #21708, #21455, #9217, #3486, #11334, #17833, #25590, #19703, #3230, #13213, #19838, #19578, #17574, #1491, #9597, #9343, #7336, #25846, #1369, #23577, #7590, #11454, #15328, #9467, #15702, #19325, #17451 ),
 ( #23826, #21335, #25462, #13715, #21840, #9731, #15450, #3609, #3106, #25980, #7721, #23333, #11210, #13461, #1109, #7213, #23455, #13333, #21581, #3353, #25711, #21975, #12122, #12381, #282, #18103, #26253, #20379, #20112, #11989 ),
 ( #24508, #10263, #24097, #19973, #16245, #6268, #152, #16107, #14245, #12256, #3747, #1889, #10129, #22247, #8256, #18373, #4292, #5872, #24238, #26112, #11853, #16374, #2281, #13841, #1754, #20509, #18501, #8128, #22385, #13979 ),
 ( #22112, #6011, #9994, #14120, #15972, #6137, #10390, #24374, #3889, #14382, #2153, #9863, #4022, #17965, #22514, #7851, #20247, #2027, #7988, #15831, #23961, #18231, #5736, #17, #4161, #22641, #14510, #20775, #2690, #14773 ) ),
 .UNSPECIFIED., .T., .F., .F. ) 
 B_SPLINE_SURFACE_WITH_KNOTS ( ( 4, 3, 4 ),
 ( 4, 2, 2, 2, 2, 2, 2, 2, 2, 2, 2, 2, 2, 2, 4 ),
 ( 0.000000000000000000, 0.5000000000000000000, 1.000000000000000000 ),
 ( 0.000000000000000000, 0.1357259735107005372, 0.1651108541090157700, 0.1944957347073310028, 0.3598804999793158710, 0.3867117631979620773, 0.4135430264166082281, 0.5789277916885930964, 0.6062785021374117456, 0.6336292125862302838, 0.8508620842112317728, 0.8814014469398914198, 0.9119408096685510667, 0.9559704048342755334, 1.000000000000000000 ),
 .UNSPECIFIED. ) 
 GEOMETRIC_REPRESENTATION_ITEM ( )  RATIONAL_B_SPLINE_SURFACE ( (
 ( 1.000000000000000000, 1.000000000000000000, 1.000000000000000000, 1.000000000000000000, 1.000000000000000000, 1.000000000000000000, 1.000000000000000000, 1.000000000000000000, 1.000000000000000000, 1.000000000000000000, 1.000000000000000000, 1.000000000000000000, 1.000000000000000000, 1.000000000000000000, 1.000000000000000000, 1.000000000000000000, 1.000000000000000000, 1.000000000000000000, 1.000000000000000000, 1.000000000000000000, 1.000000000000000000, 1.000000000000000000, 1.000000000000000000, 1.000000000000000000, 1.000000000000000000, 1.000000000000000000, 1.000000000000000000, 1.000000000000000000, 1.000000000000000000, 1.000000000000000000),
 ( 0.3333333333333333703, 0.3333333333333333703, 0.3333333333333333703, 0.3333333333333333703, 0.3333333333333333703, 0.3333333333333333703, 0.3333333333333333703, 0.3333333333333333703, 0.3333333333333333703, 0.3333333333333333703, 0.3333333333333333703, 0.3333333333333333703, 0.3333333333333333703, 0.3333333333333333703, 0.3333333333333333703, 0.3333333333333333703, 0.3333333333333333703, 0.3333333333333333703, 0.3333333333333333703, 0.3333333333333333703, 0.3333333333333333703, 0.3333333333333333703, 0.3333333333333333703, 0.3333333333333333703, 0.3333333333333333703, 0.3333333333333333703, 0.3333333333333333703, 0.3333333333333333703, 0.3333333333333333703, 0.3333333333333333703),
 ( 0.3333333333333333703, 0.3333333333333333703, 0.3333333333333333703, 0.3333333333333333703, 0.3333333333333333703, 0.3333333333333333703, 0.3333333333333333703, 0.3333333333333333703, 0.3333333333333333703, 0.3333333333333333703, 0.3333333333333333703, 0.3333333333333333703, 0.3333333333333333703, 0.3333333333333333703, 0.3333333333333333703, 0.3333333333333333703, 0.3333333333333333703, 0.3333333333333333703, 0.3333333333333333703, 0.3333333333333333703, 0.3333333333333333703, 0.3333333333333333703, 0.3333333333333333703, 0.3333333333333333703, 0.3333333333333333703, 0.3333333333333333703, 0.3333333333333333703, 0.3333333333333333703, 0.3333333333333333703, 0.3333333333333333703),
 ( 1.000000000000000000, 1.000000000000000000, 1.000000000000000000, 1.000000000000000000, 1.000000000000000000, 1.000000000000000000, 1.000000000000000000, 1.000000000000000000, 1.000000000000000000, 1.000000000000000000, 1.000000000000000000, 1.000000000000000000, 1.000000000000000000, 1.000000000000000000, 1.000000000000000000, 1.000000000000000000, 1.000000000000000000, 1.000000000000000000, 1.000000000000000000, 1.000000000000000000, 1.000000000000000000, 1.000000000000000000, 1.000000000000000000, 1.000000000000000000, 1.000000000000000000, 1.000000000000000000, 1.000000000000000000, 1.000000000000000000, 1.000000000000000000, 1.000000000000000000),
 ( 0.3333333333333333703, 0.3333333333333333703, 0.3333333333333333703, 0.3333333333333333703, 0.3333333333333333703, 0.3333333333333333703, 0.3333333333333333703, 0.3333333333333333703, 0.3333333333333333703, 0.3333333333333333703, 0.3333333333333333703, 0.3333333333333333703, 0.3333333333333333703, 0.3333333333333333703, 0.3333333333333333703, 0.3333333333333333703, 0.3333333333333333703, 0.3333333333333333703, 0.3333333333333333703, 0.3333333333333333703, 0.3333333333333333703, 0.3333333333333333703, 0.3333333333333333703, 0.3333333333333333703, 0.3333333333333333703, 0.3333333333333333703, 0.3333333333333333703, 0.3333333333333333703, 0.3333333333333333703, 0.3333333333333333703),
 ( 0.3333333333333333703, 0.3333333333333333703, 0.3333333333333333703, 0.3333333333333333703, 0.3333333333333333703, 0.3333333333333333703, 0.3333333333333333703, 0.3333333333333333703, 0.3333333333333333703, 0.3333333333333333703, 0.3333333333333333703, 0.3333333333333333703, 0.3333333333333333703, 0.3333333333333333703, 0.3333333333333333703, 0.3333333333333333703, 0.3333333333333333703, 0.3333333333333333703, 0.3333333333333333703, 0.3333333333333333703, 0.3333333333333333703, 0.3333333333333333703, 0.3333333333333333703, 0.3333333333333333703, 0.3333333333333333703, 0.3333333333333333703, 0.3333333333333333703, 0.3333333333333333703, 0.3333333333333333703, 0.3333333333333333703),
 ( 1.000000000000000000, 1.000000000000000000, 1.000000000000000000, 1.000000000000000000, 1.000000000000000000, 1.000000000000000000, 1.000000000000000000, 1.000000000000000000, 1.000000000000000000, 1.000000000000000000, 1.000000000000000000, 1.000000000000000000, 1.000000000000000000, 1.000000000000000000, 1.000000000000000000, 1.000000000000000000, 1.000000000000000000, 1.000000000000000000, 1.000000000000000000, 1.000000000000000000, 1.000000000000000000, 1.000000000000000000, 1.000000000000000000, 1.000000000000000000, 1.000000000000000000, 1.000000000000000000, 1.000000000000000000, 1.000000000000000000, 1.000000000000000000, 1.000000000000000000) ) ) 
 REPRESENTATION_ITEM ( '' )  SURFACE ( )  );
#6991 = CARTESIAN_POINT ( 'NONE',  ( -280.0000000000000568, 19.99999999999996447, -40.00000000000002132 ) ) ;
#6992 = CARTESIAN_POINT ( 'NONE',  ( -210.0000000000000284, 61.50000000000001421, -66.50000000000005684 ) ) ;
#6993 = CARTESIAN_POINT ( 'NONE',  ( 136.1360204305621266, 3.511608612530704665, 3.511608612530695339 ) ) ;
#6994 = LINE ( 'NONE', #3270, #20804 ) ;
#6995 = CARTESIAN_POINT ( 'NONE',  ( -1.258540240222670414, -13.96099832920753769, -47.88180740053038420 ) ) ;
#6996 = CARTESIAN_POINT ( 'NONE',  ( 199.0258841556672564, -17.79651494919816912, 9.142457329253240061 ) ) ;
#6997 = CARTESIAN_POINT ( 'NONE',  ( 57.59792236341147031, 26.56190807104652052, 30.00663442387728708 ) ) ;
#6998 = CARTESIAN_POINT ( 'NONE',  ( -77.90255099906852365, -20.29001641120231625, 8.064892378667423145 ) ) ;
#6999 = CARTESIAN_POINT ( 'NONE',  ( -86.86493150571115507, 7.943527260496353826, 19.77569912839162569 ) ) ;
#7000 = CARTESIAN_POINT ( 'NONE',  ( -200.4318156386405576, -14.17468120671533960, 49.29858106685333752 ) ) ;
#7001 = CARTESIAN_POINT ( 'NONE',  ( 91.82158438592158234, -1.633484621919921769E-13, 17.20528682183300262 ) ) ;
#7002 = ADVANCED_FACE ( 'NONE', ( #13151 ), #7017, .T. ) ;
#7003 = CARTESIAN_POINT ( 'NONE',  ( -192.9588430854690273, 18.05360324515418924, 38.51493924976949756 ) ) ;
#7004 = CARTESIAN_POINT ( 'NONE',  ( -77.70150415247218234, 11.19846400430064648, -18.99169997608993299 ) ) ;
#7005 = CARTESIAN_POINT ( 'NONE',  ( 14.38125909742181285, -10.73282306404712472, -10.73282306404731301 ) ) ;
#7007 = CARTESIAN_POINT ( 'NONE',  ( 192.4448373802101173, 42.42640687116487896, 14.14213562375934075 ) ) ;
#7006 = CARTESIAN_POINT ( 'NONE',  ( -198.0356074513804572, -10.87444709759714634, -10.87444709759729911 ) ) ;
#7008 = CARTESIAN_POINT ( 'NONE',  ( 57.59792236341147031, 54.84617931850878136, 1.722363176415705910 ) ) ;
#7009 = CARTESIAN_POINT ( 'NONE',  ( 14.38125909742180752, 55.17850393971008316, -40.00000000000002132 ) ) ;
#7010 = CARTESIAN_POINT ( 'NONE',  ( 0.2972598230769886718, 38.42060263243669027, -18.14793986248710667 ) ) ;
#7011 = LINE ( 'NONE', #15000, #25065 ) ;
#7012 = CARTESIAN_POINT ( 'NONE',  ( 146.6084372240433709, -32.08495691632075619, 24.48358557860298035 ) ) ;
#7013 = EDGE_CURVE ( 'NONE', #7472, #22554, #7287, .T. ) ;
#7014 = CARTESIAN_POINT ( 'NONE',  ( -183.1090696432183904, 41.47043467738880196, -22.43564075023506277 ) ) ;
#7015 = ORIENTED_EDGE ( 'NONE', *, *, #24602, .T. ) ;
#7016 = CARTESIAN_POINT ( 'NONE',  ( -91.56559293963834989, 12.25131212657480440, 12.25131212657486834 ) ) ;
#7017 = CYLINDRICAL_SURFACE ( 'NONE', #24391, 5.000000000000004441 ) ;
#7018 = CARTESIAN_POINT ( 'NONE',  ( -198.0356074513804572, 17.40982414986446969, 39.15871834505921356 ) ) ;
#7019 = CARTESIAN_POINT ( 'NONE',  ( -6.754359963570706782, -42.40682816666050314, -17.56548336385882791 ) ) ;
#7020 = EDGE_LOOP ( 'NONE', ( #13224, #188 ) ) ;
#7021 = CARTESIAN_POINT ( 'NONE',  ( -188.3508614409240067, -43.15762572182580215, 17.87647389380253315 ) ) ;
#7022 = B_SPLINE_CURVE_WITH_KNOTS ( 'NONE', 3,
 ( #23920, #7300, #3712, #11813, #19933, #24060 ),
 .UNSPECIFIED., .F., .F.,
 ( 4, 2, 4 ),
 ( -5.998621905159389411E-08, 0.03937827992696039947, 0.07875661984013984651 ),
 .UNSPECIFIED. ) ;
#7023 = AXIS2_PLACEMENT_3D ( 'NONE', #2949, #17417, #25431 ) ;
#7024 = CARTESIAN_POINT ( 'NONE',  ( 200.0000000000001990, 0.6082288760829889229, -18.99424756986708474 ) ) ;
#7025 = CARTESIAN_POINT ( 'NONE',  ( 36.88256715608616076, -16.19941669834411968, 39.10885149554682272 ) ) ;
#7026 = CARTESIAN_POINT ( 'NONE',  ( -135.8532207217289738, -9.153146818113595984, -40.00000000000002132 ) ) ;
#7027 = CARTESIAN_POINT ( 'NONE',  ( 45.01779936573458230, 18.90344565805356325, -36.09695843560584194 ) ) ;
#7028 = CARTESIAN_POINT ( 'NONE',  ( 199.0181823811410311, 10.83083347386195427, 16.81793973133765618 ) ) ;
#7029 = AXIS2_PLACEMENT_3D ( 'NONE', #15084, #10978, #996 ) ;
#7030 = VECTOR ( 'NONE', #407, 1000.000000000000000 ) ;
#7031 = B_SPLINE_CURVE_WITH_KNOTS ( 'NONE', 3,
 ( #23281, #21408, #13534, #15404, #3560, #25282, #13287, #3181, #25539, #11287, #7290, #23529, #21659, #3431 ),
 .UNSPECIFIED., .F., .F.,
 ( 4, 2, 2, 2, 2, 2, 4 ),
 ( 6.938893903907228378E-18, 0.002941681445496982863, 0.004412522168245476030, 0.005883362890993969196, 0.008825044336490964203, 0.01029588505923946344, 0.01176672578198796094 ),
 .UNSPECIFIED. ) ;
#7032 = B_SPLINE_CURVE_WITH_KNOTS ( 'NONE', 3,
 ( #9818, #22067, #21792, #22203, #11668, #11942, #3978, #7943 ),
 .UNSPECIFIED., .F., .F.,
 ( 4, 2, 2, 4 ),
 ( -5.298247996756991549E-05, 0.001923793760059295263, 0.003900570000086160151, 0.007854122480139891227 ),
 .UNSPECIFIED. ) ;
#7033 = CARTESIAN_POINT ( 'NONE',  ( 0.2972598230770027716, -38.42060263243681817, 18.14793986248684377 ) ) ;
#7034 = CARTESIAN_POINT ( 'NONE',  ( -30.26275506840324425, 39.99999999999987210, 41.69427246844643520 ) ) ;
#7035 = CARTESIAN_POINT ( 'NONE',  ( -56.48582580120559271, 2.158176344243877536E-14, -9.153146818113587102 ) ) ;
#7036 = EDGE_CURVE ( 'NONE', #6050, #4035, #20315, .T. ) ;
#7037 =( BOUNDED_SURFACE ( )  B_SPLINE_SURFACE ( 3, 3, ( 
 ( #3958, #1959, #10065, #26319, #24313, #2091, #8061, #6079, #18301, #16313, #355, #24437, #6205, #4229, #12318, #2223, #8325, #5013, #10733, #11120, #16846, #622, #13118, #21239, #6728, #757, #19105, #24709, #889, #23237 ),
 ( #1014, #3014, #15102, #18708, #4882, #6591, #12987, #14579, #12586, #14976, #20715, #2756, #23110, #20844, #2619, #19234, #18844, #20975, #8728, #14713, #25109, #24979, #6987, #16578, #12857, #4751, #14840, #22973, #10859, #18978 ),
 ( #8861, #6858, #16973, #4484, #21109, #4620, #6464, #22708, #2888, #2481, #10593, #10996, #22845, #491, #8998, #24840, #8598, #16708, #12716, #17102, #25235, #19741, #21873, #7122, #9501, #3138, #3261, #13364, #15608, #7243 ),
 ( #21614, #15482, #15232, #25878, #13493, #19358, #11240, #3519, #17607, #7497, #5641, #11365, #17228, #19483, #11619, #7622, #1148, #15737, #9252, #3388, #17358, #9635, #25494, #15364, #23363, #5513, #1530, #23864, #1269, #17737 ),
 ( #11486, #23488, #25368, #13747, #25749, #19877, #3651, #5388, #5262, #5140, #23609, #21487, #9373, #13246, #21370, #17482, #25624, #11758, #9117, #7371, #23732, #19614, #1400, #13616, #21744, #26150, #14021, #26290, #16013, #24409 ),
 ( #6049, #11891, #3788, #22422, #10169, #59, #24548, #22150, #9768, #12028, #4198, #185, #20011, #18005, #16148, #14420, #20419, #7757, #7894, #26019, #18142, #15868, #24139, #13884, #8168, #16419, #8292, #12291, #5777, #17869 ),
 ( #24280, #2063, #20148, #20284, #14154, #5913, #6302, #22019, #3930, #1927, #22550, #23996, #2196, #10305, #1796, #9900, #10033, #4331, #18410, #8029, #22286, #4060, #12162, #18272, #16281, #14286, #6175, #12421, #1659, #4990 ) ),
 .UNSPECIFIED., .T., .F., .F. ) 
 B_SPLINE_SURFACE_WITH_KNOTS ( ( 4, 3, 4 ),
 ( 4, 2, 2, 2, 2, 2, 2, 2, 2, 2, 2, 2, 2, 2, 4 ),
 ( 0.000000000000000000, 0.5000000000000000000, 1.000000000000000000 ),
 ( 0.000000000000000000, 0.1357259735107005372, 0.1651108541090157700, 0.1944957347073310028, 0.3598804999793158710, 0.3867117631979620773, 0.4135430264166082281, 0.5789277916885930964, 0.6062785021374117456, 0.6336292125862302838, 0.8508620842112317728, 0.8814014469398914198, 0.9119408096685510667, 0.9559704048342755334, 1.000000000000000000 ),
 .UNSPECIFIED. ) 
 GEOMETRIC_REPRESENTATION_ITEM ( )  RATIONAL_B_SPLINE_SURFACE ( (
 ( 1.000000000000000000, 1.000000000000000000, 1.000000000000000000, 1.000000000000000000, 1.000000000000000000, 1.000000000000000000, 1.000000000000000000, 1.000000000000000000, 1.000000000000000000, 1.000000000000000000, 1.000000000000000000, 1.000000000000000000, 1.000000000000000000, 1.000000000000000000, 1.000000000000000000, 1.000000000000000000, 1.000000000000000000, 1.000000000000000000, 1.000000000000000000, 1.000000000000000000, 1.000000000000000000, 1.000000000000000000, 1.000000000000000000, 1.000000000000000000, 1.000000000000000000, 1.000000000000000000, 1.000000000000000000, 1.000000000000000000, 1.000000000000000000, 1.000000000000000000),
 ( 0.3333333333333333703, 0.3333333333333333703, 0.3333333333333333703, 0.3333333333333333703, 0.3333333333333333703, 0.3333333333333333703, 0.3333333333333333703, 0.3333333333333333703, 0.3333333333333333703, 0.3333333333333333703, 0.3333333333333333703, 0.3333333333333333703, 0.3333333333333333703, 0.3333333333333333703, 0.3333333333333333703, 0.3333333333333333703, 0.3333333333333333703, 0.3333333333333333703, 0.3333333333333333703, 0.3333333333333333703, 0.3333333333333333703, 0.3333333333333333703, 0.3333333333333333703, 0.3333333333333333703, 0.3333333333333333703, 0.3333333333333333703, 0.3333333333333333703, 0.3333333333333333703, 0.3333333333333333703, 0.3333333333333333703),
 ( 0.3333333333333333703, 0.3333333333333333703, 0.3333333333333333703, 0.3333333333333333703, 0.3333333333333333703, 0.3333333333333333703, 0.3333333333333333703, 0.3333333333333333703, 0.3333333333333333703, 0.3333333333333333703, 0.3333333333333333703, 0.3333333333333333703, 0.3333333333333333703, 0.3333333333333333703, 0.3333333333333333703, 0.3333333333333333703, 0.3333333333333333703, 0.3333333333333333703, 0.3333333333333333703, 0.3333333333333333703, 0.3333333333333333703, 0.3333333333333333703, 0.3333333333333333703, 0.3333333333333333703, 0.3333333333333333703, 0.3333333333333333703, 0.3333333333333333703, 0.3333333333333333703, 0.3333333333333333703, 0.3333333333333333703),
 ( 1.000000000000000000, 1.000000000000000000, 1.000000000000000000, 1.000000000000000000, 1.000000000000000000, 1.000000000000000000, 1.000000000000000000, 1.000000000000000000, 1.000000000000000000, 1.000000000000000000, 1.000000000000000000, 1.000000000000000000, 1.000000000000000000, 1.000000000000000000, 1.000000000000000000, 1.000000000000000000, 1.000000000000000000, 1.000000000000000000, 1.000000000000000000, 1.000000000000000000, 1.000000000000000000, 1.000000000000000000, 1.000000000000000000, 1.000000000000000000, 1.000000000000000000, 1.000000000000000000, 1.000000000000000000, 1.000000000000000000, 1.000000000000000000, 1.000000000000000000),
 ( 0.3333333333333333703, 0.3333333333333333703, 0.3333333333333333703, 0.3333333333333333703, 0.3333333333333333703, 0.3333333333333333703, 0.3333333333333333703, 0.3333333333333333703, 0.3333333333333333703, 0.3333333333333333703, 0.3333333333333333703, 0.3333333333333333703, 0.3333333333333333703, 0.3333333333333333703, 0.3333333333333333703, 0.3333333333333333703, 0.3333333333333333703, 0.3333333333333333703, 0.3333333333333333703, 0.3333333333333333703, 0.3333333333333333703, 0.3333333333333333703, 0.3333333333333333703, 0.3333333333333333703, 0.3333333333333333703, 0.3333333333333333703, 0.3333333333333333703, 0.3333333333333333703, 0.3333333333333333703, 0.3333333333333333703),
 ( 0.3333333333333333703, 0.3333333333333333703, 0.3333333333333333703, 0.3333333333333333703, 0.3333333333333333703, 0.3333333333333333703, 0.3333333333333333703, 0.3333333333333333703, 0.3333333333333333703, 0.3333333333333333703, 0.3333333333333333703, 0.3333333333333333703, 0.3333333333333333703, 0.3333333333333333703, 0.3333333333333333703, 0.3333333333333333703, 0.3333333333333333703, 0.3333333333333333703, 0.3333333333333333703, 0.3333333333333333703, 0.3333333333333333703, 0.3333333333333333703, 0.3333333333333333703, 0.3333333333333333703, 0.3333333333333333703, 0.3333333333333333703, 0.3333333333333333703, 0.3333333333333333703, 0.3333333333333333703, 0.3333333333333333703),
 ( 1.000000000000000000, 1.000000000000000000, 1.000000000000000000, 1.000000000000000000, 1.000000000000000000, 1.000000000000000000, 1.000000000000000000, 1.000000000000000000, 1.000000000000000000, 1.000000000000000000, 1.000000000000000000, 1.000000000000000000, 1.000000000000000000, 1.000000000000000000, 1.000000000000000000, 1.000000000000000000, 1.000000000000000000, 1.000000000000000000, 1.000000000000000000, 1.000000000000000000, 1.000000000000000000, 1.000000000000000000, 1.000000000000000000, 1.000000000000000000, 1.000000000000000000, 1.000000000000000000, 1.000000000000000000, 1.000000000000000000, 1.000000000000000000, 1.000000000000000000) ) ) 
 REPRESENTATION_ITEM ( '' )  SURFACE ( )  );
#7038 = CARTESIAN_POINT ( 'NONE',  ( 22.40986519363265117, 47.15972762675190211, -13.85314893102512990 ) ) ;
#7039 = CARTESIAN_POINT ( 'NONE',  ( -135.8532207217289454, -30.84685318188648750, -40.00000000000002132 ) ) ;
#7041 = CARTESIAN_POINT ( 'NONE',  ( -603.3751967744402691, 35.45693745050460421, 18.53366164513259307 ) ) ;
#7040 = CARTESIAN_POINT ( 'NONE',  ( 22.72189371636289934, -23.48424859981544088, -43.05215026464033201 ) ) ;
#7042 = CARTESIAN_POINT ( 'NONE',  ( 91.82158438592159655, -22.79471317813468900, 40.00000000000002132 ) ) ;
#7044 = CARTESIAN_POINT ( 'NONE',  ( -259.2033419157646676, 6.730120644403521979, -6.730120644403498886 ) ) ;
#7043 = AXIS2_PLACEMENT_3D ( 'NONE', #10046, #7632, #21622 ) ;
#7045 = CARTESIAN_POINT ( 'NONE',  ( 200.0000000000000000, 39.99999999999985079, 20.00000000000052225 ) ) ;
#7046 = CARTESIAN_POINT ( 'NONE',  ( -114.6659165474109727, 11.80608088193438476, -18.60032035377434312 ) ) ;
#7047 = CARTESIAN_POINT ( 'NONE',  ( -259.2033419157646676, -39.99999999999975131, -30.48217210827782608 ) ) ;
#7048 = CARTESIAN_POINT ( 'NONE',  ( 199.0252416244725282, -6.134786337322394090, 19.04345623536530141 ) ) ;
#7049 = CARTESIAN_POINT ( 'NONE',  ( 154.0335631730542332, -28.18627069283355979, -11.67513559369096754 ) ) ;
#7050 = CARTESIAN_POINT ( 'NONE',  ( 4.995406935893283773, 39.06748935135171052, 17.50105314357239195 ) ) ;
#7051 = CARTESIAN_POINT ( 'NONE',  ( 151.7948205124836250, -4.785054706301671068, 4.785054706301645311 ) ) ;
#7052 = EDGE_CURVE ( 'NONE', #5232, #13725, #15854, .T. ) ;
#7053 = ADVANCED_FACE ( 'NONE', ( #19011 ), #25046, .T. ) ;
#7054 = ORIENTED_EDGE ( 'NONE', *, *, #11709, .T. ) ;
#7056 = CARTESIAN_POINT ( 'NONE',  ( 6.615221834200135653, 44.82734842560610389, -24.79576599683312566 ) ) ;
#7055 = CARTESIAN_POINT ( 'NONE',  ( -77.84460141634583863, -7.435777209860166437, -20.59121244913221815 ) ) ;
#7057 = CARTESIAN_POINT ( 'NONE',  ( 57.59792236341147031, 2.435789363418170872, 40.00000000000002132 ) ) ;
#7058 = CARTESIAN_POINT ( 'NONE',  ( -105.3755690713226727, -15.38646221621807619, 15.38646221621768362 ) ) ;
#7059 = CARTESIAN_POINT ( 'NONE',  ( -188.9524464570941689, 47.22058047019630322, -13.86227157644267649 ) ) ;
#7060 = PRODUCT_CONTEXT ( 'NONE', #9846, 'mechanical' ) ;
#7061 = ORIENTED_EDGE ( 'NONE', *, *, #20049, .F. ) ;
#7062 = ORIENTED_EDGE ( 'NONE', *, *, #14093, .F. ) ;
#7063 = CIRCLE ( 'NONE', #17647, 14.99999999999999645 ) ;
#7064 = CARTESIAN_POINT ( 'NONE',  ( -103.9474983244998469, -19.92928099173819589, 8.577167319634416032 ) ) ;
#7065 = CARTESIAN_POINT ( 'NONE',  ( 85.88436334094248537, -22.72801779304886338, -10.32541289898071035 ) ) ;
#7066 = ORIENTED_EDGE ( 'NONE', *, *, #19964, .T. ) ;
#7067 = ORIENTED_EDGE ( 'NONE', *, *, #9474, .T. ) ;
#7068 = CARTESIAN_POINT ( 'NONE',  ( 199.9999999999996589, -3.408648353384132079, 18.70401797595889448 ) ) ;
#7069 = DIRECTION ( 'NONE',  ( 0.9352143328346382845, 0.3271292286583122322, -0.1355013631594907397 ) ) ;
#7070 = VECTOR ( 'NONE', #13004, 1000.000000000000000 ) ;
#7071 = CARTESIAN_POINT ( 'NONE',  ( 14.38125909742181463, 10.73282306405862485, 67.30136555898259587 ) ) ;
#7072 = DIRECTION ( 'NONE',  ( 0.000000000000000000, 0.000000000000000000, -1.000000000000000000 ) ) ;
#7073 = CARTESIAN_POINT ( 'NONE',  ( -198.0356074513804572, 39.99999999999979394, 55.37879056874835726 ) ) ;
#7074 = CARTESIAN_POINT ( 'NONE',  ( -199.9999999999999432, -44.86667451853065813, 23.83166235904703356 ) ) ;
#7075 = CARTESIAN_POINT ( 'NONE',  ( 98.29820294267490510, 4.808046699556526995E-12, 20.00000000000513722 ) ) ;
#7076 = CARTESIAN_POINT ( 'NONE',  ( -56.48582580120558561, -40.00000000000012790, 9.153146818113166105 ) ) ;
#7077 = CARTESIAN_POINT ( 'NONE',  ( 14.38125909742181818, 5.830552384690105017E-13, -55.17850393972636880 ) ) ;
#7078 = CARTESIAN_POINT ( 'NONE',  ( -199.9999999999998010, 49.28189405767604114, -14.17215463606931181 ) ) ;
#7079 = CIRCLE ( 'NONE', #15544, 15.00000000000000178 ) ;
#7080 = CARTESIAN_POINT ( 'NONE',  ( -238.4067589809705794, -28.96627169325313389, -27.60227080167074831 ) ) ;
#7081 = CARTESIAN_POINT ( 'NONE',  ( -56.48582580120559271, 2.158176344243877536E-14, -9.153146818113587102 ) ) ;
#7082 = LINE ( 'NONE', #11324, #18554 ) ;
#7083 = FACE_OUTER_BOUND ( 'NONE', #2951, .T. ) ;
#7084 = CARTESIAN_POINT ( 'NONE',  ( -190.6721449140024163, -47.76494005424141420, 13.94344083317857574 ) ) ;
#7085 = CARTESIAN_POINT ( 'NONE',  ( 163.1118516004056573, 19.27778845538780317, -19.27778845538757224 ) ) ;
#7086 = CARTESIAN_POINT ( 'NONE',  ( -87.12812962369609693, -14.21201470106591991, 16.13326835690859440 ) ) ;
#7087 = CARTESIAN_POINT ( 'NONE',  ( -213.1075012329537230, -37.98287015391257881, 18.58567234101111509 ) ) ;
#7088 = CARTESIAN_POINT ( 'NONE',  ( -658.1427801728231088, 42.08087261121841038, -15.95318208560120610 ) ) ;
#7089 = CARTESIAN_POINT ( 'NONE',  ( 190.0000000000000000, 61.50000000000009948, 66.50000000000005684 ) ) ;
#7090 = VERTEX_POINT ( 'NONE', #21269 ) ;
#7091 = CARTESIAN_POINT ( 'NONE',  ( 192.4448373802101173, 14.14213562370261279, 42.42640687122091236 ) ) ;
#7092 = DIRECTION ( 'NONE',  ( -1.000000000000000000, 1.836970198721030181E-16, 0.000000000000000000 ) ) ;
#7093 = VECTOR ( 'NONE', #2667, 1000.000000000000000 ) ;
#7094 = CARTESIAN_POINT ( 'NONE',  ( -295.0000000000000568, -4.857225732735059864E-14, 0.000000000000000000 ) ) ;
#7095 = VERTEX_POINT ( 'NONE', #13023 ) ;
#7096 = CARTESIAN_POINT ( 'NONE',  ( 163.1118516004056573, 1.658263919738574066E-13, -12.73709011382475254 ) ) ;
#7097 = CARTESIAN_POINT ( 'NONE',  ( 199.0186487660832029, -17.30925014347549862, -10.04346281267784669 ) ) ;
#7098 = CARTESIAN_POINT ( 'NONE',  ( -199.9999999999998863, -10.02640517461913738, -53.44529986889384077 ) ) ;
#7099 = B_SPLINE_CURVE_WITH_KNOTS ( 'NONE', 3,
 ( #21313, #25955, #3205, #13191, #11432, #5208 ),
 .UNSPECIFIED., .F., .F.,
 ( 4, 2, 4 ),
 ( -6.000000006192509110E-08, 0.03937727993095045675, 0.07875461986190096519 ),
 .UNSPECIFIED. ) ;
#7100 = ORIENTED_EDGE ( 'NONE', *, *, #7510, .F. ) ;
#7101 = ORIENTED_EDGE ( 'NONE', *, *, #7370, .T. ) ;
#7102 = CARTESIAN_POINT ( 'NONE',  ( -105.3755690713226727, 18.24025645688350750, 2.449293598294708485E-15 ) ) ;
#7103 = CARTESIAN_POINT ( 'NONE',  ( -102.4294859496614265, -20.29697089065278703, -8.407280618127234817 ) ) ;
#7104 = CIRCLE ( 'NONE', #8369, 19.53474504356807273 ) ;
#7105 = CARTESIAN_POINT ( 'NONE',  ( -77.78673448795234435, -9.959188558496027355, 19.58653132801459762 ) ) ;
#7106 = CARTESIAN_POINT ( 'NONE',  ( -198.0356074513804572, -40.00000000000011369, 15.37879056873056527 ) ) ;
#7107 = CARTESIAN_POINT ( 'NONE',  ( 199.9999999999999432, -9.907006709245502307, -16.21817530592209522 ) ) ;
#7108 = CARTESIAN_POINT ( 'NONE',  ( -82.28158588894086733, 9.172127817915399106, 18.01698387549497937 ) ) ;
#7109 = CARTESIAN_POINT ( 'NONE',  ( -24.51100708723331323, -15.48921386291974400, -37.39427017791097541 ) ) ;
#7110 = CARTESIAN_POINT ( 'NONE',  ( 146.6084372240433993, 24.48358557860307272, 24.48358557860347418 ) ) ;
#7111 = DIRECTION ( 'NONE',  ( 0.000000000000000000, -0.9767746502210202797, 0.2142691827715867137 ) ) ;
#7112 = CARTESIAN_POINT ( 'NONE',  ( 57.59792236341149163, -39.99999999999961631, -37.56421063658228832 ) ) ;
#7113 = CARTESIAN_POINT ( 'NONE',  ( -56.48582580120559271, 6.472252184284121412, 6.472252184284244869 ) ) ;
#7114 = CARTESIAN_POINT ( 'NONE',  ( -86.96347745069645896, 21.75974354311648895, -40.00000000000002132 ) ) ;
#7115 = CARTESIAN_POINT ( 'NONE',  ( 0.2972598230770100991, -38.42060263243686791, 38.42060263243645579 ) ) ;
#7116 = CARTESIAN_POINT ( 'NONE',  ( 19.06497207195980792, -14.19242893257839988, -40.00000000000002132 ) ) ;
#7117 = ADVANCED_FACE ( 'NONE', ( #21143 ), #11025, .F. ) ;
#7119 = CARTESIAN_POINT ( 'NONE',  ( -213.1075012329537230, 39.99999999999992895, 13.71589010951925935 ) ) ;
#7118 = CARTESIAN_POINT ( 'NONE',  ( 184.8905102610680444, -14.79361573936330565, -41.77492675556016621 ) ) ;
#7120 = CARTESIAN_POINT ( 'NONE',  ( -30.26275506840324425, 1.694272468446254232, -40.00000000000002132 ) ) ;
#7121 = CARTESIAN_POINT ( 'NONE',  ( 136.1360204305621551, -53.05693388239313890, 3.511608612530593199 ) ) ;
#7122 = CARTESIAN_POINT ( 'NONE',  ( 146.6084372240433709, 5.374981219216996564, 40.00000000000002132 ) ) ;
#7123 = ORIENTED_EDGE ( 'NONE', *, *, #21362, .F. ) ;
#7124 = CARTESIAN_POINT ( 'NONE',  ( -3.993758944537062483, -43.01863922058820577, 23.45926997169917172 ) ) ;
#7125 = CARTESIAN_POINT ( 'NONE',  ( 91.82158438592158234, 22.79471317813472098, 2.449293598294708485E-15 ) ) ;
#7126 = CARTESIAN_POINT ( 'NONE',  ( 23.37394308801977871, 23.33966569535068203, 42.85717664514594816 ) ) ;
#7127 = CARTESIAN_POINT ( 'NONE',  ( -280.0000000000000568, -14.14213562373108601, 42.42640687119285303 ) ) ;
#7128 = FACE_OUTER_BOUND ( 'NONE', #19944, .T. ) ;
#7129 = CARTESIAN_POINT ( 'NONE',  ( -77.84359416767949824, 20.59644767746334892, -7.424842266730552254 ) ) ;
#7130 = CARTESIAN_POINT ( 'NONE',  ( -3.903133374378768838, -13.83543723415285598, -47.03983734341025524 ) ) ;
#7131 = CARTESIAN_POINT ( 'NONE',  ( 200.0000000000000568, 7.542793502284206753, 17.44923311141863920 ) ) ;
#7132 = CARTESIAN_POINT ( 'NONE',  ( -648.7286587598725873, 34.24530595729361693, -20.67420341552261931 ) ) ;
#7133 = CARTESIAN_POINT ( 'NONE',  ( -77.70150415251713127, 5.510650003026252186, -21.34766967565243689 ) ) ;
#7134 = CARTESIAN_POINT ( 'NONE',  ( 163.1118516004056573, -19.27778845538787422, 19.27778845538743724 ) ) ;
#7135 = CARTESIAN_POINT ( 'NONE',  ( -105.3755690713226727, 15.38646221621771737, 15.38646221621800514 ) ) ;
#7136 = CARTESIAN_POINT ( 'NONE',  ( -30.26275506840325136, 27.08623969584573388, 29.48230279907808793 ) ) ;
#7137 = CARTESIAN_POINT ( 'NONE',  ( 163.1118516004056573, -19.27778845538787422, 19.27778845538743724 ) ) ;
#7138 = CARTESIAN_POINT ( 'NONE',  ( 170.2234770963711128, 17.36149277826980253, 17.36149277827007253 ) ) ;
#7140 = CARTESIAN_POINT ( 'NONE',  ( -162.0762913951020892, 1.198031840456041497, -57.76657433537918251 ) ) ;
#7139 = CARTESIAN_POINT ( 'NONE',  ( -192.9588430854689989, -10.23066800230742501, -10.23066800230756712 ) ) ;
#7141 = CARTESIAN_POINT ( 'NONE',  ( 151.7948205124836534, 33.06932595376333239, 23.49921654116065284 ) ) ;
#7142 = CARTESIAN_POINT ( 'NONE',  ( -208.1127848780265026, 15.00245453012665564, 0.000000000000000000 ) ) ;
#7143 = CARTESIAN_POINT ( 'NONE',  ( 163.1118516004056573, 9.006482792074356425, -47.56205970284957374 ) ) ;
#7144 = CARTESIAN_POINT ( 'NONE',  ( -105.3755690713226727, 5.661656051307470077E-14, -21.75974354311649961 ) ) ;
#7145 = CARTESIAN_POINT ( 'NONE',  ( -280.0000000000000568, -14.14213562373137556, 42.42640687119276066 ) ) ;
#7146 = CARTESIAN_POINT ( 'NONE',  ( -173.7925187070230493, 38.69492115310539049, -20.60915802527609486 ) ) ;
#7147 = ORIENTED_EDGE ( 'NONE', *, *, #11566, .T. ) ;
#7148 = CARTESIAN_POINT ( 'NONE',  ( -135.8532207217289738, -6.472252184284287502, 50.09629031063965243 ) ) ;
#7149 = CARTESIAN_POINT ( 'NONE',  ( -192.1131137119205050, 24.17676406461165683, 43.98782916596407944 ) ) ;
#7150 = CARTESIAN_POINT ( 'NONE',  ( 22.90311673803691406, 23.44499648834731431, 42.99920082299472313 ) ) ;
#7151 = CARTESIAN_POINT ( 'NONE',  ( -4.151555265633191105, -42.97219445042051689, -23.42746911247791886 ) ) ;
#7152 = ORIENTED_EDGE ( 'NONE', *, *, #15011, .T. ) ;
#7153 = CARTESIAN_POINT ( 'NONE',  ( -83.21262154144253032, -13.72187187061453706, -33.12752917118435647 ) ) ;
#7154 = CARTESIAN_POINT ( 'NONE',  ( 199.9999999999999147, -3.403913688674531812, -18.69557029314349705 ) ) ;
#7155 = CARTESIAN_POINT ( 'NONE',  ( 23.30336656375605742, -13.80490921643078117, 46.83484695576456147 ) ) ;
#7156 = CONICAL_SURFACE ( 'NONE', #22042, 39.99999999999997158, 0.4944367829892074018 ) ;
#7157 = CARTESIAN_POINT ( 'NONE',  ( 37.37129771749314244, 12.75330473306422618, -41.71823991406499488 ) ) ;
#7158 = CARTESIAN_POINT ( 'NONE',  ( 199.0189287881835583, 9.564175521352543896, 17.56735958655279362 ) ) ;
#7159 = CARTESIAN_POINT ( 'NONE',  ( 127.8236149080042310, -28.75948073575762720, 11.91256696755838362 ) ) ;
#7160 = CARTESIAN_POINT ( 'NONE',  ( -56.48582580120559271, 2.158176344243877536E-14, -9.153146818113587102 ) ) ;
#7161 = DIRECTION ( 'NONE',  ( 0.2259624731721235902, 0.000000000000000000, -0.9741360072997697905 ) ) ;
#7162 = FACE_OUTER_BOUND ( 'NONE', #19770, .T. ) ;
#7163 = CARTESIAN_POINT ( 'NONE',  ( 170.2234770963711128, 24.55285855007190676, -40.00000000000002132 ) ) ;
#7165 = CARTESIAN_POINT ( 'NONE',  ( -601.1835555497099222, 36.94693614929742154, 15.42485920190372717 ) ) ;
#7164 = CARTESIAN_POINT ( 'NONE',  ( 37.15749683985377061, -20.52531616267859604, -38.58455518502878334 ) ) ;
#7166 = CARTESIAN_POINT ( 'NONE',  ( -238.4067589809705794, -0.9644942799826262680, 0.000000000000000000 ) ) ;
#7167 = CARTESIAN_POINT ( 'NONE',  ( -86.96347745069644475, 15.38646221621793586, -15.38646221621778842 ) ) ;
#7168 = CARTESIAN_POINT ( 'NONE',  ( 19.06497207195980792, 40.00000000000059686, -54.19242893257802507 ) ) ;
#7169 = CARTESIAN_POINT ( 'NONE',  ( -86.96347745069643054, -40.00000000000026290, 21.75974354311608749 ) ) ;
#7170 = CARTESIAN_POINT ( 'NONE',  ( 151.0849710023778414, -29.07003783291312971, -12.04120392909159776 ) ) ;
#7171 = CARTESIAN_POINT ( 'NONE',  ( -86.96347745069644475, -15.38646221621807442, 15.38646221621768184 ) ) ;
#7172 = VERTEX_POINT ( 'NONE', #11150 ) ;
#7174 = CARTESIAN_POINT ( 'NONE',  ( -2.557884977170212792, 47.52441970259129533, -13.90734923103464560 ) ) ;
#7173 = CARTESIAN_POINT ( 'NONE',  ( -77.55625318716882077, 0.6712688186143358493, -22.13218714683804933 ) ) ;
#7175 = CARTESIAN_POINT ( 'NONE',  ( -192.9588430854690273, -14.46834944099973264, 40.00000000000002132 ) ) ;
#7176 = FILL_AREA_STYLE ('',( #19292 ) ) ;
#7177 = CARTESIAN_POINT ( 'NONE',  ( -114.5520593196434618, 6.810303045868788097, -20.89066532546352306 ) ) ;
#7178 = CARTESIAN_POINT ( 'NONE',  ( 0.000000000000000000, 0.000000000000000000, 0.000000000000000000 ) ) ;
#7179 = EDGE_LOOP ( 'NONE', ( #23041, #11086, #5200, #5080 ) ) ;
#7180 = VERTEX_POINT ( 'NONE', #9148 ) ;
#7181 = CARTESIAN_POINT ( 'NONE',  ( 57.59792236341147031, 1.722363176415065089, -1.722363176415036445 ) ) ;
#7182 = CARTESIAN_POINT ( 'NONE',  ( 156.5537079553355113, 11.28159757857233814, -27.23618587942430480 ) ) ;
#7183 = AXIS2_PLACEMENT_3D ( 'NONE', #15307, #11315, #19555 ) ;
#7184 = CARTESIAN_POINT ( 'NONE',  ( -196.0240759113457045, 44.60678620512916837, -24.63338926175146071 ) ) ;
#7185 = EDGE_CURVE ( 'NONE', #20651, #23802, #19910, .T. ) ;
#7186 = VERTEX_POINT ( 'NONE', #11790 ) ;
#7187 = CARTESIAN_POINT ( 'NONE',  ( 199.9999999999999716, -11.58333327279321701, 15.07704058621049548 ) ) ;
#7188 = CARTESIAN_POINT ( 'NONE',  ( -193.0908541284701982, 14.03723495791108000, 48.38978395451673720 ) ) ;
#7189 = EDGE_CURVE ( 'NONE', #24779, #10794, #1694, .T. ) ;
#7190 = CARTESIAN_POINT ( 'NONE',  ( -280.0000000000000568, 42.42640687119285303, -14.14213562373088351 ) ) ;
#7191 = CARTESIAN_POINT ( 'NONE',  ( -105.3174555396234240, -5.405828096113452830, -20.76745762185852939 ) ) ;
#7192 = CARTESIAN_POINT ( 'NONE',  ( -56.48582580120559271, 2.158176344243877536E-14, -9.153146818113587102 ) ) ;
#7193 = CARTESIAN_POINT ( 'NONE',  ( -190.1935349183499682, -23.83022391594521139, 43.51927535257657098 ) ) ;
#7194 = ADVANCED_FACE ( 'NONE', ( #17636 ), #9799, .F. ) ;
#7195 = EDGE_CURVE ( 'NONE', #11726, #7299, #13015, .T. ) ;
#7196 = DIRECTION ( 'NONE',  ( -1.000000000000000000, -1.836970198721030181E-16, -2.465190328815661892E-32 ) ) ;
#7197 = CARTESIAN_POINT ( 'NONE',  ( -259.2033419157646676, -39.99999999999975131, -30.48217210827782608 ) ) ;
#7198 = CARTESIAN_POINT ( 'NONE',  ( 136.1360204305621551, 40.00000000000009948, -4.966164525586641787 ) ) ;
#7199 = CARTESIAN_POINT ( 'NONE',  ( -110.0737093975828316, -17.41451009903333613, 10.28294049095705986 ) ) ;
#7200 = CARTESIAN_POINT ( 'NONE',  ( 57.59792236341147031, -26.56190807104670171, -30.00663442387710234 ) ) ;
#7201 = CARTESIAN_POINT ( 'NONE',  ( 200.0000000000000000, 40.00000000000012790, -19.99999999999996092 ) ) ;
#7202 = CARTESIAN_POINT ( 'NONE',  ( 4.995406935893293543, -10.78321810389005364, 10.78321810388994173 ) ) ;
#7203 = CARTESIAN_POINT ( 'NONE',  ( -86.86493150571121191, -19.77569912839188149, -7.943527260495856446 ) ) ;
#7204 = CIRCLE ( 'NONE', #1686, 31.79780246617542616 ) ;
#7205 = CARTESIAN_POINT ( 'NONE',  ( -77.56334768864763873, 14.65129183226247278, -16.59360462361560451 ) ) ;
#7206 = CARTESIAN_POINT ( 'NONE',  ( 163.1118516004056573, 47.56205970284957374, 9.006482792074494981 ) ) ;
#7207 = CARTESIAN_POINT ( 'NONE',  ( -77.55461540593363168, 22.14110896975470411, -1.281724172690315244 ) ) ;
#7208 = CARTESIAN_POINT ( 'NONE',  ( -91.56559293963834989, 12.25131212657480440, 12.25131212657486834 ) ) ;
#7209 = CARTESIAN_POINT ( 'NONE',  ( 130.8568914410475088, -32.49135343045495006, 24.07718906446878648 ) ) ;
#7210 = CARTESIAN_POINT ( 'NONE',  ( -187.3037411062501576, -23.25513534570995944, -42.71163782368778783 ) ) ;
#7211 = DIRECTION ( 'NONE',  ( 0.000000000000000000, -1.000000000000000000, 0.000000000000000000 ) ) ;
#7212 = ORIENTED_EDGE ( 'NONE', *, *, #2001, .T. ) ;
#7213 = CARTESIAN_POINT ( 'NONE',  ( 0.2972598230770011618, 10.13633138497555919, -66.70487387989845729 ) ) ;
#7214 = DIRECTION ( 'NONE',  ( -0.000000000000000000, 1.000000000000000000, -0.000000000000000000 ) ) ;
#7215 = CARTESIAN_POINT ( 'NONE',  ( -190.0000000000000000, -52.49999999999970868, 82.49999999999998579 ) ) ;
#7216 = ORIENTED_EDGE ( 'NONE', *, *, #12400, .F. ) ;
#7217 = CARTESIAN_POINT ( 'NONE',  ( -100.7734535825088358, -2.560096224687585342E-13, 22.67402823373191723 ) ) ;
#7218 = CARTESIAN_POINT ( 'NONE',  ( 199.0252574105521717, -19.02124966810586315, 6.202843364552198757 ) ) ;
#7219 = CARTESIAN_POINT ( 'NONE',  ( -1.821043593238315328, -43.61003463695182347, 23.89737153267518721 ) ) ;
#7220 = VERTEX_POINT ( 'NONE', #13651 ) ;
#7221 = EDGE_LOOP ( 'NONE', ( #14771, #17843 ) ) ;
#7222 = CIRCLE ( 'NONE', #14018, 5.000000000000004441 ) ;
#7223 = CARTESIAN_POINT ( 'NONE',  ( -238.4067589809705794, -0.6820004457913680929, 0.6820004457913170226 ) ) ;
#7224 = CARTESIAN_POINT ( 'NONE',  ( 146.6084372240433993, 5.715592784339989804E-15, 5.374981219216972583 ) ) ;
#7225 = CARTESIAN_POINT ( 'NONE',  ( -99.31267923331543557, -20.62886818715002235, -8.544756979596986213 ) ) ;
#7226 = CIRCLE ( 'NONE', #17824, 31.79780246617542616 ) ;
#7227 = CARTESIAN_POINT ( 'NONE',  ( 170.0000000000000000, 3.122849337825751958E-14, 0.000000000000000000 ) ) ;
#7228 = CARTESIAN_POINT ( 'NONE',  ( 19.06497207195981147, -4.605042221739098431E-14, 14.19242893257840521 ) ) ;
#7229 = CARTESIAN_POINT ( 'NONE',  ( 199.9999999999999716, -18.76480772196043034, -3.095184993347289026 ) ) ;
#7230 = CARTESIAN_POINT ( 'NONE',  ( -87.13361725334107177, 14.23662800447680610, 16.15936842096636283 ) ) ;
#7231 = CARTESIAN_POINT ( 'NONE',  ( 14.38125909742180752, 10.73282306404735387, -10.73282306404708919 ) ) ;
#7232 = CARTESIAN_POINT ( 'NONE',  ( 14.38125909742181996, -10.73282306405815234, -67.30136555898266693 ) ) ;
#7233 = CARTESIAN_POINT ( 'NONE',  ( 200.0000000000000000, -71.50000000000002842, 66.50000000000005684 ) ) ;
#7234 = CARTESIAN_POINT ( 'NONE',  ( 0.2972598230770030492, 5.716321584140269555E-13, -54.33493731733936016 ) ) ;
#7235 = CARTESIAN_POINT ( 'NONE',  ( -105.3220005116013880, -20.73876282934127246, -5.373930277613494511 ) ) ;
#7236 = CARTESIAN_POINT ( 'NONE',  ( -91.56559293963836410, 22.67402823373190301, -40.00000000000002132 ) ) ;
#7237 = CARTESIAN_POINT ( 'NONE',  ( -238.4067589809705794, 27.60227080167040370, 28.96627169325338613 ) ) ;
#7238 = CARTESIAN_POINT ( 'NONE',  ( 91.82158438592156813, 17.20528682183302038, -40.00000000000002132 ) ) ;
#7240 = CARTESIAN_POINT ( 'NONE',  ( 184.8905102610680444, 1.070102760522089011E-13, -20.92133201514444352 ) ) ;
#7239 = CARTESIAN_POINT ( 'NONE',  ( 12.01361959687203296, -44.88892880200806701, -24.84115733209536714 ) ) ;
#7241 = CARTESIAN_POINT ( 'NONE',  ( -162.0762913951020892, -1.202636532414034422E-14, -1.694272876828323948 ) ) ;
#7242 = CARTESIAN_POINT ( 'NONE',  ( -208.1127848780265026, 38.89260858015724409, 38.89260858015741462 ) ) ;
#7243 = CARTESIAN_POINT ( 'NONE',  ( 200.0000000000000000, 19.99999999999995737, 40.00000000000002132 ) ) ;
#7244 = ORIENTED_EDGE ( 'NONE', *, *, #17579, .F. ) ;
#7245 = CARTESIAN_POINT ( 'NONE',  ( 23.17367289775000216, -46.88342923877002022, 13.81211338457517535 ) ) ;
#7246 = CARTESIAN_POINT ( 'NONE',  ( -87.08883615166492120, -12.58652615577264022, 17.39726528837622865 ) ) ;
#7247 = CARTESIAN_POINT ( 'NONE',  ( 151.7948205124836534, -23.49921654116027980, 33.06932595376354556 ) ) ;
#7248 = CARTESIAN_POINT ( 'NONE',  ( 91.82158438592158234, 7.693928927950222250E-14, -17.20528682183300262 ) ) ;
#7249 = CARTESIAN_POINT ( 'NONE',  ( -82.28657550317936398, 19.11315898605473862, 6.589961070193250947 ) ) ;
#7250 = AXIS2_PLACEMENT_3D ( 'NONE', #15236, #21492, #13123 ) ;
#7251 = AXIS2_PLACEMENT_3D ( 'NONE', #1746, #13970, #17957 ) ;
#7252 = CIRCLE ( 'NONE', #23010, 15.00000000000000178 ) ;
#7253 = CARTESIAN_POINT ( 'NONE',  ( -7.297127544326129645, 22.81351773422571583, -42.04314499753679968 ) ) ;
#7254 = CARTESIAN_POINT ( 'NONE',  ( 199.9999999999996305, -4.934527571401590151, 18.35877764772902410 ) ) ;
#7255 = EDGE_CURVE ( 'NONE', #12861, #24474, #19694, .T. ) ;
#7256 = CARTESIAN_POINT ( 'NONE',  ( -655.8738625874835861, 39.17324258975333606, -8.150688919272367272 ) ) ;
#7257 = CARTESIAN_POINT ( 'NONE',  ( -82.28266731795157796, -6.247331033611341233, -19.19528918669051265 ) ) ;
#7258 = CARTESIAN_POINT ( 'NONE',  ( 151.7948205124836534, 4.785054706297857230, 51.78348778862544322 ) ) ;
#7259 = CARTESIAN_POINT ( 'NONE',  ( -259.2033419157646676, -21.55415060305824326, -21.55415060305857367 ) ) ;
#7260 = CARTESIAN_POINT ( 'NONE',  ( -100.7734535825088500, 44.31723036834890905, 12.25131212657507795 ) ) ;
#7261 = CARTESIAN_POINT ( 'NONE',  ( 180.0000000000000284, -135.7889608577475258, 82.50000000000001421 ) ) ;
#7262 = CARTESIAN_POINT ( 'NONE',  ( -91.56559293963834989, -12.25131212657475466, -12.25131212657495361 ) ) ;
#7264 = CARTESIAN_POINT ( 'NONE',  ( 184.8905102610680444, -14.79361573936330565, -41.77492675556016621 ) ) ;
#7263 = CARTESIAN_POINT ( 'NONE',  ( -238.4067589809705794, -28.96627169325303797, -28.96627169325349627 ) ) ;
#7265 = CARTESIAN_POINT ( 'NONE',  ( 130.8568914410475088, 32.49135343045448820, 24.07718906446946860 ) ) ;
#7266 = CARTESIAN_POINT ( 'NONE',  ( -280.0000000000000568, -20.00000000000006750, -40.00000000000002132 ) ) ;
#7267 = CARTESIAN_POINT ( 'NONE',  ( 200.0000000000000000, 3.673940397442060756E-14, 0.000000000000000000 ) ) ;
#7268 = DIRECTION ( 'NONE',  ( 1.000000000000000000, 0.000000000000000000, 0.000000000000000000 ) ) ;
#7269 = CARTESIAN_POINT ( 'NONE',  ( 146.6084372240433709, -3.800685668859084210, 52.76785682606516303 ) ) ;
#7270 = AXIS2_PLACEMENT_3D ( 'NONE', #3848, #7553, #11952 ) ;
#7271 = CARTESIAN_POINT ( 'NONE',  ( -188.8948201289232998, 43.30398576617499629, -17.93709820916102871 ) ) ;
#7273 = ADVANCED_FACE ( 'NONE', ( #5672 ), #1403, .T. ) ;
#7272 = EDGE_LOOP ( 'NONE', ( #10006, #18636 ) ) ;
#7274 = CARTESIAN_POINT ( 'NONE',  ( -213.1075012329537230, 37.98287015391236565, -18.58567234101138510 ) ) ;
#7275 = CARTESIAN_POINT ( 'NONE',  ( -199.9999999999998579, 24.82633483071252201, 44.86878812508700776 ) ) ;
#7276 = CARTESIAN_POINT ( 'NONE',  ( 160.9163046357249129, -125.7889608577475684, -55.61140153332245006 ) ) ;
#7277 = CYLINDRICAL_SURFACE ( 'NONE', #24286, 30.00000000000000711 ) ;
#7278 = ORIENTED_EDGE ( 'NONE', *, *, #15894, .F. ) ;
#7279 = CARTESIAN_POINT ( 'NONE',  ( -187.7698581930727073, -46.80706826624575712, 13.79076165501089335 ) ) ;
#7280 = CARTESIAN_POINT ( 'NONE',  ( 200.0000000000001990, -15.45587892757197146, -11.06220582312848144 ) ) ;
#7281 = CARTESIAN_POINT ( 'NONE',  ( 83.11963132822124578, -10.90660717645929090, 23.63628489315943781 ) ) ;
#7282 = ADVANCED_FACE ( 'NONE', ( #13749 ), #21876, .F. ) ;
#7283 = CARTESIAN_POINT ( 'NONE',  ( 170.0000000000000853, -9.369682556672300322, 22.62041470344878746 ) ) ;
#7284 = CARTESIAN_POINT ( 'NONE',  ( 199.0053389886216451, 13.17958853561047228, -15.05032186847045672 ) ) ;
#7285 = CIRCLE ( 'NONE', #21330, 14.99999999999999822 ) ;
#7286 = CARTESIAN_POINT ( 'NONE',  ( -102.4068193528161999, -20.17396017424868404, -8.735227608996884996 ) ) ;
#7287 = B_SPLINE_CURVE_WITH_KNOTS ( 'NONE', 3,
 ( #8893, #9279, #7149, #23394, #12889, #7275 ),
 .UNSPECIFIED., .F., .F.,
 ( 4, 2, 4 ),
 ( -5.998616618535840220E-08, 0.005994953700759713192, 0.01198996738768561172 ),
 .UNSPECIFIED. ) ;
#7288 = CARTESIAN_POINT ( 'NONE',  ( 19.06497207195980792, 39.99999999999983658, 54.19242893257857929 ) ) ;
#7289 = DIRECTION ( 'NONE',  ( 0.000000000000000000, 0.000000000000000000, 1.000000000000000000 ) ) ;
#7290 = CARTESIAN_POINT ( 'NONE',  ( -199.9999999999999716, -15.65821854886078057, -47.96425349429453178 ) ) ;
#7291 = CARTESIAN_POINT ( 'NONE',  ( 184.8905102610680444, -19.07866798485555293, -2.449293598294708485E-15 ) ) ;
#7293 = LINE ( 'NONE', #5188, #9592 ) ;
#7292 = CARTESIAN_POINT ( 'NONE',  ( -121.8281150760809339, 10.16552079391129304, -22.46071699682265788 ) ) ;
#7294 = CARTESIAN_POINT ( 'NONE',  ( -86.96347745069645896, 21.75974354311648895, 40.00000000000002132 ) ) ;
#7295 = CARTESIAN_POINT ( 'NONE',  ( -192.9588430854689989, -14.46834944099973086, 0.000000000000000000 ) ) ;
#7296 = CARTESIAN_POINT ( 'NONE',  ( 170.2234770963711128, 39.99999999999980105, 24.55285855007229401 ) ) ;
#7297 = CARTESIAN_POINT ( 'NONE',  ( 136.1360204305621551, -40.00000000000036238, 35.03383547441254109 ) ) ;
#7298 = DIRECTION ( 'NONE',  ( 0.000000000000000000, 0.000000000000000000, 1.000000000000000000 ) ) ;
#7299 = VERTEX_POINT ( 'NONE', #19879 ) ;
#7301 = CARTESIAN_POINT ( 'NONE',  ( -4.439300432586822609, 42.88738538954446256, -23.37136716947834003 ) ) ;
#7300 = CARTESIAN_POINT ( 'NONE',  ( -16.41594856534389990, 39.35878123533669282, -21.03672846690459863 ) ) ;
#7302 = CARTESIAN_POINT ( 'NONE',  ( -105.3755690713226585, -18.24025645688355013, 40.00000000000002132 ) ) ;
#7303 = CARTESIAN_POINT ( 'NONE',  ( -188.2995950289364941, -46.99046209955528042, 13.82811170417144453 ) ) ;
#7304 = CARTESIAN_POINT ( 'NONE',  ( -192.6562840316691734, 44.11756026580140144, -18.27409180090461760 ) ) ;
#7305 = CARTESIAN_POINT ( 'NONE',  ( 0.000000000000000000, 0.000000000000000000, 0.000000000000000000 ) ) ;
#7306 = ORIENTED_EDGE ( 'NONE', *, *, #11113, .T. ) ;
#7307 = ORIENTED_EDGE ( 'NONE', *, *, #23949, .F. ) ;
#7308 = CARTESIAN_POINT ( 'NONE',  ( -210.0000000000000568, 82.50000000000008527, 52.49999999999980105 ) ) ;
#7309 = CARTESIAN_POINT ( 'NONE',  ( 128.5824617753799828, 11.99766463964419749, -28.96492468983268509 ) ) ;
#7310 = CARTESIAN_POINT ( 'NONE',  ( -97.72675010090323156, 8.185591577777252326, -20.89622088363367070 ) ) ;
#7311 = VERTEX_POINT ( 'NONE', #24551 ) ;
#7312 = CARTESIAN_POINT ( 'NONE',  ( 199.9999999999999716, 1.225499021177249404, 18.97167928969624384 ) ) ;
#7313 = CARTESIAN_POINT ( 'NONE',  ( -211.2619052429883482, 9.184850993605148733E-15, 75.00000000000000000 ) ) ;
#7314 = CARTESIAN_POINT ( 'NONE',  ( 57.59792236341147031, 54.84617931850881689, -1.722363176414946073 ) ) ;
#7315 = CARTESIAN_POINT ( 'NONE',  ( -114.4388184736423142, -20.16431396440720292, -8.352332320002245680 ) ) ;
#7316 = CARTESIAN_POINT ( 'NONE',  ( -280.0000000000000000, 1.839446121267387017E-14, -20.00000000000001421 ) ) ;
#7317 = CARTESIAN_POINT ( 'NONE',  ( 210.0000000000000284, 66.50000000000009948, -66.50000000000005684 ) ) ;
#7318 = DIRECTION ( 'NONE',  ( 1.000000000000000000, 1.836970198721030181E-16, -0.000000000000000000 ) ) ;
#7319 = LINE ( 'NONE', #9579, #21198 ) ;
#7320 = CARTESIAN_POINT ( 'NONE',  ( 163.1118516004056573, -39.99999999999986500, -12.73709011382517353 ) ) ;
#7321 = CARTESIAN_POINT ( 'NONE',  ( -259.2033419157646676, 2.741182173978444749E-13, -30.48217210827739621 ) ) ;
#7322 = CARTESIAN_POINT ( 'NONE',  ( -87.07288175661508944, 17.66871184921714644, 12.16928828659077766 ) ) ;
#7323 = CARTESIAN_POINT ( 'NONE',  ( -91.56559293963836410, -12.25131212657462321, -44.31723036834905827 ) ) ;
#7324 = CARTESIAN_POINT ( 'NONE',  ( -83.21262154144250189, -33.12752917118416462, -13.72187187061501668 ) ) ;
#7325 = CARTESIAN_POINT ( 'NONE',  ( 57.59792236341147031, 1.722363176415065089, -1.722363176415036445 ) ) ;
#7326 = CARTESIAN_POINT ( 'NONE',  ( 156.5537079553356534, 27.23618587942429770, 11.28159757857223688 ) ) ;
#7327 = ADVANCED_FACE ( 'NONE', ( #12424 ), #21644, .T. ) ;
#7328 = DIRECTION ( 'NONE',  ( -7.401486830834375884E-15, -0.3656393565658525024, -0.9307566067077415184 ) ) ;
#7329 = CYLINDRICAL_SURFACE ( 'NONE', #13197, 9.999999999999998224 ) ;
#7330 = CARTESIAN_POINT ( 'NONE',  ( -82.27051431267241810, -17.53273480388464023, 9.999544339283986005 ) ) ;
#7331 = CARTESIAN_POINT ( 'NONE',  ( -86.96347745069644475, -15.38646221621796073, 41.18208027870593924 ) ) ;
#7332 = CARTESIAN_POINT ( 'NONE',  ( 151.7948205124836534, -33.06932595376376582, 23.49921654115996006 ) ) ;
#7333 = CARTESIAN_POINT ( 'NONE',  ( -265.6482238768269326, 0.000000000000000000, 0.000000000000000000 ) ) ;
#7334 = CARTESIAN_POINT ( 'NONE',  ( 200.0000000000000000, 61.50000000000009948, 66.50000000000005684 ) ) ;
#7335 = EDGE_LOOP ( 'NONE', ( #7212, #11305 ) ) ;
#7336 = CARTESIAN_POINT ( 'NONE',  ( 57.59792236341147031, 26.56190807104720975, -26.56190807104655249 ) ) ;
#7337 = EDGE_CURVE ( 'NONE', #15141, #18174, #14944, .T. ) ;
#7338 = CARTESIAN_POINT ( 'NONE',  ( 190.0000000000000000, 66.50000000000009948, 66.50000000000005684 ) ) ;
#7339 = DIRECTION ( 'NONE',  ( 0.000000000000000000, 1.000000000000000000, 0.000000000000000000 ) ) ;
#7340 = VERTEX_POINT ( 'NONE', #14877 ) ;
#7341 = CARTESIAN_POINT ( 'NONE',  ( 163.1118516004056573, -2.556006622855449647E-13, 27.26290988616872824 ) ) ;
#7342 = EDGE_CURVE ( 'NONE', #16610, #19577, #21831, .T. ) ;
#7343 = CARTESIAN_POINT ( 'NONE',  ( 199.0199639038170574, -18.47329534536968509, -7.669176827176202416 ) ) ;
#7344 = CARTESIAN_POINT ( 'NONE',  ( -77.90022806219164409, 8.352332316460230999, 20.16431395584620390 ) ) ;
#7345 = ORIENTED_EDGE ( 'NONE', *, *, #18835, .T. ) ;
#7346 = ORIENTED_EDGE ( 'NONE', *, *, #19154, .T. ) ;
#7347 = CARTESIAN_POINT ( 'NONE',  ( -199.0730705748055982, -44.83667434817697028, -18.57195860671723864 ) ) ;
#7348 = CARTESIAN_POINT ( 'NONE',  ( -56.48582580120560692, 40.00000000000004263, -9.153146818113443217 ) ) ;
#7349 = DIRECTION ( 'NONE',  ( 0.000000000000000000, 0.000000000000000000, -1.000000000000000000 ) ) ;
#7350 = CARTESIAN_POINT ( 'NONE',  ( 170.2234770963711128, 10.92277846919216522, -10.92277846919186501 ) ) ;
#7351 = CARTESIAN_POINT ( 'NONE',  ( -208.1127848780264742, -40.00000000000025580, 55.00245453014408525 ) ) ;
#7352 = CARTESIAN_POINT ( 'NONE',  ( 199.9999999999999147, -17.67734251759716457, -6.986728219496066927 ) ) ;
#7353 = FACE_OUTER_BOUND ( 'NONE', #13469, .T. ) ;
#7354 = CARTESIAN_POINT ( 'NONE',  ( -24.88648382749493848, -12.31763033312684286, -39.69105101983515027 ) ) ;
#7355 = B_SPLINE_CURVE_WITH_KNOTS ( 'NONE', 3,
 ( #6454, #12440, #4348, #4474, #20436, #16838 ),
 .UNSPECIFIED., .F., .F.,
 ( 4, 2, 4 ),
 ( 1.631784767670790744E-15, 0.03937685683732423253, 0.07875371367464684136 ),
 .UNSPECIFIED. ) ;
#7356 = CARTESIAN_POINT ( 'NONE',  ( -86.96347745069645896, 43.67073346367988762, -12.89780903124366418 ) ) ;
#7357 = EDGE_CURVE ( 'NONE', #10760, #7340, #11767, .T. ) ;
#7358 = CARTESIAN_POINT ( 'NONE',  ( -86.86493150571118349, -19.60045294882770506, 8.366608963953762412 ) ) ;
#7359 = CARTESIAN_POINT ( 'NONE',  ( 170.2234770963711128, 1.955190573858485757E-13, -15.44714144992816074 ) ) ;
#7360 = CARTESIAN_POINT ( 'NONE',  ( -626.9846540392097722, 75.00000000000000000, 59.99999999999999289 ) ) ;
#7361 = CARTESIAN_POINT ( 'NONE',  ( 200.0000000000000000, -19.99999999999989342, 40.00000000000002132 ) ) ;
#7362 = B_SPLINE_CURVE_WITH_KNOTS ( 'NONE', 3,
 ( #10697, #6823, #10420, #18668, #8961, #20811, #14805, #22807, #851, #24671, #14941, #24805, #455, #14545, #17070, #12414, #2582, #25204, #8695, #18537, #6951, #20540, #16806, #4717, #12822, #2311, #6427, #20944, #22675, #319, #23076, #2722, #4847, #10827, #18942, #722, #15574, #25708, #13578, #17193, #17325, #11331, #19575, #7088, #21705, #25587, #23698, #13458, #17448, #19200, #21452, #15446, #15202, #2976, #23574, #9464, #25331, #1366, #3103, #21204, #19447, #23330, #15699, #5105 ),
 .UNSPECIFIED., .F., .F.,
 ( 4, 2, 2, 2, 2, 2, 2, 2, 2, 2, 2, 2, 2, 2, 2, 2, 2, 2, 2, 2, 2, 2, 2, 2, 2, 2, 2, 2, 2, 2, 2, 4 ),
 ( 0.1150183322533817887, 0.1222062663255236575, 0.1258002333615945989, 0.1293942003976655264, 0.1329881674337364816, 0.1365821344698074091, 0.1437700685419490421, 0.1455670520599845474, 0.1473640355780200806, 0.1509580026140910913, 0.1581459366862331684, 0.1599429202042686182, 0.1617399037223040681, 0.1653338707583749956, 0.1671308542764104454, 0.1689278377944458953, 0.1725218048305168228, 0.1761157718665877225, 0.1779127553846231724, 0.1797097389026586223, 0.1868976729748003107, 0.1886946564928357883, 0.1904916400108712105, 0.1940856070469419992, 0.1976795740830127324, 0.2012735411190835211, 0.2084614751912248487, 0.2120554422272953876, 0.2156494092633658988, 0.2192433762994364654, 0.2228373433355070321, 0.2300252774076481099 ),
 .UNSPECIFIED. ) ;
#7363 = CARTESIAN_POINT ( 'NONE',  ( 184.8905102610680444, -19.07866798485553872, -40.00000000000002132 ) ) ;
#7364 = CARTESIAN_POINT ( 'NONE',  ( -213.1075012329537230, -9.698598906450557777, 9.698598906450415669 ) ) ;
#7365 = CARTESIAN_POINT ( 'NONE',  ( -135.8532207217289738, 9.153146818113548022, -40.00000000000002132 ) ) ;
#7367 = DIRECTION ( 'NONE',  ( 0.9352143328345526863, 0.1355013631511626238, -0.3271292286620064993 ) ) ;
#7366 = CARTESIAN_POINT ( 'NONE',  ( 136.1360204305621266, -24.77266263493151044, 24.77266263493093135 ) ) ;
#7368 = CARTESIAN_POINT ( 'NONE',  ( -30.26275506840324070, 1.218738420030236455E-14, -1.694272468446259783 ) ) ;
#7369 = CARTESIAN_POINT ( 'NONE',  ( 14.38125909742181108, 39.01709431150907648, 39.01709431150921858 ) ) ;
#7370 = EDGE_CURVE ( 'NONE', #2226, #10098, #13650, .T. ) ;
#7371 = CARTESIAN_POINT ( 'NONE',  ( 57.59792236341147031, 37.56421063658187620, -40.00000000000002132 ) ) ;
#7372 = ORIENTED_EDGE ( 'NONE', *, *, #6480, .F. ) ;
#7373 = CARTESIAN_POINT ( 'NONE',  ( 23.49666234703822809, -42.81942870555059244, 23.31470603676244480 ) ) ;
#7374 = CARTESIAN_POINT ( 'NONE',  ( 132.4338126186516718, 12.33615677966314195, 29.78211700502430759 ) ) ;
#7375 = CARTESIAN_POINT ( 'NONE',  ( -56.48582580120559271, 21.81201906317768291, 21.81201906317777173 ) ) ;
#7376 = CARTESIAN_POINT ( 'NONE',  ( -30.26275506840324070, -1.147469862568086380E-14, 1.694272468446259783 ) ) ;
#7377 = CARTESIAN_POINT ( 'NONE',  ( -77.70542728667135179, 21.32786667381274270, -5.408320660863019214 ) ) ;
#7378 = CARTESIAN_POINT ( 'NONE',  ( 0.4289713102705769998, -14.02712011273541037, -48.32239598606157926 ) ) ;
#7379 = CARTESIAN_POINT ( 'NONE',  ( 200.0000000000000000, 2.625635831523228880, 18.82681798050185051 ) ) ;
#7380 = FACE_OUTER_BOUND ( 'NONE', #10896, .T. ) ;
#7381 = CARTESIAN_POINT ( 'NONE',  ( -87.13368444201113050, 0.6697911384492148956, -21.49365365690828256 ) ) ;
#7382 = FACE_OUTER_BOUND ( 'NONE', #22648, .T. ) ;
#7383 = CARTESIAN_POINT ( 'NONE',  ( -135.8532207217289738, -21.81201906317757633, -21.81201906317793515 ) ) ;
#7384 = CARTESIAN_POINT ( 'NONE',  ( 136.1360204305621266, 24.77266263493138965, -24.77266263493110188 ) ) ;
#7385 = DIRECTION ( 'NONE',  ( 0.000000000000000000, 0.000000000000000000, -1.000000000000000000 ) ) ;
#7386 = CARTESIAN_POINT ( 'NONE',  ( 0.2972598230769923355, 18.14793986248751168, -38.42060263243650553 ) ) ;
#7388 = CARTESIAN_POINT ( 'NONE',  ( 136.1360204305621551, -24.77266263493081766, -31.79587985999290112 ) ) ;
#7387 = CARTESIAN_POINT ( 'NONE',  ( -91.56559293963834989, -12.25131212657475466, -12.25131212657495361 ) ) ;
#7389 = CARTESIAN_POINT ( 'NONE',  ( -30.26275506840323715, 29.48230279907829754, -29.48230279907758344 ) ) ;
#7390 = DIRECTION ( 'NONE',  ( -1.000000000000000000, 0.000000000000000000, 0.000000000000000000 ) ) ;
#7391 = DIRECTION ( 'NONE',  ( 1.000000000000000000, 1.836970198721030181E-16, 0.000000000000000000 ) ) ;
#7392 = CARTESIAN_POINT ( 'NONE',  ( 57.59792236341148453, -40.00000000000000000, -2.435789363418300546 ) ) ;
#7393 = CARTESIAN_POINT ( 'NONE',  ( -86.96347745069645896, -12.89780903124443689, 43.67073346367968156 ) ) ;
#7394 = CARTESIAN_POINT ( 'NONE',  ( -280.0000000000000000, 19.99999999999996092, 2.449293598294708485E-15 ) ) ;
#7395 = ORIENTED_EDGE ( 'NONE', *, *, #8830, .T. ) ;
#7396 = CARTESIAN_POINT ( 'NONE',  ( 184.8905102610680444, 41.77492675556005253, -14.79361573936377461 ) ) ;
#7397 = CARTESIAN_POINT ( 'NONE',  ( 62.42050862285469748, 30.90338125512822387, 12.80059963906062315 ) ) ;
#7398 = CARTESIAN_POINT ( 'NONE',  ( 200.0000000000000000, 75.52305771588345351, -68.47933392563552957 ) ) ;
#7399 = CARTESIAN_POINT ( 'NONE',  ( -5.379830816903821145, -42.60994460517692062, -23.18791234549714986 ) ) ;
#7400 = ORIENTED_EDGE ( 'NONE', *, *, #21432, .F. ) ;
#7401 = CARTESIAN_POINT ( 'NONE',  ( -144.1957000274121867, -30.13184844814661645, 12.48102028665973506 ) ) ;
#7402 = B_SPLINE_CURVE_WITH_KNOTS ( 'NONE', 3,
 ( #7868, #24524, #1906, #6282, #14397, #22529 ),
 .UNSPECIFIED., .F., .F.,
 ( 4, 2, 4 ),
 ( -5.998616622604924294E-08, 0.005994953700759752223, 0.01198996738768573142 ),
 .UNSPECIFIED. ) ;
#7403 = CARTESIAN_POINT ( 'NONE',  ( 200.0000000000001421, -10.69674284809226350, -15.70882504007707681 ) ) ;
#7404 = CARTESIAN_POINT ( 'NONE',  ( 60.28378959952933513, -15.72633063269985421, 31.18416451510499954 ) ) ;
#7405 = CARTESIAN_POINT ( 'NONE',  ( 199.0055119247266759, 16.54204028020789252, -11.23294693469441263 ) ) ;
#7406 = EDGE_CURVE ( 'NONE', #24210, #8803, #18472, .T. ) ;
#7407 = CARTESIAN_POINT ( 'NONE',  ( -89.92902785008701017, -20.17328762787301955, -8.734793929541259772 ) ) ;
#7408 = CARTESIAN_POINT ( 'NONE',  ( 170.2234770963711128, 40.00000000000014211, -24.55285855007172913 ) ) ;
#7409 = CARTESIAN_POINT ( 'NONE',  ( 136.1360204305621266, 1.473277640373554421E-13, -35.03383547441296741 ) ) ;
#7410 = CARTESIAN_POINT ( 'NONE',  ( -210.0000000000000284, 69.99999999999998579, 0.000000000000000000 ) ) ;
#7411 = CARTESIAN_POINT ( 'NONE',  ( 163.1118516004056573, -12.73709011382472234, -2.449293598294708485E-15 ) ) ;
#7413 = CARTESIAN_POINT ( 'NONE',  ( 150.0000000000000284, -135.7889608577475258, 82.50000000000001421 ) ) ;
#7412 = CARTESIAN_POINT ( 'NONE',  ( -144.1957134275961323, 12.48102206801882552, -30.13185274904616406 ) ) ;
#7414 = CARTESIAN_POINT ( 'NONE',  ( 151.7948205124836534, -6.767089262349006873, 40.00000000000002132 ) ) ;
#7415 = CARTESIAN_POINT ( 'NONE',  ( -192.9588430854690273, -14.46834944099973264, -40.00000000000002132 ) ) ;
#7416 = CARTESIAN_POINT ( 'NONE',  ( 136.1360204305621266, -35.03383547441293899, 0.000000000000000000 ) ) ;
#7417 = CARTESIAN_POINT ( 'NONE',  ( -162.0762913951021176, 40.00000000000001421, -1.694272876827905394 ) ) ;
#7418 = CARTESIAN_POINT ( 'NONE',  ( 163.1118516004056573, 1.658263919738574066E-13, -12.73709011382475254 ) ) ;
#7419 = CARTESIAN_POINT ( 'NONE',  ( -86.86493150571114086, -19.60045294882784717, -8.366608963953355627 ) ) ;
#7420 = VERTEX_POINT ( 'NONE', #14610 ) ;
#7422 = CARTESIAN_POINT ( 'NONE',  ( 1.925538622597735339, 44.35335385591526602, -24.44644315488994479 ) ) ;
#7421 = CARTESIAN_POINT ( 'NONE',  ( 98.29850319135208281, 8.262390927745583369, -18.22532005587680359 ) ) ;
#7423 = CARTESIAN_POINT ( 'NONE',  ( -208.1127848780264742, -55.00245453010926866, 40.00000000000002132 ) ) ;
#7424 = EDGE_CURVE ( 'NONE', #26265, #19296, #8498, .T. ) ;
#7425 = CARTESIAN_POINT ( 'NONE',  ( -56.48582580120559271, -6.472252184284276844, 6.472252184284108978 ) ) ;
#7426 = CARTESIAN_POINT ( 'NONE',  ( -195.1686598214107846, 48.78512304063578853, -14.09692385499625900 ) ) ;
#7427 = DIRECTION ( 'NONE',  ( 0.000000000000000000, 0.000000000000000000, 1.000000000000000000 ) ) ;
#7428 =( GEOMETRIC_REPRESENTATION_CONTEXT ( 3 ) GLOBAL_UNCERTAINTY_ASSIGNED_CONTEXT ( ( #15650 ) ) GLOBAL_UNIT_ASSIGNED_CONTEXT ( ( #4028, #14250, #22518 ) ) REPRESENTATION_CONTEXT ( 'NONE', 'WORKASPACE' ) );
#7429 = ORIENTED_EDGE ( 'NONE', *, *, #13444, .F. ) ;
#7430 = ORIENTED_EDGE ( 'NONE', *, *, #21493, .T. ) ;
#7431 = CARTESIAN_POINT ( 'NONE',  ( -93.02511667907101867, -20.50052124204851367, 8.946512270084788554 ) ) ;
#7432 = CARTESIAN_POINT ( 'NONE',  ( 155.4809970915716519, 11.45899766888377869, -27.66446758342027934 ) ) ;
#7433 = EDGE_LOOP ( 'NONE', ( #10400, #16251 ) ) ;
#7434 = CARTESIAN_POINT ( 'NONE',  ( -96.93773665438905596, 8.190703376740906094, -20.92028269119429496 ) ) ;
#7435 = ORIENTED_EDGE ( 'NONE', *, *, #19387, .F. ) ;
#7436 = CARTESIAN_POINT ( 'NONE',  ( 200.0000000000002842, -5.234650960127995134, 18.27551028936266775 ) ) ;
#7437 = VECTOR ( 'NONE', #8707, 1000.000000000000000 ) ;
#7438 = CIRCLE ( 'NONE', #15506, 6.000000000000005329 ) ;
#7439 = CARTESIAN_POINT ( 'NONE',  ( -200.0000000000000000, 66.50000000000009948, -66.50000000000005684 ) ) ;
#7440 = CARTESIAN_POINT ( 'NONE',  ( -100.7734535825088358, 12.25131212657480440, 12.25131212657487012 ) ) ;
#7441 = CARTESIAN_POINT ( 'NONE',  ( -200.0000000000000853, 44.88127304973836118, -30.70179486994623375 ) ) ;
#7442 = CARTESIAN_POINT ( 'NONE',  ( 151.7948205124836250, 1.439163438361279259E-13, -33.23291073765553705 ) ) ;
#7443 = CARTESIAN_POINT ( 'NONE',  ( -188.2995950289364657, -23.44932284466040784, 43.00522595870950937 ) ) ;
#7444 = DIRECTION ( 'NONE',  ( 0.000000000000000000, 1.000000000000000000, 0.000000000000000000 ) ) ;
#7445 = CARTESIAN_POINT ( 'NONE',  ( -626.9846540392142060, 105.0000000000000000, 0.000000000000000000 ) ) ;
#7446 = CARTESIAN_POINT ( 'NONE',  ( -198.0356074513804572, 1.247057299367198800E-13, -15.37879056873070560 ) ) ;
#7447 = PRODUCT_DEFINITION_FORMATION_WITH_SPECIFIED_SOURCE ( 'ANY', '', #10401, .NOT_KNOWN. ) ;
#7448 = CARTESIAN_POINT ( 'NONE',  ( -208.1127848780264742, -39.99999999999948841, -55.00245453010965235 ) ) ;
#7449 = CARTESIAN_POINT ( 'NONE',  ( -114.7465989397656756, -17.47221266594894473, 13.54917888340187204 ) ) ;
#7450 = CARTESIAN_POINT ( 'NONE',  ( 136.1360204305621266, 24.77266263493138965, -24.77266263493110188 ) ) ;
#7451 = CARTESIAN_POINT ( 'NONE',  ( -91.56559293963834989, 6.234561990864368500E-14, -22.67402823373191723 ) ) ;
#7452 = CARTESIAN_POINT ( 'NONE',  ( -192.1963514251162621, 24.16258207727632978, 43.96876056339223027 ) ) ;
#7453 = LINE ( 'NONE', #11445, #23211 ) ;
#7454 = CARTESIAN_POINT ( 'NONE',  ( -86.84962968273566730, 19.67999904273991163, 8.151722510992470916 ) ) ;
#7455 = CARTESIAN_POINT ( 'NONE',  ( 151.7948205124836250, 23.49921654116361225, -23.49921654116333514 ) ) ;
#7456 = CARTESIAN_POINT ( 'NONE',  ( -162.0762913951021176, -40.00000000000005684, 1.694272876828184504 ) ) ;
#7457 = CARTESIAN_POINT ( 'NONE',  ( 4.995406935893297096, 10.78321810387837232, 67.35176059880234334 ) ) ;
#7458 = AXIS2_PLACEMENT_3D ( 'NONE', #15240, #11765, #15875 ) ;
#7459 = AXIS2_PLACEMENT_3D ( 'NONE', #16031, #26038, #24156 ) ;
#7460 = CARTESIAN_POINT ( 'NONE',  ( -56.48582580120558561, -21.81201906317755146, -21.81201906317792449 ) ) ;
#7461 = CARTESIAN_POINT ( 'NONE',  ( 116.7964245048382850, -2.716484884814708943E-13, 27.98274000340149925 ) ) ;
#7462 = VERTEX_POINT ( 'NONE', #4391 ) ;
#7463 = CARTESIAN_POINT ( 'NONE',  ( 184.8905102610680444, 41.77492675555983936, 14.79361573936436081 ) ) ;
#7464 = CARTESIAN_POINT ( 'NONE',  ( -678.9461782662789346, 75.00000000000000000, -29.99999999999836220 ) ) ;
#7465 = CARTESIAN_POINT ( 'NONE',  ( -362.0709805440841365, 10.00000000000000000, 0.000000000000000000 ) ) ;
#7466 = ORIENTED_EDGE ( 'NONE', *, *, #20455, .F. ) ;
#7467 = CARTESIAN_POINT ( 'NONE',  ( 4.995406935893297984, -39.99999999999986500, -15.24977328854874870 ) ) ;
#7468 = CARTESIAN_POINT ( 'NONE',  ( 199.0156711280681350, -13.74982657632009264, -14.52405353129264043 ) ) ;
#7469 = CARTESIAN_POINT ( 'NONE',  ( -40.07203023071645021, 16.33025453615710632, 32.10811084141644045 ) ) ;
#7470 = AXIS2_PLACEMENT_3D ( 'NONE', #20459, #901, #6604 ) ;
#7471 = ORIENTED_EDGE ( 'NONE', *, *, #12728, .T. ) ;
#7472 = VERTEX_POINT ( 'NONE', #24609 ) ;
#7473 = CARTESIAN_POINT ( 'NONE',  ( -197.4153392275794658, -49.11379398046383216, -14.14666332908225321 ) ) ;
#7474 = CARTESIAN_POINT ( 'NONE',  ( -86.96347745069645896, 39.99999999999994316, 18.24025645688366737 ) ) ;
#7475 = SURFACE_STYLE_FILL_AREA ( #9748 ) ;
#7476 = CIRCLE ( 'NONE', #1548, 5.000000000000046185 ) ;
#7477 = CARTESIAN_POINT ( 'NONE',  ( -200.0000000000000000, 0.000000000000000000, 0.000000000000000000 ) ) ;
#7478 = CARTESIAN_POINT ( 'NONE',  ( 0.2972598230770030492, -1.921041075453695163E-13, 54.33493731733936016 ) ) ;
#7479 = CARTESIAN_POINT ( 'NONE',  ( 199.9999999999998579, -10.30558286630674658, -15.96802547070553047 ) ) ;
#7480 = CARTESIAN_POINT ( 'NONE',  ( 130.8568914410475372, 1.429239637432775288E-13, -34.05028731879788495 ) ) ;
#7481 = CIRCLE ( 'NONE', #10910, 30.00000000000000000 ) ;
#7482 = SPHERICAL_SURFACE ( 'NONE', #17277, 15.00000000000000000 ) ;
#7483 = CARTESIAN_POINT ( 'NONE',  ( -5.152948516943947510, -13.74948675458091785, -46.60473671797106476 ) ) ;
#7484 = CARTESIAN_POINT ( 'NONE',  ( -162.0762913951020892, -1.198031840315659124, -57.76657433523998009 ) ) ;
#7485 = AXIS2_PLACEMENT_3D ( 'NONE', #24288, #20025, #19885 ) ;
#7486 = CARTESIAN_POINT ( 'NONE',  ( -105.2054292635175585, -21.49321519473986442, -7.030298963786045751E-29 ) ) ;
#7487 = CARTESIAN_POINT ( 'NONE',  ( 136.1360204305621551, -40.00000000000036238, 35.03383547441254109 ) ) ;
#7488 = CARTESIAN_POINT ( 'NONE',  ( 35.93675087557281245, -42.26938917802861084, -12.87543817561850723 ) ) ;
#7489 = CARTESIAN_POINT ( 'NONE',  ( 91.82158438592156813, 17.20528682183302038, 40.00000000000002132 ) ) ;
#7490 = CARTESIAN_POINT ( 'NONE',  ( -56.48582580120558561, -30.84685318188645553, -40.00000000000002132 ) ) ;
#7491 = CARTESIAN_POINT ( 'NONE',  ( 0.2972598230769976091, -10.13633138497479180, 10.13633138497468522 ) ) ;
#7492 = CARTESIAN_POINT ( 'NONE',  ( 170.2234770963711128, 24.55285855007190321, 0.000000000000000000 ) ) ;
#7494 = CARTESIAN_POINT ( 'NONE',  ( 150.0000000000000284, -135.7889608577475258, -82.49999999999998579 ) ) ;
#7493 = CARTESIAN_POINT ( 'NONE',  ( 23.23639021239542046, -42.89921396172177026, -23.37084785298091205 ) ) ;
#7495 = CARTESIAN_POINT ( 'NONE',  ( -56.48582580120559271, -1.062504017861011783E-13, 9.153146818113587102 ) ) ;
#7496 = CARTESIAN_POINT ( 'NONE',  ( 192.4448373802100889, 14.14213562370310662, 14.14213562370312438 ) ) ;
#7497 = CARTESIAN_POINT ( 'NONE',  ( -105.3755690713226727, 18.24025645688350750, 2.449293598294708485E-15 ) ) ;
#7498 = VERTEX_POINT ( 'NONE', #6363 ) ;
#7499 = CARTESIAN_POINT ( 'NONE',  ( 83.06440094974429655, -23.65491511365441113, 10.91839312112026050 ) ) ;
#7500 = CARTESIAN_POINT ( 'NONE',  ( -83.21262154144274348, 13.72187187063241609, 33.12752917117732210 ) ) ;
#7501 = CIRCLE ( 'NONE', #1574, 19.53474504356812602 ) ;
#7502 = EDGE_CURVE ( 'NONE', #16387, #18786, #3823, .T. ) ;
#7503 = CARTESIAN_POINT ( 'NONE',  ( 0.2972598230769907257, 66.70487387989857098, 10.13633138497486641 ) ) ;
#7504 = CARTESIAN_POINT ( 'NONE',  ( 4.995406935893297984, -40.00000000000007816, 15.24977328854818914 ) ) ;
#7505 = CARTESIAN_POINT ( 'NONE',  ( -213.1075012329537230, 37.98287015391211696, 18.58567234101190735 ) ) ;
#7506 = EDGE_CURVE ( 'NONE', #19428, #6493, #322, .T. ) ;
#7507 = CARTESIAN_POINT ( 'NONE',  ( 200.0000000000000000, 19.99999999999996447, -40.00000000000002132 ) ) ;
#7508 = CARTESIAN_POINT ( 'NONE',  ( -163.5815439468644854, -35.61501074489159180, -18.59457101073931540 ) ) ;
#7509 = CARTESIAN_POINT ( 'NONE',  ( 200.0000000000000284, 9.630262036685882876, 16.38694142346205140 ) ) ;
#7510 = EDGE_CURVE ( 'NONE', #287, #6828, #3272, .T. ) ;
#7511 = EDGE_CURVE ( 'NONE', #12221, #2784, #10071, .T. ) ;
#7512 = CARTESIAN_POINT ( 'NONE',  ( 170.0000000000000000, 12.70659020859086574, 21.59613885783099718 ) ) ;
#7513 = CARTESIAN_POINT ( 'NONE',  ( -56.48582580120559982, 21.81201906317729922, 34.75652343174635917 ) ) ;
#7514 = CARTESIAN_POINT ( 'NONE',  ( -198.0356074513804288, -39.15871834505882276, -39.15871834505946936 ) ) ;
#7515 = DIRECTION ( 'NONE',  ( 0.000000000000000000, 1.000000000000000000, 0.000000000000000000 ) ) ;
#7516 = CARTESIAN_POINT ( 'NONE',  ( -82.28162732578149985, 9.169756991572501903, -18.01798805106890811 ) ) ;
#7517 = CARTESIAN_POINT ( 'NONE',  ( 170.2234770963711128, 17.36149277827028925, -39.20704971665377059 ) ) ;
#7519 = CARTESIAN_POINT ( 'NONE',  ( 170.2234770963711128, -45.64576402573167258, -10.92277846919254891 ) ) ;
#7518 = CARTESIAN_POINT ( 'NONE',  ( 4.995406935893300648, -10.78321810387790514, -67.35176059880241439 ) ) ;
#7520 = CARTESIAN_POINT ( 'NONE',  ( 14.38125909742181285, -17.55144818341421598, -39.01709431150935359 ) ) ;
#7521 = CARTESIAN_POINT ( 'NONE',  ( -105.2274517607656463, -13.17594969608524735, 17.01575307706266571 ) ) ;
#7522 = DIRECTION ( 'NONE',  ( -1.000000000000000000, 0.000000000000000000, 0.000000000000000000 ) ) ;
#7523 = CARTESIAN_POINT ( 'NONE',  ( 4.995406935893297984, -40.00000000000007816, 15.24977328854818914 ) ) ;
#7524 = CARTESIAN_POINT ( 'NONE',  ( -100.7734535825088500, 16.03295912088683295, 40.53558337403684675 ) ) ;
#7525 = CARTESIAN_POINT ( 'NONE',  ( 170.2234770963711128, -17.36149277827010096, 17.36149277826970660 ) ) ;
#7526 = CARTESIAN_POINT ( 'NONE',  ( -238.4067589809705794, 40.96449427990177128, 40.00000000000002132 ) ) ;
#7527 = ORIENTED_EDGE ( 'NONE', *, *, #9629, .T. ) ;
#7528 = CARTESIAN_POINT ( 'NONE',  ( 0.2972598230769886718, 38.42060263243669027, -18.14793986248710667 ) ) ;
#7529 = CARTESIAN_POINT ( 'NONE',  ( 24.48536172914053566, 41.83775886953835510, 17.32976714305807775 ) ) ;
#7530 = LINE ( 'NONE', #21776, #14536 ) ;
#7531 = CARTESIAN_POINT ( 'NONE',  ( 98.29820294267335612, -19.49240851343218850, -4.524526698153942483 ) ) ;
#7532 = ORIENTED_EDGE ( 'NONE', *, *, #9614, .F. ) ;
#7533 = CARTESIAN_POINT ( 'NONE',  ( -188.9001212172966291, -43.30535683045341955, 17.93766612257997295 ) ) ;
#7534 = CARTESIAN_POINT ( 'NONE',  ( 199.9999999999998579, -16.14759498898286338, -10.02975912355057453 ) ) ;
#7535 = CARTESIAN_POINT ( 'NONE',  ( 23.13330272892053330, -17.84165608060301622, 43.07356808498551715 ) ) ;
#7536 = CARTESIAN_POINT ( 'NONE',  ( 11.71430589693755131, 24.82930166508055692, -44.87285427231127954 ) ) ;
#7537 = CARTESIAN_POINT ( 'NONE',  ( 199.0054122081438948, 15.86953797770180508, -12.16778084942700211 ) ) ;
#7538 = CARTESIAN_POINT ( 'NONE',  ( -96.93773665438882858, -20.58457565566404313, -9.001171854902130676 ) ) ;
#7539 = CARTESIAN_POINT ( 'NONE',  ( 192.4448373802101173, 39.99999999999998579, 19.99999999996075317 ) ) ;
#7540 = CARTESIAN_POINT ( 'NONE',  ( 170.0000000000000000, -24.95097643316997704, 0.000000000000000000 ) ) ;
#7541 = CARTESIAN_POINT ( 'NONE',  ( -190.0000000000000000, 66.50000000000009948, -66.50000000000005684 ) ) ;
#7542 = CARTESIAN_POINT ( 'NONE',  ( -208.1127848780264742, -15.00245453012673202, 40.00000000000002132 ) ) ;
#7544 = CARTESIAN_POINT ( 'NONE',  ( -605.2086264830600157, 34.26251070455288072, -20.65666574593837268 ) ) ;
#7543 = CARTESIAN_POINT ( 'NONE',  ( 98.29820294267328507, -7.653668647303858208, -18.47759065023126723 ) ) ;
#7545 = DIRECTION ( 'NONE',  ( 1.000000000000000000, -0.000000000000000000, -0.000000000000000000 ) ) ;
#7546 = CARTESIAN_POINT ( 'NONE',  ( -135.8532207217289454, -30.84685318188648750, -40.00000000000002132 ) ) ;
#7547 = CARTESIAN_POINT ( 'NONE',  ( 151.7948205124836534, -33.23291073765550863, 40.00000000000002132 ) ) ;
#7548 = CARTESIAN_POINT ( 'NONE',  ( -213.1075012329537230, 5.259461644596141978E-13, -53.71589010951915100 ) ) ;
#7549 = CARTESIAN_POINT ( 'NONE',  ( 19.06497207195981147, 1.521599808664285085E-13, -14.19242893257840521 ) ) ;
#7550 = CARTESIAN_POINT ( 'NONE',  ( -716.9846540392142060, 82.50000000000008527, -52.49999999999977973 ) ) ;
#7551 = ORIENTED_EDGE ( 'NONE', *, *, #10708, .T. ) ;
#7552 = DIRECTION ( 'NONE',  ( 1.000000000000000000, 0.000000000000000000, 0.000000000000000000 ) ) ;
#7553 = DIRECTION ( 'NONE',  ( -1.000000000000000000, -1.836970198721030181E-16, 0.000000000000000000 ) ) ;
#7554 = SURFACE_SIDE_STYLE ('',( #25807 ) ) ;
#7555 = CARTESIAN_POINT ( 'NONE',  ( -96.94475454968979022, -8.190683501892733531, 20.92018922310777285 ) ) ;
#7556 = DIRECTION ( 'NONE',  ( 0.000000000000000000, 0.000000000000000000, 1.000000000000000000 ) ) ;
#7557 = ORIENTED_EDGE ( 'NONE', *, *, #22503, .T. ) ;
#7558 = ORIENTED_EDGE ( 'NONE', *, *, #19074, .T. ) ;
#7559 = CARTESIAN_POINT ( 'NONE',  ( -100.7734535825088500, 16.03295912088713848, -16.03295912088698927 ) ) ;
#7560 = CARTESIAN_POINT ( 'NONE',  ( -210.0000000000000284, 61.50000000000009948, 66.50000000000005684 ) ) ;
#7561 = ORIENTED_EDGE ( 'NONE', *, *, #18243, .F. ) ;
#7562 = CARTESIAN_POINT ( 'NONE',  ( -259.2033419157646676, -9.517827891722680178, -40.00000000000002132 ) ) ;
#7563 = CARTESIAN_POINT ( 'NONE',  ( -94.58414068588119505, -20.73981583676798479, 8.590713000820761280 ) ) ;
#7564 = ORIENTED_EDGE ( 'NONE', *, *, #8835, .F. ) ;
#7565 = CARTESIAN_POINT ( 'NONE',  ( 199.9999999999995453, -10.04557064260861843, 16.14007440661455206 ) ) ;
#7566 = DIRECTION ( 'NONE',  ( 0.000000000000000000, 1.000000000000000000, 0.000000000000000000 ) ) ;
#7567 = CARTESIAN_POINT ( 'NONE',  ( -162.0762913951020892, 29.48230308784758691, 29.48230308784772191 ) ) ;
#7568 = DIRECTION ( 'NONE',  ( 0.000000000000000000, 0.000000000000000000, 1.000000000000000000 ) ) ;
#7569 = CARTESIAN_POINT ( 'NONE',  ( -135.8532207217289738, 7.002209520526292428E-15, -9.153146818113572891 ) ) ;
#7570 = CARTESIAN_POINT ( 'NONE',  ( -189.4799804244525490, -23.69387126430439494, 43.33513910317159201 ) ) ;
#7571 = DIRECTION ( 'NONE',  ( 0.000000000000000000, 0.000000000000000000, -1.000000000000000000 ) ) ;
#7572 = CARTESIAN_POINT ( 'NONE',  ( -678.9461782662772293, 90.00000000000000000, 30.00000000000158096 ) ) ;
#7573 = CYLINDRICAL_SURFACE ( 'NONE', #24715, 10.00000000000004796 ) ;
#7574 = CARTESIAN_POINT ( 'NONE',  ( 184.8905102610680444, -40.00000000000021316, 20.92133201514402430 ) ) ;
#7575 = ADVANCED_FACE ( 'NONE', ( #19516 ), #4136, .T. ) ;
#7576 = CARTESIAN_POINT ( 'NONE',  ( -105.2055636155751728, -14.22328983910611555, 16.17146666061736937 ) ) ;
#7577 = CARTESIAN_POINT ( 'NONE',  ( 0.2972598230769976091, -10.13633138497479180, 10.13633138497468522 ) ) ;
#7578 = CARTESIAN_POINT ( 'NONE',  ( 163.1118516004056573, 40.00000000000014921, -27.26290988616858968 ) ) ;
#7579 = CARTESIAN_POINT ( 'NONE',  ( 91.82158438592156813, -16.11829626348402655, -40.45024623143966380 ) ) ;
#7580 = CARTESIAN_POINT ( 'NONE',  ( 155.4809970915716235, 27.66446758342027223, 11.45899766888373783 ) ) ;
#7581 = VECTOR ( 'NONE', #14565, 1000.000000000000000 ) ;
#7582 = DIRECTION ( 'NONE',  ( -0.000000000000000000, -0.000000000000000000, 1.000000000000000000 ) ) ;
#7583 = CARTESIAN_POINT ( 'NONE',  ( 14.38125909742180220, 40.00000000000017764, -15.17850393972591760 ) ) ;
#7584 = CARTESIAN_POINT ( 'NONE',  ( -259.2033419157646676, -40.00000000000017764, 30.48217210827725054 ) ) ;
#7585 = CARTESIAN_POINT ( 'NONE',  ( -30.26275506840324070, -27.08623969584595770, 29.48230279907789608 ) ) ;
#7586 = CARTESIAN_POINT ( 'NONE',  ( 192.4448373802101173, -42.42640687116510634, 14.14213562375845257 ) ) ;
#7587 = CARTESIAN_POINT ( 'NONE',  ( -183.1091233173586090, -22.43565125817906392, -41.47045062402216331 ) ) ;
#7588 = CARTESIAN_POINT ( 'NONE',  ( 192.4448373802100889, 14.14213562375893574, -14.14213562375874922 ) ) ;
#7589 = ORIENTED_EDGE ( 'NONE', *, *, #13932, .F. ) ;
#7590 = CARTESIAN_POINT ( 'NONE',  ( 146.6084372240433993, 3.800685668858732935, -3.800685668858610367 ) ) ;
#7591 = CARTESIAN_POINT ( 'NONE',  ( 170.2234770963711128, 24.55285855007190321, 0.000000000000000000 ) ) ;
#7592 = CARTESIAN_POINT ( 'NONE',  ( -624.5543896866091700, 28.38207856527901995, 34.92076931028241660 ) ) ;
#7593 = CARTESIAN_POINT ( 'NONE',  ( -135.8532207217289738, -6.472252184283586729, -50.09629031063973770 ) ) ;
#7594 = CARTESIAN_POINT ( 'NONE',  ( -87.02123777084361222, 5.414077845889153195, 20.76518631983113750 ) ) ;
#7595 = EDGE_LOOP ( 'NONE', ( #15956, #1490 ) ) ;
#7596 = CARTESIAN_POINT ( 'NONE',  ( -109.1264249741485060, 13.72187187123402907, -33.12752917269585851 ) ) ;
#7597 = CARTESIAN_POINT ( 'NONE',  ( 199.0224076953712711, -19.86590228279781201, -2.420100283956707621 ) ) ;
#7598 = CARTESIAN_POINT ( 'NONE',  ( -40.07203023092437633, 11.15662918590678565, 34.25109662808139177 ) ) ;
#7599 = EDGE_LOOP ( 'NONE', ( #3520, #20246 ) ) ;
#7600 = EDGE_LOOP ( 'NONE', ( #11859, #16068 ) ) ;
#7601 = CARTESIAN_POINT ( 'NONE',  ( 136.1360204305621266, 4.966164525587089429, 2.449293598294708485E-15 ) ) ;
#7602 = CARTESIAN_POINT ( 'NONE',  ( -194.7884774423165197, -44.44046305923735929, -18.40784251728739562 ) ) ;
#7603 = CARTESIAN_POINT ( 'NONE',  ( -135.8532207217289738, 40.00000000000002842, -9.153146818113432559 ) ) ;
#7604 = DIRECTION ( 'NONE',  ( 0.000000000000000000, -1.000000000000000000, 0.000000000000000000 ) ) ;
#7605 = CARTESIAN_POINT ( 'NONE',  ( -56.48582580120559271, 21.81201906317798489, -21.81201906317746619 ) ) ;
#7606 = CARTESIAN_POINT ( 'NONE',  ( -259.2033419157646676, 39.99999999999987921, 9.517827891723049660 ) ) ;
#7607 = CARTESIAN_POINT ( 'NONE',  ( 199.9999999999998863, -18.14641137086378819, -5.658975142792487922 ) ) ;
#7608 = CARTESIAN_POINT ( 'NONE',  ( 146.6084372240433993, 1.478241399363601114E-13, -34.62501878078305850 ) ) ;
#7609 = CARTESIAN_POINT ( 'NONE',  ( -198.1130638040447423, 43.61599283946033268, 18.06633577047154304 ) ) ;
#7610 = CARTESIAN_POINT ( 'NONE',  ( -4.037857402784342575, -13.82822410908647903, -46.99101396955030907 ) ) ;
#7611 = CARTESIAN_POINT ( 'NONE',  ( -213.1075012329537230, 18.58567234101174037, -37.98287015391222354 ) ) ;
#7612 = CARTESIAN_POINT ( 'NONE',  ( -87.13361725327075646, -15.19799821270861706, 15.19799821270823159 ) ) ;
#7613 = FACE_OUTER_BOUND ( 'NONE', #25812, .T. ) ;
#7614 = PLANE ( 'NONE',  #22333 ) ;
#7615 = CARTESIAN_POINT ( 'NONE',  ( 19.06497207195980792, -14.19242893257839988, 40.00000000000002132 ) ) ;
#7616 = CARTESIAN_POINT ( 'NONE',  ( -280.0000000000000568, 19.99999999999996092, -40.00000000000002132 ) ) ;
#7617 = CARTESIAN_POINT ( 'NONE',  ( -238.4067589809705794, -0.6820004457913680929, 0.6820004457913170226 ) ) ;
#7618 = CARTESIAN_POINT ( 'NONE',  ( 136.1360204305621266, 35.03383547441298873, 0.000000000000000000 ) ) ;
#7619 = CARTESIAN_POINT ( 'NONE',  ( -105.2502153031283143, 3.401878988843269003, 21.20171025720689784 ) ) ;
#7620 = CARTESIAN_POINT ( 'NONE',  ( -77.90255099906769942, 20.29001641120678201, -8.064892378658056415 ) ) ;
#7621 = CARTESIAN_POINT ( 'NONE',  ( 200.0000000000000000, -14.14213562373106114, 42.42640687119278908 ) ) ;
#7622 = CARTESIAN_POINT ( 'NONE',  ( 0.2972598230769930572, 54.33493731733936016, 2.449293598294708485E-15 ) ) ;
#7623 = VERTEX_POINT ( 'NONE', #7932 ) ;
#7624 = AXIS2_PLACEMENT_3D ( 'NONE', #16907, #4819, #8390 ) ;
#7625 = CARTESIAN_POINT ( 'NONE',  ( 83.01683444506817011, -24.01517293250395824, 9.947410331339252565 ) ) ;
#7626 = CARTESIAN_POINT ( 'NONE',  ( -4.039451493210485467, -13.82811171175474207, 46.99046209229799587 ) ) ;
#7627 = CARTESIAN_POINT ( 'NONE',  ( -91.56559293963834989, 12.25131212657490209, -44.31723036834897300 ) ) ;
#7628 = CARTESIAN_POINT ( 'NONE',  ( 136.1360204305621266, 5.219216885335291329E-15, 4.966164525587064560 ) ) ;
#7629 = CARTESIAN_POINT ( 'NONE',  ( 14.38125909742180752, 10.73282306404735387, -10.73282306404708919 ) ) ;
#7630 = CARTESIAN_POINT ( 'NONE',  ( -238.4067589809705794, 0.9644942799825385604, 40.00000000000002132 ) ) ;
#7631 = CARTESIAN_POINT ( 'NONE',  ( -213.1075012329537230, 13.71589010951907994, 0.000000000000000000 ) ) ;
#7632 = DIRECTION ( 'NONE',  ( 0.01051738792038020565, -0.9166396752531025260, 0.3995761383056042337 ) ) ;
#7633 = CARTESIAN_POINT ( 'NONE',  ( 199.9999999999998863, -4.328516665792998097, 18.51095020188552809 ) ) ;
#7634 = CARTESIAN_POINT ( 'NONE',  ( 199.9999999999999716, -14.30114536083090471, 12.54040393066167347 ) ) ;
#7635 = CARTESIAN_POINT ( 'NONE',  ( -30.26275506840322649, -29.48230279907769358, -29.48230279907820162 ) ) ;
#7636 = VECTOR ( 'NONE', #16678, 1000.000000000000000 ) ;
#7637 = CARTESIAN_POINT ( 'NONE',  ( -114.7292050955122278, 21.84104191940862449, -3.341916304163401463 ) ) ;
#7638 = CARTESIAN_POINT ( 'NONE',  ( 130.8568914410475372, -3.326198072800416995E-13, 34.05028731879788495 ) ) ;
#7639 = CARTESIAN_POINT ( 'NONE',  ( 192.4448373802101173, 14.14213562375922884, -42.42640687116488607 ) ) ;
#7641 = CARTESIAN_POINT ( 'NONE',  ( -208.1127848780265026, 10.60833733269551615, -10.60833733269529766 ) ) ;
#7640 = CARTESIAN_POINT ( 'NONE',  ( -56.48582580120558561, -21.81201906317755146, -21.81201906317792449 ) ) ;
#7642 = CARTESIAN_POINT ( 'NONE',  ( -91.56559293963834989, -44.31723036834885932, -12.25131212657538171 ) ) ;
#7643 = CARTESIAN_POINT ( 'NONE',  ( -114.7539999065896126, -2.778737770292790898, -21.97438050586149316 ) ) ;
#7644 = CARTESIAN_POINT ( 'NONE',  ( -716.9846540392142060, -66.50000000000001421, 66.50000000000005684 ) ) ;
#7645 = EDGE_CURVE ( 'NONE', #11213, #10975, #9532, .T. ) ;
#7647 = CARTESIAN_POINT ( 'NONE',  ( 91.82158438592159655, -40.00000000000008527, 22.79471317813456110 ) ) ;
#7646 = CARTESIAN_POINT ( 'NONE',  ( -162.0762913951021176, 57.76657433523994456, -1.198031840315424867 ) ) ;
#7648 = CARTESIAN_POINT ( 'NONE',  ( 192.4448373802101173, 14.14213562375862665, 42.42640687116509213 ) ) ;
#7649 = CARTESIAN_POINT ( 'NONE',  ( -100.7734535825088358, -16.03295912088728770, 16.03295912088687913 ) ) ;
#7650 = CARTESIAN_POINT ( 'NONE',  ( -56.48582580120559982, 30.84685318188643421, 40.00000000000002132 ) ) ;
#7651 = VERTEX_POINT ( 'NONE', #23900 ) ;
#7652 = CARTESIAN_POINT ( 'NONE',  ( 57.59792236341147031, 54.84617931850881689, -1.722363176414946073 ) ) ;
#7653 = EDGE_CURVE ( 'NONE', #7864, #23212, #1300, .T. ) ;
#7654 = CARTESIAN_POINT ( 'NONE',  ( 36.90243737664644641, 38.55584411169299841, 15.97035353980611205 ) ) ;
#7655 = CARTESIAN_POINT ( 'NONE',  ( 67.79414719548810808, 14.15005687161725589, 28.72755866868557106 ) ) ;
#7656 = CARTESIAN_POINT ( 'NONE',  ( -192.9588430854690273, 14.46834944099966336, 40.00000000000002132 ) ) ;
#7657 = EDGE_CURVE ( 'NONE', #22554, #19424, #9538, .T. ) ;
#7658 = ADVANCED_FACE ( 'NONE', ( #16317 ), #16455, .T. ) ;
#7659 = EDGE_LOOP ( 'NONE', ( #25111, #14780, #18300, #18336 ) ) ;
#7660 = CARTESIAN_POINT ( 'NONE',  ( -189.0115211946963427, -43.33403054566051793, 17.94954316430237284 ) ) ;
#7661 = CIRCLE ( 'NONE', #8109, 34.99999999999999289 ) ;
#7662 = CARTESIAN_POINT ( 'NONE',  ( 200.0000000000001421, -14.29287298608315382, 12.53529920294169386 ) ) ;
#7663 = CARTESIAN_POINT ( 'NONE',  ( -3.966425590329079931, -23.46521855348130714, 43.02666064534189871 ) ) ;
#7664 = CARTESIAN_POINT ( 'NONE',  ( 22.95085416411744461, 17.86294511971856380, -43.12496437194744203 ) ) ;
#7665 = CARTESIAN_POINT ( 'NONE',  ( 199.0062089136474128, 7.336486126005011599, -18.60345363517511430 ) ) ;
#7666 = CARTESIAN_POINT ( 'NONE',  ( 125.5832160019859884, -28.05309928654004281, 11.61997419108369733 ) ) ;
#7667 = DIRECTION ( 'NONE',  ( -1.000000000000000000, -1.836970198721030181E-16, -0.000000000000000000 ) ) ;
#7668 = CARTESIAN_POINT ( 'NONE',  ( -315.0000000000000568, -4.857225732735059864E-14, -31.79780246617542616 ) ) ;
#7669 = CARTESIAN_POINT ( 'NONE',  ( -213.1075012329537230, 9.698598906438871126, -66.26714140136179765 ) ) ;
#7670 = CARTESIAN_POINT ( 'NONE',  ( 130.8568914410475372, -5.949712681206667853, -2.449293598294708485E-15 ) ) ;
#7671 = AXIS2_PLACEMENT_3D ( 'NONE', #7728, #15840, #4032 ) ;
#7673 = DIRECTION ( 'NONE',  ( -1.000000000000000000, -0.000000000000000000, -0.000000000000000000 ) ) ;
#7672 = CARTESIAN_POINT ( 'NONE',  ( -144.0562696877211124, 14.68019673968441552, -29.54283206240011950 ) ) ;
#7674 = CARTESIAN_POINT ( 'NONE',  ( 170.2234770963711128, 24.55285855007190321, 0.000000000000000000 ) ) ;
#7675 = CARTESIAN_POINT ( 'NONE',  ( 91.82158438592156813, 17.20528682183302038, -40.00000000000002132 ) ) ;
#7676 = CIRCLE ( 'NONE', #25963, 21.53474504356805852 ) ;
#7677 = CARTESIAN_POINT ( 'NONE',  ( -213.1075012329537230, 53.71589010953660193, 40.00000000000002132 ) ) ;
#7678 = CARTESIAN_POINT ( 'NONE',  ( -86.96347745069643054, -39.99999999999985079, -18.24025645688394448 ) ) ;
#7679 = CARTESIAN_POINT ( 'NONE',  ( 136.1360204305621266, -3.419521671106983309E-13, 35.03383547441296741 ) ) ;
#7680 = CARTESIAN_POINT ( 'NONE',  ( 130.8568914410475088, 52.36146031193427319, -4.207082182989173802 ) ) ;
#7681 = ORIENTED_EDGE ( 'NONE', *, *, #3619, .F. ) ;
#7682 = DIRECTION ( 'NONE',  ( 0.000000000000000000, -0.9166903767145597737, 0.3995982397845596612 ) ) ;
#7683 = CARTESIAN_POINT ( 'NONE',  ( -259.2033419157646676, -6.730120644403570829, -6.730120644403545960 ) ) ;
#7684 = CARTESIAN_POINT ( 'NONE',  ( 130.8568914410475372, -24.07718906447255947, 24.07718906447199458 ) ) ;
#7685 = CARTESIAN_POINT ( 'NONE',  ( -94.58360650948853277, -9.000712009830975191, 20.58386743644871331 ) ) ;
#7686 = ITEM_DEFINED_TRANSFORMATION ( 'NONE', 'NONE', #9156,  #21058 ) ;
#7687 = ORIENTED_EDGE ( 'NONE', *, *, #25360, .T. ) ;
#7688 = ORIENTED_EDGE ( 'NONE', *, *, #21906, .F. ) ;
#7689 = CARTESIAN_POINT ( 'NONE',  ( -91.56559293963836410, -12.25131212657462321, -44.31723036834905827 ) ) ;
#7690 = CARTESIAN_POINT ( 'NONE',  ( 20.38198589864675014, -43.75891014378044019, -18.12553405624110781 ) ) ;
#7691 = EDGE_CURVE ( 'NONE', #13855, #15801, #3706, .T. ) ;
#7692 = EDGE_LOOP ( 'NONE', ( #19581, #18546, #11366, #9730 ) ) ;
#7693 = CARTESIAN_POINT ( 'NONE',  ( 130.8568914410475088, 5.949712681206719367, -40.00000000000002132 ) ) ;
#7694 = CARTESIAN_POINT ( 'NONE',  ( -88.37877758187065069, -19.92653024478079615, 8.575405934537359443 ) ) ;
#7695 = ORIENTED_EDGE ( 'NONE', *, *, #8822, .T. ) ;
#7696 = CARTESIAN_POINT ( 'NONE',  ( 199.9999999999999716, 17.67160698027466736, 6.995183481556395577 ) ) ;
#7697 = VECTOR ( 'NONE', #4137, 1000.000000000000000 ) ;
#7698 = CARTESIAN_POINT ( 'NONE',  ( -210.0000000000000284, -66.50000000000001421, 66.50000000000005684 ) ) ;
#7699 = CARTESIAN_POINT ( 'NONE',  ( 151.7948205124836250, 4.785054706301690608, 4.785054706301682614 ) ) ;
#7700 = LINE ( 'NONE', #5588, #8515 ) ;
#7701 = CARTESIAN_POINT ( 'NONE',  ( 170.2234770963711128, 1.169953928977015745E-13, -24.55285855007187124 ) ) ;
#7702 = CARTESIAN_POINT ( 'NONE',  ( 146.6084372240433993, -34.62501878078303008, 0.000000000000000000 ) ) ;
#7703 = CARTESIAN_POINT ( 'NONE',  ( 0.2972598230770011618, 10.13633138497555919, -66.70487387989845729 ) ) ;
#7704 = DIRECTION ( 'NONE',  ( 0.000000000000000000, 0.000000000000000000, -1.000000000000000000 ) ) ;
#7705 = DIRECTION ( 'NONE',  ( 0.000000000000000000, -0.3028247695821854046, 0.9530462522498561739 ) ) ;
#7706 = CARTESIAN_POINT ( 'NONE',  ( -213.1075012329537230, -39.99999999999991473, -13.71589010951953647 ) ) ;
#7707 = CARTESIAN_POINT ( 'NONE',  ( -110.0960685945389343, -12.40690815812826386, 15.98210693808425376 ) ) ;
#7708 = CARTESIAN_POINT ( 'NONE',  ( -91.56559293963834989, -40.53558337403669753, -16.03295912088728770 ) ) ;
#7709 = CARTESIAN_POINT ( 'NONE',  ( 151.7948205124836250, 33.23291073765556547, 0.000000000000000000 ) ) ;
#7710 = CARTESIAN_POINT ( 'NONE',  ( 163.1118516004056573, -9.006482792073960297, -47.56205970284963769 ) ) ;
#7711 = CARTESIAN_POINT ( 'NONE',  ( 200.0000000000000000, -1.836970198721029589E-15, 0.000000000000000000 ) ) ;
#7712 = CARTESIAN_POINT ( 'NONE',  ( -77.78673448795234435, 9.959188558496546051, -19.58653132801435959 ) ) ;
#7713 = CARTESIAN_POINT ( 'NONE',  ( -213.1075012329537230, 1.045191102001431893E-13, -13.71589010951911902 ) ) ;
#7714 = CARTESIAN_POINT ( 'NONE',  ( 199.9999999999999432, 1.065690307512836407E-13, -20.00000000000010303 ) ) ;
#7715 = CARTESIAN_POINT ( 'NONE',  ( 130.8568914410475372, 4.207082182992862407, 4.207082182992856190 ) ) ;
#7716 = AXIS2_PLACEMENT_3D ( 'NONE', #21336, #1493, #11335 ) ;
#7717 = CARTESIAN_POINT ( 'NONE',  ( -114.7410223956348148, 17.58920299499807172, 13.38943653989989890 ) ) ;
#7718 = CARTESIAN_POINT ( 'NONE',  ( -195.1685814578900420, -24.52825302095775939, -44.46431112711859157 ) ) ;
#7719 = CARTESIAN_POINT ( 'NONE',  ( -238.4067589809705794, -0.6820004457913680929, 0.6820004457913170226 ) ) ;
#7720 = ORIENTED_EDGE ( 'NONE', *, *, #2001, .F. ) ;
#7721 = CARTESIAN_POINT ( 'NONE',  ( -100.7734535825088500, -16.03295912088659492, -40.53558337403696044 ) ) ;
#7722 = CARTESIAN_POINT ( 'NONE',  ( 0.2972598230769983307, -14.33493731733933352, -40.00000000000002132 ) ) ;
#7723 =( BOUNDED_SURFACE ( )  B_SPLINE_SURFACE ( 3, 2, ( 
 ( #6155, #20264, #4041 ),
 ( #20129, #10407, #8408 ),
 ( #8273, #2043, #24389 ),
 ( #18524, #16397, #20662 ),
 ( #10149, #14532, #14401 ),
 ( #18252, #14265, #22530 ),
 ( #10012, #6414, #4312 ),
 ( #20527, #305, #1908 ),
 ( #16530, #18120, #26272 ),
 ( #8010, #24255, #8545 ),
 ( #4703, #6810, #14926 ),
 ( #2710, #23063, #8948 ) ),
 .UNSPECIFIED., .F., .F., .F. ) 
 B_SPLINE_SURFACE_WITH_KNOTS ( ( 4, 2, 2, 2, 2, 4 ),
 ( 3, 3 ),
 ( 0.006022589392325016291, 0.01254516766564325869, 0.01580645680230238076, 0.01906774593896149936, 0.02559032421227974002, 0.03211290248559798416 ),
 ( 0.000000000000000000, 1.000000000000000000 ),
 .UNSPECIFIED. ) 
 GEOMETRIC_REPRESENTATION_ITEM ( )  RATIONAL_B_SPLINE_SURFACE ( (
 ( 1.000000000000000000, 0.9998834880171258988, 1.000000000000000000),
 ( 1.000000000000000000, 0.9998139205012253061, 1.000000000000000000),
 ( 1.000000000000000000, 0.9997315632444677691, 1.000000000000000000),
 ( 1.000000000000000000, 0.9996405464946958030, 1.000000000000000000),
 ( 1.000000000000000000, 0.9996155081776924023, 1.000000000000000000),
 ( 1.000000000000000000, 0.9995814087511104562, 1.000000000000000000),
 ( 1.000000000000000000, 0.9995724100939918921, 1.000000000000000000),
 ( 1.000000000000000000, 0.9995726760936894939, 1.000000000000000000),
 ( 1.000000000000000000, 0.9996103361816741639, 1.000000000000000000),
 ( 1.000000000000000000, 0.9997312749796802844, 1.000000000000000000),
 ( 1.000000000000000000, 0.9998135910914284219, 1.000000000000000000),
 ( 1.000000000000000000, 0.9998834880173383954, 1.000000000000000000) ) ) 
 REPRESENTATION_ITEM ( '' )  SURFACE ( )  );
#7724 = CARTESIAN_POINT ( 'NONE',  ( 200.0000000000000000, -14.14213562373046784, -42.42640687119298804 ) ) ;
#7725 = CARTESIAN_POINT ( 'NONE',  ( -87.13361725327075646, -2.411356650979015128E-13, 21.49321519333430430 ) ) ;
#7726 = ORIENTED_EDGE ( 'NONE', *, *, #9144, .T. ) ;
#7727 = CARTESIAN_POINT ( 'NONE',  ( -259.2033419157646676, -1.473088368616265084E-13, 9.517827891722632216 ) ) ;
#7728 = CARTESIAN_POINT ( 'NONE',  ( -716.9846540392142060, 66.50000000000009948, -66.50000000000005684 ) ) ;
#7729 = CARTESIAN_POINT ( 'NONE',  ( -4.027137536850666777, 13.82877337592787015, 46.99492183298313819 ) ) ;
#7730 = ORIENTED_EDGE ( 'NONE', *, *, #13704, .F. ) ;
#7731 = ORIENTED_EDGE ( 'NONE', *, *, #18822, .F. ) ;
#7732 = CARTESIAN_POINT ( 'NONE',  ( 163.1118516004056573, 12.73709011382478273, 2.449293598294708485E-15 ) ) ;
#7733 = CARTESIAN_POINT ( 'NONE',  ( -195.5008451367067721, -44.52806290063275441, -18.44412755964722450 ) ) ;
#7734 = CARTESIAN_POINT ( 'NONE',  ( -30.26275506840325136, 40.00000000000001421, 1.694272468446399227 ) ) ;
#7735 = CARTESIAN_POINT ( 'NONE',  ( -114.4364955367327497, -20.04994829327637262, -8.644468109209869411 ) ) ;
#7736 = LINE ( 'NONE', #25860, #4087 ) ;
#7737 = CARTESIAN_POINT ( 'NONE',  ( 48.46158794344649579, 18.19743102720972416, -35.02055625264701888 ) ) ;
#7738 = DIRECTION ( 'NONE',  ( -1.000000000000000000, 1.836970198721030181E-16, 0.000000000000000000 ) ) ;
#7739 = CARTESIAN_POINT ( 'NONE',  ( 199.0241407150285227, -2.291925048877014870, 19.87495682421008425 ) ) ;
#7740 = EDGE_CURVE ( 'NONE', #13337, #4265, #20450, .T. ) ;
#7741 = CARTESIAN_POINT ( 'NONE',  ( -195.2739252856439407, 43.39389462262437291, 17.97433967688010270 ) ) ;
#7742 = CARTESIAN_POINT ( 'NONE',  ( 6.762329110801217347, -18.56720258520416067, -44.82519229650321790 ) ) ;
#7743 = CARTESIAN_POINT ( 'NONE',  ( 163.1118516004056573, -37.29075403953166301, 19.27778845539196695 ) ) ;
#7744 = CARTESIAN_POINT ( 'NONE',  ( 116.7964245048381429, -19.78678521258544620, 19.78678521258498435 ) ) ;
#7745 = CARTESIAN_POINT ( 'NONE',  ( -208.1127848780264742, -67.17687982763172272, 10.60833733270744617 ) ) ;
#7746 = CARTESIAN_POINT ( 'NONE',  ( 91.82158438592159655, -40.00000000000017764, 17.20528682183258340 ) ) ;
#7747 = DIRECTION ( 'NONE',  ( -1.000000000000000000, -1.836970198721024264E-16, 0.000000000000000000 ) ) ;
#7748 = FACE_OUTER_BOUND ( 'NONE', #16341, .T. ) ;
#7749 = CARTESIAN_POINT ( 'NONE',  ( -259.2033419157646676, -30.48217210827744950, 40.00000000000002132 ) ) ;
#7750 = EDGE_CURVE ( 'NONE', #14209, #23802, #14456, .T. ) ;
#7751 = CARTESIAN_POINT ( 'NONE',  ( 136.1360204305621551, 24.77266263493108411, 31.79587985999273769 ) ) ;
#7752 = CARTESIAN_POINT ( 'NONE',  ( 14.38125909742182884, -55.17850393974264733, -40.00000000000002132 ) ) ;
#7753 = CARTESIAN_POINT ( 'NONE',  ( -210.0000000000000284, 71.50000000000009948, 66.50000000000005684 ) ) ;
#7754 = CARTESIAN_POINT ( 'NONE',  ( -213.1075012329537230, 40.00000000000012790, -13.71589010951869980 ) ) ;
#7755 = CARTESIAN_POINT ( 'NONE',  ( 4.995406935893290878, 39.06748935135185263, 39.06748935135198764 ) ) ;
#7756 = EDGE_CURVE ( 'NONE', #24877, #4727, #12083, .T. ) ;
#7757 = CARTESIAN_POINT ( 'NONE',  ( 14.38125909742180752, 15.17850393972634038, -40.00000000000002132 ) ) ;
#7758 = ORIENTED_EDGE ( 'NONE', *, *, #8481, .T. ) ;
#7759 = EDGE_CURVE ( 'NONE', #20976, #3723, #21716, .T. ) ;
#7760 = CARTESIAN_POINT ( 'NONE',  ( 44.82887508593488946, -38.96139886170605848, 12.17256213108278828 ) ) ;
#7761 = CARTESIAN_POINT ( 'NONE',  ( -213.1075012329537230, 66.26714140136188291, 9.698598906438215650 ) ) ;
#7762 = CARTESIAN_POINT ( 'NONE',  ( 91.82158438592159655, -40.00000000000008527, 22.79471317813456110 ) ) ;
#7763 = CARTESIAN_POINT ( 'NONE',  ( -192.9588430854689989, 10.23066800230756712, -10.23066800230735396 ) ) ;
#7764 = CARTESIAN_POINT ( 'NONE',  ( 151.7948205124836250, -3.202120068677277203E-13, 33.23291073765553705 ) ) ;
#7765 = CARTESIAN_POINT ( 'NONE',  ( 14.38125909742180752, 15.17850393972634038, 0.000000000000000000 ) ) ;
#7766 = CARTESIAN_POINT ( 'NONE',  ( -575.0231298121466352, 75.00000000000000000, -30.00000000000202505 ) ) ;
#7767 = CARTESIAN_POINT ( 'NONE',  ( 199.9999999999996874, 13.64679526057751069, 13.22824625860694070 ) ) ;
#7768 = CARTESIAN_POINT ( 'NONE',  ( 200.0000000000000284, -18.10041568647748278, 5.811528243237751745 ) ) ;
#7769 = CARTESIAN_POINT ( 'NONE',  ( -91.56559293963834989, 40.53558337403654832, 16.03295912088756481 ) ) ;
#7770 = CARTESIAN_POINT ( 'NONE',  ( 170.2234770963711128, 45.64576402573196390, -10.92277846919159856 ) ) ;
#7771 = CARTESIAN_POINT ( 'NONE',  ( -77.58504657351252831, -21.97438139950685354, -2.778622652594447295 ) ) ;
#7772 = CARTESIAN_POINT ( 'NONE',  ( -82.28266731796803413, 17.99064928892941140, -9.155589012553823736 ) ) ;
#7773 = CARTESIAN_POINT ( 'NONE',  ( -86.96347745069644475, -12.89780903124395195, -12.89780903124416511 ) ) ;
#7775 = CARTESIAN_POINT ( 'NONE',  ( 4.995406935893289102, 10.78321810389013002, -10.78321810388986712 ) ) ;
#7774 = CARTESIAN_POINT ( 'NONE',  ( 130.8568914410475088, 24.07718906446937623, -32.49135343045455215 ) ) ;
#7776 = CARTESIAN_POINT ( 'NONE',  ( 151.7948205124836534, -51.78348778862529400, -4.785054706299085581 ) ) ;
#7777 = CARTESIAN_POINT ( 'NONE',  ( 184.8905102610680444, -20.92133201514440799, 0.000000000000000000 ) ) ;
#7778 = CARTESIAN_POINT ( 'NONE',  ( 199.0155675229561609, 14.66025079576549750, 13.60702933000608006 ) ) ;
#7780 = CARTESIAN_POINT ( 'NONE',  ( 192.4448373802101173, -39.99999999999991473, -20.00000000003956302 ) ) ;
#7779 = CARTESIAN_POINT ( 'NONE',  ( -238.4067589809705794, 57.25054294065799354, -0.6820004457334954973 ) ) ;
#7781 = CARTESIAN_POINT ( 'NONE',  ( 0.2972598230769923355, 18.14793986248697166, 38.42060263243675422 ) ) ;
#7782 = CARTESIAN_POINT ( 'NONE',  ( -213.1075012329537230, 37.98287015391211696, 18.58567234101190735 ) ) ;
#7783 = CARTESIAN_POINT ( 'NONE',  ( 0.2972598230769930017, 54.33493731733936016, 40.00000000000002132 ) ) ;
#7784 = VERTEX_POINT ( 'NONE', #14717 ) ;
#7785 = CARTESIAN_POINT ( 'NONE',  ( 136.1360204305621551, 3.511608612530801032, -53.05693388239316022 ) ) ;
#7786 = CARTESIAN_POINT ( 'NONE',  ( 94.73518454776767328, 19.78402239393997419, 8.194810393863161124 ) ) ;
#7787 = CARTESIAN_POINT ( 'NONE',  ( 23.49666234703747847, 13.79192166426321720, 46.76389514419428650 ) ) ;
#7788 = CARTESIAN_POINT ( 'NONE',  ( -162.0762913951020892, 1.694272876828294194, 0.000000000000000000 ) ) ;
#7789 = ORIENTED_EDGE ( 'NONE', *, *, #7052, .T. ) ;
#7790 = CARTESIAN_POINT ( 'NONE',  ( -189.5227390968213115, -43.46195835885610137, 18.00253259953374751 ) ) ;
#7791 = CARTESIAN_POINT ( 'NONE',  ( 199.9999999999996874, -18.85616045826023779, 2.487226269395955480 ) ) ;
#7792 = CARTESIAN_POINT ( 'NONE',  ( 3.869409319468993580, -14.12455301873678515, 48.96737585073453403 ) ) ;
#7793 = EDGE_CURVE ( 'NONE', #14842, #10807, #853, .T. ) ;
#7794 = CARTESIAN_POINT ( 'NONE',  ( 23.36927571439210993, 13.80130822340207430, -46.80992244775424638 ) ) ;
#7795 = CARTESIAN_POINT ( 'NONE',  ( 199.0112868605082497, -6.441215115722609852, -18.93473387006624620 ) ) ;
#7796 = EDGE_CURVE ( 'NONE', #14640, #11418, #23008, .T. ) ;
#7797 = CARTESIAN_POINT ( 'NONE',  ( -716.9846540392142060, 82.50000000000008527, 52.49999999999980105 ) ) ;
#7798 = CARTESIAN_POINT ( 'NONE',  ( -129.2303573021155216, -11.67678754051281409, 24.84170325990223205 ) ) ;
#7799 = CARTESIAN_POINT ( 'NONE',  ( -91.56559293963834989, -16.03295912088659492, -40.53558337403696044 ) ) ;
#7800 = CARTESIAN_POINT ( 'NONE',  ( 91.82158438592156813, 17.20528682183302038, 40.00000000000002132 ) ) ;
#7802 = FACE_OUTER_BOUND ( 'NONE', #24410, .T. ) ;
#7801 = CARTESIAN_POINT ( 'NONE',  ( -174.2682069750576659, 16.26528465553901981, -39.26787081121104706 ) ) ;
#7803 = EDGE_CURVE ( 'NONE', #10709, #4560, #10679, .T. ) ;
#7804 = CARTESIAN_POINT ( 'NONE',  ( 163.1118516004056573, 27.26290988616875310, 0.000000000000000000 ) ) ;
#7805 = CARTESIAN_POINT ( 'NONE',  ( -105.3755690713226585, -18.24025645688353947, -40.00000000000002132 ) ) ;
#7806 = CARTESIAN_POINT ( 'NONE',  ( -30.26275506840324070, 1.694272468446254232, 0.000000000000000000 ) ) ;
#7807 = CARTESIAN_POINT ( 'NONE',  ( -162.0762913951020892, 4.094006889353306706E-13, -41.69427287682835015 ) ) ;
#7808 = CARTESIAN_POINT ( 'NONE',  ( -238.4067589809705794, -3.369206980223063916E-14, -0.9644942799825824142 ) ) ;
#7809 = CARTESIAN_POINT ( 'NONE',  ( 19.06497207195980792, 18.24870850772790831, -38.31983398719609824 ) ) ;
#7810 = ORIENTED_EDGE ( 'NONE', *, *, #15462, .F. ) ;
#7811 = CARTESIAN_POINT ( 'NONE',  ( -86.91014751117378978, 20.05881702300802516, -7.317915707774923284 ) ) ;
#7812 = CARTESIAN_POINT ( 'NONE',  ( -208.1127848780265026, -15.00245453012673202, 0.000000000000000000 ) ) ;
#7813 = DIRECTION ( 'NONE',  ( 1.000000000000000000, -0.000000000000000000, -0.000000000000000000 ) ) ;
#7814 = APPLICATION_PROTOCOL_DEFINITION ( 'draft international standard', 'automotive_design', 1998, #2450 ) ;
#7815 = ORIENTED_EDGE ( 'NONE', *, *, #7740, .F. ) ;
#7816 = ORIENTED_EDGE ( 'NONE', *, *, #16318, .T. ) ;
#7817 = CARTESIAN_POINT ( 'NONE',  ( 57.59792236341148453, -54.84617931850877426, -1.722363176415331099 ) ) ;
#7818 = CARTESIAN_POINT ( 'NONE',  ( 23.54890483848240379, -42.80335737019201758, -23.30407993985230064 ) ) ;
#7819 = ORIENTED_EDGE ( 'NONE', *, *, #5333, .T. ) ;
#7820 = CARTESIAN_POINT ( 'NONE',  ( -162.0762913951021176, 1.694272876828294194, -40.00000000000002132 ) ) ;
#7821 = CARTESIAN_POINT ( 'NONE',  ( -94.58360650941220626, -20.58386743640747341, 9.000712009939409342 ) ) ;
#7822 = ORIENTED_EDGE ( 'NONE', *, *, #17819, .F. ) ;
#7823 = CARTESIAN_POINT ( 'NONE',  ( 199.9999999999999432, 18.93973332185608172, 1.567235916626209535 ) ) ;
#7824 =( BOUNDED_CURVE ( )  B_SPLINE_CURVE ( 3, ( #17572, #15203, #15326, #17194 ),
 .UNSPECIFIED., .F., .F. ) 
 B_SPLINE_CURVE_WITH_KNOTS ( ( 4, 4 ),
 ( 0.004183487405659220247, 0.01388163287021914813 ),
 .UNSPECIFIED. ) 
 CURVE ( )  GEOMETRIC_REPRESENTATION_ITEM ( )  RATIONAL_B_SPLINE_CURVE ( ( 0.6809743333591556924, 0.7608653435686150157, 0.8672072324488964146, 1.000000000000000000 ) ) 
 REPRESENTATION_ITEM ( '' )  );
#7825 = DIRECTION ( 'NONE',  ( 1.000000000000000000, 1.836970198721030181E-16, 0.000000000000000000 ) ) ;
#7826 = CARTESIAN_POINT ( 'NONE',  ( 19.06497207195979726, 38.31983398719629719, -18.24870850772750686 ) ) ;
#7827 = CARTESIAN_POINT ( 'NONE',  ( -144.0562696871581920, -29.54283206217719382, -14.68019673973296868 ) ) ;
#7828 = EDGE_CURVE ( 'NONE', #8666, #26151, #17362, .T. ) ;
#7829 = CARTESIAN_POINT ( 'NONE',  ( -280.0000000000000000, -1.237140859393462838E-13, 20.00000000000001421 ) ) ;
#7830 = CARTESIAN_POINT ( 'NONE',  ( -91.56559293963834989, 17.32597176626808988, 40.00000000000002132 ) ) ;
#7831 = CARTESIAN_POINT ( 'NONE',  ( -91.56559293963834989, 12.25131212657497848, -12.25131212657469426 ) ) ;
#7832 = CARTESIAN_POINT ( 'NONE',  ( -83.28983882461062649, 25.45044590560994990, 25.45044590561006004 ) ) ;
#7833 = CARTESIAN_POINT ( 'NONE',  ( 14.38125909742181818, -40.00000000000007816, 15.17850393972619649 ) ) ;
#7834 = CARTESIAN_POINT ( 'NONE',  ( -208.1127848780264742, -39.99999999999990763, -15.00245453012711394 ) ) ;
#7835 = DIRECTION ( 'NONE',  ( 0.000000000000000000, 0.000000000000000000, -1.000000000000000000 ) ) ;
#7836 = CARTESIAN_POINT ( 'NONE',  ( -280.0000000000000000, -14.14213562373108779, 14.14213562373088529 ) ) ;
#7837 = EDGE_CURVE ( 'NONE', #20782, #6050, #18307, .T. ) ;
#7838 = CARTESIAN_POINT ( 'NONE',  ( 57.59792236341147031, 2.435789363418170872, -40.00000000000002132 ) ) ;
#7839 = EDGE_CURVE ( 'NONE', #24783, #15800, #22979, .T. ) ;
#7840 = CARTESIAN_POINT ( 'NONE',  ( -86.96347745069645896, -12.89780903124382938, -43.67073346367985920 ) ) ;
#7841 = CARTESIAN_POINT ( 'NONE',  ( -190.0000000000000284, -82.49999999999990052, 52.49999999999977973 ) ) ;
#7842 = CARTESIAN_POINT ( 'NONE',  ( 17.75917311731582160, -48.46615948699198384, 14.04884443869907606 ) ) ;
#7843 = CARTESIAN_POINT ( 'NONE',  ( -213.1075012329537230, 40.00000000000012790, -13.71589010951869980 ) ) ;
#7844 = CARTESIAN_POINT ( 'NONE',  ( 146.6084372240433709, -39.99999999999987921, -34.62501878078319351 ) ) ;
#7845 = AXIS2_PLACEMENT_3D ( 'NONE', #25680, #19172, #1077 ) ;
#7846 = CARTESIAN_POINT ( 'NONE',  ( -56.48582580120559982, 21.81201906317778594, -34.75652343174606074 ) ) ;
#7847 = CARTESIAN_POINT ( 'NONE',  ( 4.995406935893297984, -39.06748935135205869, 17.50105314357158193 ) ) ;
#7848 = CARTESIAN_POINT ( 'NONE',  ( -190.0144721487477852, -23.79987203023481968, -43.47822244618638621 ) ) ;
#7849 = CARTESIAN_POINT ( 'NONE',  ( 160.9163046357249129, -125.7889608577475400, 49.61140153332247138 ) ) ;
#7850 = ORIENTED_EDGE ( 'NONE', *, *, #12009, .F. ) ;
#7851 = CARTESIAN_POINT ( 'NONE',  ( 0.2972598230769938343, 10.13633138497486286, -10.13633138497461594 ) ) ;
#7852 = CARTESIAN_POINT ( 'NONE',  ( 14.38125909742180752, 17.55144818341448953, 39.01709431150923280 ) ) ;
#7853 = CARTESIAN_POINT ( 'NONE',  ( -315.0000000000000568, -4.467814962633844109E-14, 31.79780246617542616 ) ) ;
#7854 = DIRECTION ( 'NONE',  ( -0.000000000000000000, 0.000000000000000000, 1.000000000000000000 ) ) ;
#7855 = CARTESIAN_POINT ( 'NONE',  ( -135.8532207217289738, -34.75652343174584757, -21.81201906317816253 ) ) ;
#7856 = CARTESIAN_POINT ( 'NONE',  ( -200.4318156386388523, -14.17468120671733089, -49.29858106685323804 ) ) ;
#7857 = CARTESIAN_POINT ( 'NONE',  ( -77.70139926391286167, 5.508459030575254545, 21.34823270895579839 ) ) ;
#7858 = AXIS2_PLACEMENT_3D ( 'NONE', #23843, #5753, #17463 ) ;
#7859 = ORIENTED_EDGE ( 'NONE', *, *, #7506, .T. ) ;
#7860 = AXIS2_PLACEMENT_3D ( 'NONE', #13138, #9392, #7385 ) ;
#7861 = CARTESIAN_POINT ( 'NONE',  ( 199.9999999999999716, 18.66316687947711728, 3.577466338041057181 ) ) ;
#7862 = CARTESIAN_POINT ( 'NONE',  ( 98.29820294268191105, -7.653668647302824368, -18.47759065022797031 ) ) ;
#7863 = CARTESIAN_POINT ( 'NONE',  ( -4.037857402786239724, 13.82822410908674904, 46.99101396954952037 ) ) ;
#7864 = VERTEX_POINT ( 'NONE', #19362 ) ;
#7865 = VERTEX_POINT ( 'NONE', #17486 ) ;
#7866 = CARTESIAN_POINT ( 'NONE',  ( 184.8905102610680444, -20.92133201514440799, 0.000000000000000000 ) ) ;
#7867 = CARTESIAN_POINT ( 'NONE',  ( 199.0072281836893637, 3.578240568248503894, -19.67355276342582115 ) ) ;
#7868 = CARTESIAN_POINT ( 'NONE',  ( -188.2995950289364941, -43.00522595870984333, 23.44932284465888728 ) ) ;
#7869 = CARTESIAN_POINT ( 'NONE',  ( -97.73860346104962105, -20.56359266935174901, -8.987542150724097567 ) ) ;
#7870 = CARTESIAN_POINT ( 'NONE',  ( 1.564253033640318868, 44.28527310957349528, -24.39614062124454108 ) ) ;
#7871 = CARTESIAN_POINT ( 'NONE',  ( 136.1360204305621266, -3.419521671106983309E-13, 35.03383547441296741 ) ) ;
#7872 = CARTESIAN_POINT ( 'NONE',  ( 200.0000000000001421, -14.29287298608315382, 12.53529920294169386 ) ) ;
#7873 = MECHANICAL_DESIGN_GEOMETRIC_PRESENTATION_REPRESENTATION (  '', ( #16380 ), #24910 ) ;
#7874 = CARTESIAN_POINT ( 'NONE',  ( -626.9846540392142060, 26.45751311064579880, -30.00000000000005329 ) ) ;
#7875 = CIRCLE ( 'NONE', #26183, 30.00000000000000355 ) ;
#7876 = DIRECTION ( 'NONE',  ( 1.357111460130037815E-16, -0.7387770694782699321, 0.6739498806388346530 ) ) ;
#7877 = CARTESIAN_POINT ( 'NONE',  ( 199.0137418305357073, 16.79925839223816197, 10.85573510210755899 ) ) ;
#7878 = CARTESIAN_POINT ( 'NONE',  ( -166.3490444787485387, 12.23457652163751419, 39.29840179234926723 ) ) ;
#7879 = CARTESIAN_POINT ( 'NONE',  ( -3.524834090817713150, -17.92814044289628583, -43.28235980537089489 ) ) ;
#7880 = CARTESIAN_POINT ( 'NONE',  ( -105.3755690713226727, -12.89780903124395550, -12.89780903124416511 ) ) ;
#7881 =( BOUNDED_SURFACE ( )  B_SPLINE_SURFACE ( 3, 3, ( 
 ( #24240, #14121, #12258, #9865, #5610, #26114, #19, #14247, #9997, #1892, #22115, #19975, #16247, #21841, #21977, #19840, #18105, #22249, #1756, #17967, #10265, #26255, #7990, #16110, #3749, #24376, #22387, #2155, #4024, #12124 ),
 ( #23963, #11855, #3610, #20249, #10131, #4164, #2029, #6139, #20381, #1626, #9733, #13716, #18375, #17835, #154, #7722, #15833, #10931, #14637, #22774, #22516, #22905, #6526, #10665, #24905, #2547, #2692, #4555, #4683, #19042 ),
 ( #14775, #16771, #4294, #20640, #10525, #20777, #4418, #10392, #24773, #12652, #18503, #284, #10798, #6660, #12786, #4820, #2416, #16376, #18639, #18908, #6793, #18775, #558, #8527, #12512, #686, #14384, #14512, #6270, #8663 ),
 ( #16908, #22643, #12383, #20913, #8391, #20511, #16513, #422, #8796, #25040, #14905, #16644, #23045, #12923, #21039, #2822, #2283, #8258, #24510, #24639, #6396, #3321, #19541, #17037, #4949, #13055, #11545, #25299, #5446, #15292 ),
 ( #11302, #11421, #8928, #1327, #7423, #5313, #9308, #25172, #13424, #7302, #9432, #13300, #17539, #21547, #15538, #21300, #25677, #23666, #13547, #3075, #21675, #821, #15416, #5197, #6923, #21421, #15040, #19419, #17296, #23422 ),
 ( #3449, #23171, #3193, #1205, #17414, #1074, #7175, #11176, #9183, #19168, #952, #25554, #23542, #21173, #2946, #11056, #15172, #9060, #17165, #7057, #23297, #5074, #13179, #19291, #25428, #26076, #1587, #11676, #25806, #17664 ),
 ( #14451, #15928, #16070, #4483, #7812, #25941, #26216, #1855, #15665, #5697, #21937, #5837, #15797, #21800, #9827, #24061, #3573, #19801, #22578, #9958, #18065, #16577, #13802, #1456, #3713, #4357, #18574, #13941, #22076, #19934 ) ),
 .UNSPECIFIED., .T., .F., .F. ) 
 B_SPLINE_SURFACE_WITH_KNOTS ( ( 4, 3, 4 ),
 ( 4, 2, 2, 2, 2, 2, 2, 2, 2, 2, 2, 2, 2, 2, 4 ),
 ( 0.000000000000000000, 0.5000000000000000000, 1.000000000000000000 ),
 ( 0.000000000000000000, 0.1357259735107005372, 0.1651108541090157700, 0.1944957347073310028, 0.3598804999793158710, 0.3867117631979620773, 0.4135430264166082281, 0.5789277916885930964, 0.6062785021374117456, 0.6336292125862302838, 0.8508620842112317728, 0.8814014469398914198, 0.9119408096685510667, 0.9559704048342755334, 1.000000000000000000 ),
 .UNSPECIFIED. ) 
 GEOMETRIC_REPRESENTATION_ITEM ( )  RATIONAL_B_SPLINE_SURFACE ( (
 ( 1.000000000000000000, 1.000000000000000000, 1.000000000000000000, 1.000000000000000000, 1.000000000000000000, 1.000000000000000000, 1.000000000000000000, 1.000000000000000000, 1.000000000000000000, 1.000000000000000000, 1.000000000000000000, 1.000000000000000000, 1.000000000000000000, 1.000000000000000000, 1.000000000000000000, 1.000000000000000000, 1.000000000000000000, 1.000000000000000000, 1.000000000000000000, 1.000000000000000000, 1.000000000000000000, 1.000000000000000000, 1.000000000000000000, 1.000000000000000000, 1.000000000000000000, 1.000000000000000000, 1.000000000000000000, 1.000000000000000000, 1.000000000000000000, 1.000000000000000000),
 ( 0.3333333333333333703, 0.3333333333333333703, 0.3333333333333333703, 0.3333333333333333703, 0.3333333333333333703, 0.3333333333333333703, 0.3333333333333333703, 0.3333333333333333703, 0.3333333333333333703, 0.3333333333333333703, 0.3333333333333333703, 0.3333333333333333703, 0.3333333333333333703, 0.3333333333333333703, 0.3333333333333333703, 0.3333333333333333703, 0.3333333333333333703, 0.3333333333333333703, 0.3333333333333333703, 0.3333333333333333703, 0.3333333333333333703, 0.3333333333333333703, 0.3333333333333333703, 0.3333333333333333703, 0.3333333333333333703, 0.3333333333333333703, 0.3333333333333333703, 0.3333333333333333703, 0.3333333333333333703, 0.3333333333333333703),
 ( 0.3333333333333333703, 0.3333333333333333703, 0.3333333333333333703, 0.3333333333333333703, 0.3333333333333333703, 0.3333333333333333703, 0.3333333333333333703, 0.3333333333333333703, 0.3333333333333333703, 0.3333333333333333703, 0.3333333333333333703, 0.3333333333333333703, 0.3333333333333333703, 0.3333333333333333703, 0.3333333333333333703, 0.3333333333333333703, 0.3333333333333333703, 0.3333333333333333703, 0.3333333333333333703, 0.3333333333333333703, 0.3333333333333333703, 0.3333333333333333703, 0.3333333333333333703, 0.3333333333333333703, 0.3333333333333333703, 0.3333333333333333703, 0.3333333333333333703, 0.3333333333333333703, 0.3333333333333333703, 0.3333333333333333703),
 ( 1.000000000000000000, 1.000000000000000000, 1.000000000000000000, 1.000000000000000000, 1.000000000000000000, 1.000000000000000000, 1.000000000000000000, 1.000000000000000000, 1.000000000000000000, 1.000000000000000000, 1.000000000000000000, 1.000000000000000000, 1.000000000000000000, 1.000000000000000000, 1.000000000000000000, 1.000000000000000000, 1.000000000000000000, 1.000000000000000000, 1.000000000000000000, 1.000000000000000000, 1.000000000000000000, 1.000000000000000000, 1.000000000000000000, 1.000000000000000000, 1.000000000000000000, 1.000000000000000000, 1.000000000000000000, 1.000000000000000000, 1.000000000000000000, 1.000000000000000000),
 ( 0.3333333333333333703, 0.3333333333333333703, 0.3333333333333333703, 0.3333333333333333703, 0.3333333333333333703, 0.3333333333333333703, 0.3333333333333333703, 0.3333333333333333703, 0.3333333333333333703, 0.3333333333333333703, 0.3333333333333333703, 0.3333333333333333703, 0.3333333333333333703, 0.3333333333333333703, 0.3333333333333333703, 0.3333333333333333703, 0.3333333333333333703, 0.3333333333333333703, 0.3333333333333333703, 0.3333333333333333703, 0.3333333333333333703, 0.3333333333333333703, 0.3333333333333333703, 0.3333333333333333703, 0.3333333333333333703, 0.3333333333333333703, 0.3333333333333333703, 0.3333333333333333703, 0.3333333333333333703, 0.3333333333333333703),
 ( 0.3333333333333333703, 0.3333333333333333703, 0.3333333333333333703, 0.3333333333333333703, 0.3333333333333333703, 0.3333333333333333703, 0.3333333333333333703, 0.3333333333333333703, 0.3333333333333333703, 0.3333333333333333703, 0.3333333333333333703, 0.3333333333333333703, 0.3333333333333333703, 0.3333333333333333703, 0.3333333333333333703, 0.3333333333333333703, 0.3333333333333333703, 0.3333333333333333703, 0.3333333333333333703, 0.3333333333333333703, 0.3333333333333333703, 0.3333333333333333703, 0.3333333333333333703, 0.3333333333333333703, 0.3333333333333333703, 0.3333333333333333703, 0.3333333333333333703, 0.3333333333333333703, 0.3333333333333333703, 0.3333333333333333703),
 ( 1.000000000000000000, 1.000000000000000000, 1.000000000000000000, 1.000000000000000000, 1.000000000000000000, 1.000000000000000000, 1.000000000000000000, 1.000000000000000000, 1.000000000000000000, 1.000000000000000000, 1.000000000000000000, 1.000000000000000000, 1.000000000000000000, 1.000000000000000000, 1.000000000000000000, 1.000000000000000000, 1.000000000000000000, 1.000000000000000000, 1.000000000000000000, 1.000000000000000000, 1.000000000000000000, 1.000000000000000000, 1.000000000000000000, 1.000000000000000000, 1.000000000000000000, 1.000000000000000000, 1.000000000000000000, 1.000000000000000000, 1.000000000000000000, 1.000000000000000000) ) ) 
 REPRESENTATION_ITEM ( '' )  SURFACE ( )  );
#7882 = CARTESIAN_POINT ( 'NONE',  ( -200.0000000000000284, 15.65821854886104880, 47.96425349429443941 ) ) ;
#7883 = CARTESIAN_POINT ( 'NONE',  ( -30.26275506840322649, -29.48230279907810925, 29.48230279907778950 ) ) ;
#7884 = CARTESIAN_POINT ( 'NONE',  ( 146.6084372240433993, -3.357462877844280890E-13, 34.62501878078305850 ) ) ;
#7885 = CARTESIAN_POINT ( 'NONE',  ( 91.82158438592158234, 12.16597498397756993, 12.16597498397776356 ) ) ;
#7886 = CARTESIAN_POINT ( 'NONE',  ( 151.7948205124836534, -6.767089262349006873, 40.00000000000002132 ) ) ;
#7887 = AXIS2_PLACEMENT_3D ( 'NONE', #303, #10950, #6677 ) ;
#7888 = CARTESIAN_POINT ( 'NONE',  ( -716.9846540392142060, -52.49999999999991473, 82.49999999999998579 ) ) ;
#7889 = CARTESIAN_POINT ( 'NONE',  ( 130.8568914410475088, -5.949712681206664300, -40.00000000000002132 ) ) ;
#7890 = CARTESIAN_POINT ( 'NONE',  ( -114.6336192494810575, 11.25681893587175608, 18.90533938101397737 ) ) ;
#7891 = VECTOR ( 'NONE', #1462, 1000.000000000000000 ) ;
#7892 = CARTESIAN_POINT ( 'NONE',  ( 163.1118516004056573, 40.00000000000017764, -12.73709011382432976 ) ) ;
#7893 = CARTESIAN_POINT ( 'NONE',  ( -100.7734535825088358, -16.03295912088706743, -16.03295912088710296 ) ) ;
#7894 = CARTESIAN_POINT ( 'NONE',  ( 19.06497207195980792, 14.19242893257840699, -40.00000000000002132 ) ) ;
#7895 = ORIENTED_EDGE ( 'NONE', *, *, #3211, .T. ) ;
#7896 = CARTESIAN_POINT ( 'NONE',  ( 23.38399212876581146, -42.85408588822665621, 23.33762193384644590 ) ) ;
#7897 = CIRCLE ( 'NONE', #4548, 30.00000000000003908 ) ;
#7898 = DIRECTION ( 'NONE',  ( -1.000000000000000000, -1.836970198721030181E-16, -0.000000000000000000 ) ) ;
#7899 = CARTESIAN_POINT ( 'NONE',  ( 19.06497207195979726, 38.31983398719629719, -18.24870850772750686 ) ) ;
#7900 = CARTESIAN_POINT ( 'NONE',  ( 130.8568914410475088, -40.00000000000001421, 5.949712681206549725 ) ) ;
#7901 = CARTESIAN_POINT ( 'NONE',  ( -135.8532207217289738, 21.81201906317729566, 34.75652343174635917 ) ) ;
#7902 = CARTESIAN_POINT ( 'NONE',  ( -100.7734535825088358, -22.67402823373193499, 0.000000000000000000 ) ) ;
#7903 = CARTESIAN_POINT ( 'NONE',  ( 130.8568914410475088, 5.949712681206719367, -40.00000000000002132 ) ) ;
#7904 = DIRECTION ( 'NONE',  ( 1.000000000000000000, 1.836970198721030181E-16, 0.000000000000000000 ) ) ;
#7905 = CARTESIAN_POINT ( 'NONE',  ( 200.0000000000000853, 18.51119012207909620, 4.337730402235636440 ) ) ;
#7906 = CARTESIAN_POINT ( 'NONE',  ( 199.9999999999999147, -15.18276431615445610, 11.44766049767000915 ) ) ;
#7907 = CARTESIAN_POINT ( 'NONE',  ( -105.3755690713226727, 12.89780903124418998, -12.89780903124389155 ) ) ;
#7908 = CARTESIAN_POINT ( 'NONE',  ( 200.0000000000000000, -42.42640687119290988, 14.14213562373064903 ) ) ;
#7909 = EDGE_CURVE ( 'NONE', #17301, #6965, #2892, .T. ) ;
#7910 = CARTESIAN_POINT ( 'NONE',  ( 199.9999999999999432, 14.14213562373113398, -14.14213562373094923 ) ) ;
#7911 = CARTESIAN_POINT ( 'NONE',  ( -86.86493150571119770, 19.60045294882776901, -8.366608963953506617 ) ) ;
#7912 = CARTESIAN_POINT ( 'NONE',  ( -259.2033419157646676, -49.83842185052040463, 6.730120644403092101 ) ) ;
#7913 = DIRECTION ( 'NONE',  ( 0.000000000000000000, 0.3028247695821862928, -0.9530462522498558409 ) ) ;
#7914 = CARTESIAN_POINT ( 'NONE',  ( -30.26275506840324070, 1.198031551616030033, -1.198031551616006496 ) ) ;
#7915 = CARTESIAN_POINT ( 'NONE',  ( 151.7948205124835681, -4.785054706298153882, -51.78348778862540058 ) ) ;
#7916 = B_SPLINE_CURVE_WITH_KNOTS ( 'NONE', 3,
 ( #14009, #24265, #14275, #2307, #10021, #10415 ),
 .UNSPECIFIED., .F., .F.,
 ( 4, 2, 4 ),
 ( 0.000000000000000000, 0.004167651203541847087, 0.008335302407083694173 ),
 .UNSPECIFIED. ) ;
#7917 = CARTESIAN_POINT ( 'NONE',  ( 199.0224155992051180, 2.400915676194647741, 19.86821540553048848 ) ) ;
#7919 = CARTESIAN_POINT ( 'NONE',  ( -259.2033419157646676, -40.00000000000003553, -9.517827891722768996 ) ) ;
#7918 = CARTESIAN_POINT ( 'NONE',  ( -56.48582580120559982, -6.472252184283581400, -50.09629031063973059 ) ) ;
#7920 = CARTESIAN_POINT ( 'NONE',  ( 192.4448373802101173, 42.42640687122070631, 14.14213562370331623 ) ) ;
#7921 = CARTESIAN_POINT ( 'NONE',  ( -30.26275506840324070, -1.198031551616016266, -1.198031551616031587 ) ) ;
#7922 = CARTESIAN_POINT ( 'NONE',  ( -4.201409602818262812, 46.93439176590655393, -13.81669219312473906 ) ) ;
#7923 = CARTESIAN_POINT ( 'NONE',  ( 170.2234770963711128, -24.55285855007184281, 40.00000000000002132 ) ) ;
#7924 = ORIENTED_EDGE ( 'NONE', *, *, #20019, .F. ) ;
#7925 = CARTESIAN_POINT ( 'NONE',  ( -30.26275506840324070, 1.198031551616013601, 1.198031551616023371 ) ) ;
#7926 = AXIS2_PLACEMENT_3D ( 'NONE', #15349, #11227, #9104 ) ;
#7927 = CARTESIAN_POINT ( 'NONE',  ( 29.55251326303118375, 40.53812068415412995, 16.79143938049396567 ) ) ;
#7928 = B_SPLINE_CURVE_WITH_KNOTS ( 'NONE', 3,
 ( #23551, #23178, #19550, #7184, #2954, #11064 ),
 .UNSPECIFIED., .F., .F.,
 ( 4, 2, 4 ),
 ( -5.998616615737899812E-08, 0.005994953700759804265, 0.01198996738768576611 ),
 .UNSPECIFIED. ) ;
#7929 = LINE ( 'NONE', #12059, #19617 ) ;
#7930 = CARTESIAN_POINT ( 'NONE',  ( -259.2033419157646676, -9.517827891722680178, 0.000000000000000000 ) ) ;
#7931 = ORIENTED_EDGE ( 'NONE', *, *, #3619, .T. ) ;
#7932 = CARTESIAN_POINT ( 'NONE',  ( -348.0000000000001137, -4.467814962633844109E-14, -31.79780246617542616 ) ) ;
#7933 = CARTESIAN_POINT ( 'NONE',  ( 200.0000000000001421, -15.08701489606589341, 11.56722645162647467 ) ) ;
#7934 = CARTESIAN_POINT ( 'NONE',  ( 11.71430589694271340, -14.17293196763458596, 49.28686712666256398 ) ) ;
#7935 = CARTESIAN_POINT ( 'NONE',  ( 23.84827734669562460, 23.24317830786175421, -42.71123329578252026 ) ) ;
#7936 = CARTESIAN_POINT ( 'NONE',  ( 199.0117582043400830, -7.359043231587310885, -18.59750019459799120 ) ) ;
#7937 = CARTESIAN_POINT ( 'NONE',  ( 190.0000000000000000, 71.50000000000009948, -66.50000000000005684 ) ) ;
#7938 = CARTESIAN_POINT ( 'NONE',  ( -187.8779108535583191, -17.82355704115829553, 43.02987313850725570 ) ) ;
#7939 = CARTESIAN_POINT ( 'NONE',  ( 0.2972598230769907257, 66.70487387989869887, -10.13633138497392494 ) ) ;
#7940 = CARTESIAN_POINT ( 'NONE',  ( -87.13361725327072804, 8.813415818526478339E-15, 21.49321519333429009 ) ) ;
#7942 = CARTESIAN_POINT ( 'NONE',  ( 199.9999999999999432, -14.14213562373115884, 14.14213562373085153 ) ) ;
#7941 = CARTESIAN_POINT ( 'NONE',  ( -187.7699188115598474, 13.79076593539120310, -46.80708926515250567 ) ) ;
#7943 = CARTESIAN_POINT ( 'NONE',  ( 98.29820294267528880, -14.14213562373450017, -14.14213562373441668 ) ) ;
#7944 = CARTESIAN_POINT ( 'NONE',  ( -280.0000000000000568, -20.00000000000006395, -40.00000000000002132 ) ) ;
#7945 = CARTESIAN_POINT ( 'NONE',  ( -162.0762913951020892, 1.694272876828294194, 0.000000000000000000 ) ) ;
#7946 = CARTESIAN_POINT ( 'NONE',  ( -162.0762913951020892, -39.99999999999961631, -41.69427287692722928 ) ) ;
#7947 = CARTESIAN_POINT ( 'NONE',  ( -280.0000000000000568, 42.42640687119285303, -14.14213562373088351 ) ) ;
#7948 = CARTESIAN_POINT ( 'NONE',  ( 190.0000000000000000, -69.99999999999987210, 8.572527594031463526E-15 ) ) ;
#7949 = CARTESIAN_POINT ( 'NONE',  ( -135.8532207217289738, 34.75652343174625258, -21.81201906317744132 ) ) ;
#7950 = VERTEX_POINT ( 'NONE', #17233 ) ;
#7951 = CARTESIAN_POINT ( 'NONE',  ( -280.0000000000000568, -42.42640687119295251, 14.14213562373088351 ) ) ;
#7952 = DIRECTION ( 'NONE',  ( 1.000000000000000000, -1.836970198721030181E-16, -0.000000000000000000 ) ) ;
#7953 = CARTESIAN_POINT ( 'NONE',  ( -626.9846540392142060, 95.00000000000000000, 0.000000000000000000 ) ) ;
#7954 = SHAPE_DEFINITION_REPRESENTATION ( #23973, #12169 ) ;
#7955 = ORIENTED_EDGE ( 'NONE', *, *, #21219, .T. ) ;
#7956 = VERTEX_POINT ( 'NONE', #6992 ) ;
#7957 = CARTESIAN_POINT ( 'NONE',  ( 91.82158438592156813, -16.11829626348402655, -40.45024623143966380 ) ) ;
#7958 = CARTESIAN_POINT ( 'NONE',  ( 25.88393124173831339, -45.90075965690534332, -13.61573025393274072 ) ) ;
#7959 = ORIENTED_EDGE ( 'NONE', *, *, #26226, .T. ) ;
#7960 = CARTESIAN_POINT ( 'NONE',  ( -238.4067589809705794, 0.9644942799825386714, 0.000000000000000000 ) ) ;
#7961 = CARTESIAN_POINT ( 'NONE',  ( -93.01741312762746361, -20.50009083233623386, 8.946232117507843640 ) ) ;
#7962 = ORIENTED_EDGE ( 'NONE', *, *, #6706, .F. ) ;
#7963 = CARTESIAN_POINT ( 'NONE',  ( 199.9999999999999147, 6.094537134382843391, 18.00666549647224812 ) ) ;
#7964 = DIRECTION ( 'NONE',  ( 1.000000000000000000, 1.836970198721030427E-16, -0.000000000000000000 ) ) ;
#7965 = CARTESIAN_POINT ( 'NONE',  ( -162.0762913951020892, 1.198031840385716418, 1.198031840385750169 ) ) ;
#7966 = CARTESIAN_POINT ( 'NONE',  ( -188.2957210513884831, -46.98905903629623282, -13.82790368522444169 ) ) ;
#7967 = CARTESIAN_POINT ( 'NONE',  ( 170.2234770963711128, -40.00000000000004263, 15.44714144992801685 ) ) ;
#7968 = CARTESIAN_POINT ( 'NONE',  ( 200.0000000000000000, -20.00000000000006750, 40.00000000000002132 ) ) ;
#7969 = CARTESIAN_POINT ( 'NONE',  ( -162.0762913951020892, 29.48230308784799902, -29.48230308784730980 ) ) ;
#7970 = CARTESIAN_POINT ( 'NONE',  ( 199.0228608363770206, 1.289830063590766907, 19.96444201077071057 ) ) ;
#7971 = APPLICATION_CONTEXT ( 'automotive_design' ) ;
#7972 = CARTESIAN_POINT ( 'NONE',  ( -135.8532207217289738, -40.00000000000014921, 30.84685318188631697 ) ) ;
#7973 = CARTESIAN_POINT ( 'NONE',  ( 136.1360204305621266, 5.219216885335291329E-15, 4.966164525587064560 ) ) ;
#7974 = CARTESIAN_POINT ( 'NONE',  ( -259.2033419157646676, -1.473088368616265084E-13, 9.517827891722632216 ) ) ;
#7975 = CARTESIAN_POINT ( 'NONE',  ( -110.0947178154763719, -15.96121929952994378, 12.38433105677422574 ) ) ;
#7976 = CARTESIAN_POINT ( 'NONE',  ( 0.2972598230770153171, -66.70487387989861361, 10.13633138497438324 ) ) ;
#7977 = CARTESIAN_POINT ( 'NONE',  ( -30.26275506840324425, -1.694272468446265334, -40.00000000000002132 ) ) ;
#7978 = CARTESIAN_POINT ( 'NONE',  ( -162.0762913951021176, -29.48230308784755493, -27.08623940707632372 ) ) ;
#7979 = CARTESIAN_POINT ( 'NONE',  ( -103.9474983245025044, -8.577167319634718012, 19.92928099173747114 ) ) ;
#7980 = CARTESIAN_POINT ( 'NONE',  ( 21.15737826136109589, -47.57244852138556013, 13.91467835516659513 ) ) ;
#7981 = CARTESIAN_POINT ( 'NONE',  ( -198.0356074513804572, 40.00000000000014921, -15.37879056873028816 ) ) ;
#7982 = CARTESIAN_POINT ( 'NONE',  ( -280.0000000000000000, 1.839446121267387017E-14, -20.00000000000001421 ) ) ;
#7983 = CARTESIAN_POINT ( 'NONE',  ( -198.0356074513804572, 67.44298959253333692, 10.87444709760969452 ) ) ;
#7984 = CARTESIAN_POINT ( 'NONE',  ( -238.4067589809705794, -0.6820004457913585449, -0.6820004457913265705 ) ) ;
#7985 = CARTESIAN_POINT ( 'NONE',  ( -188.8532066752252376, -17.93248812771238221, -43.29285604501852447 ) ) ;
#7986 = CARTESIAN_POINT ( 'NONE',  ( -135.8532207217289738, 6.472252184284186249, -6.472252184284142729 ) ) ;
#7987 = VERTEX_POINT ( 'NONE', #6734 ) ;
#7988 = CARTESIAN_POINT ( 'NONE',  ( 19.06497207195980792, 10.03556273973447155, -10.03556273973422286 ) ) ;
#7989 = CARTESIAN_POINT ( 'NONE',  ( -200.0000000000000000, 52.49999999999988631, -82.49999999999998579 ) ) ;
#7990 = CARTESIAN_POINT ( 'NONE',  ( 136.1360204305621266, 35.03383547441298873, 0.000000000000000000 ) ) ;
#7991 = EDGE_CURVE ( 'NONE', #2026, #15674, #12559, .T. ) ;
#7992 = SURFACE_STYLE_USAGE ( .BOTH. , #20382 ) ;
#7993 = CARTESIAN_POINT ( 'NONE',  ( -208.1127848780264742, 10.60833733268383483, -67.17687982760675425 ) ) ;
#7994 = CARTESIAN_POINT ( 'NONE',  ( 0.000000000000000000, 0.000000000000000000, 0.000000000000000000 ) ) ;
#7995 = CARTESIAN_POINT ( 'NONE',  ( -626.9846540392097722, 90.00000000000000000, 59.99999999999999289 ) ) ;
#7996 = ORIENTED_EDGE ( 'NONE', *, *, #3959, .T. ) ;
#7997 = CARTESIAN_POINT ( 'NONE',  ( 199.9999999999999432, 17.99246019556983711, 6.122134764576554034 ) ) ;
#7998 = CARTESIAN_POINT ( 'NONE',  ( 73.43438336400350863, -9.843172575685745329, -28.18283891303412858 ) ) ;
#7999 = EDGE_CURVE ( 'NONE', #1453, #8799, #15107, .T. ) ;
#8000 = CARTESIAN_POINT ( 'NONE',  ( -4.915070467882389771, 23.27857837408975783, 42.74707758271485858 ) ) ;
#8001 = ORIENTED_EDGE ( 'NONE', *, *, #18091, .F. ) ;
#8002 = VERTEX_POINT ( 'NONE', #25373 ) ;
#8003 = CARTESIAN_POINT ( 'NONE',  ( 184.8905102610680444, -20.92133201514440799, -40.00000000000002132 ) ) ;
#8004 = CARTESIAN_POINT ( 'NONE',  ( 199.0095093599360894, -2.612260778589423182, -19.82812366214328748 ) ) ;
#8005 = CARTESIAN_POINT ( 'NONE',  ( -114.6375327213287818, 5.510795915284336211, 21.34761811097288486 ) ) ;
#8006 = EDGE_CURVE ( 'NONE', #22119, #2384, #14846, .T. ) ;
#8007 = ADVANCED_FACE ( 'NONE', ( #5018 ), #3267, .T. ) ;
#8008 = CARTESIAN_POINT ( 'NONE',  ( 73.43438336401153776, 28.18283891303104483, -9.843172575685235515 ) ) ;
#8009 = CIRCLE ( 'NONE', #16080, 15.00000000000000000 ) ;
#8010 = CARTESIAN_POINT ( 'NONE',  ( -89.91498783730708055, -8.733585467785214718, -20.17141720495975576 ) ) ;
#8011 = CARTESIAN_POINT ( 'NONE',  ( -198.0356074513804572, 40.00000000000014921, -15.37879056873028816 ) ) ;
#8012 = DIRECTION ( 'NONE',  ( 1.000000000000000000, -1.937599346585394162E-16, -0.000000000000000000 ) ) ;
#8013 = CARTESIAN_POINT ( 'NONE',  ( -77.55640685876512919, -22.13135000837101529, -2.449293598294708880E-15 ) ) ;
#8014 = DIRECTION ( 'NONE',  ( -1.000000000000000000, 0.000000000000000000, 0.000000000000000000 ) ) ;
#8015 = CARTESIAN_POINT ( 'NONE',  ( 199.0248237628271113, -4.554872532684343334, 19.47958378538321611 ) ) ;
#8016 = DIRECTION ( 'NONE',  ( -0.2259624731720487056, 0.9741360072997872210, 0.000000000000000000 ) ) ;
#8017 = CARTESIAN_POINT ( 'NONE',  ( -4.439300432586843037, -13.79990882516970352, -46.85201324744510742 ) ) ;
#8018 = CARTESIAN_POINT ( 'NONE',  ( -208.1127848780264742, -38.89260858015704514, -38.89260858015768463 ) ) ;
#8019 = CARTESIAN_POINT ( 'NONE',  ( -4.039451493210485467, -13.82811171175474207, 46.99046209229799587 ) ) ;
#8020 = CARTESIAN_POINT ( 'NONE',  ( -56.48582580120558561, -50.09629031063963112, -6.472252184284449150 ) ) ;
#8021 = CARTESIAN_POINT ( 'NONE',  ( 91.82158438592158234, -1.633484621919921769E-13, 17.20528682183300262 ) ) ;
#8022 = CARTESIAN_POINT ( 'NONE',  ( 57.59792236341147031, 1.722363176415040886, 1.722363176415060426 ) ) ;
#8023 = CARTESIAN_POINT ( 'NONE',  ( -162.0762913951020607, -41.69427287692683848, 40.00000000000002132 ) ) ;
#8024 = CARTESIAN_POINT ( 'NONE',  ( 160.7895100361087657, 20.14405787076037413, -20.14405787076013254 ) ) ;
#8025 = CARTESIAN_POINT ( 'NONE',  ( 151.7948205124836250, -6.767089262349004208, -2.449293598294708485E-15 ) ) ;
#8026 = CARTESIAN_POINT ( 'NONE',  ( -114.4954523681517458, 9.313731507797939457, 19.81404414622909016 ) ) ;
#8027 = CARTESIAN_POINT ( 'NONE',  ( -56.48582580120559982, 40.00000000000034106, -30.84685318188602210 ) ) ;
#8028 = CARTESIAN_POINT ( 'NONE',  ( -105.3755690713226727, -15.38646221621786481, -15.38646221621789856 ) ) ;
#8029 = CARTESIAN_POINT ( 'NONE',  ( 57.59792236341147031, -2.435789363418150444, 0.000000000000000000 ) ) ;
#8030 = ORIENTED_EDGE ( 'NONE', *, *, #26271, .T. ) ;
#8031 = VERTEX_POINT ( 'NONE', #1272 ) ;
#8032 = CARTESIAN_POINT ( 'NONE',  ( 0.2972598230769930017, 14.33493731733933352, 40.00000000000002132 ) ) ;
#8033 = AXIS2_PLACEMENT_3D ( 'NONE', #19816, #23556, #7568 ) ;
#8034 = CARTESIAN_POINT ( 'NONE',  ( -96.93773665438791909, -8.190703376740877673, -20.92028269119433403 ) ) ;
#8035 = CARTESIAN_POINT ( 'NONE',  ( -105.3755690713226727, -8.549198663894545631E-14, 18.24025645688352881 ) ) ;
#8036 = CARTESIAN_POINT ( 'NONE',  ( -259.2033419157646676, -6.730120644403663199, 6.730120644403451813 ) ) ;
#8037 = CARTESIAN_POINT ( 'NONE',  ( -200.0000000000000000, 0.000000000000000000, 0.000000000000000000 ) ) ;
#8038 = CARTESIAN_POINT ( 'NONE',  ( -188.5332406156555010, -43.07394490460117709, -23.50029615581455644 ) ) ;
#8039 =( BOUNDED_SURFACE ( )  B_SPLINE_SURFACE ( 3, 2, ( 
 ( #17122, #905, #3405 ),
 ( #11506, #7516, #15624 ),
 ( #7004, #15124, #23255 ),
 ( #21257, #1033, #9133 ),
 ( #14169, #16165, #5793 ),
 ( #1945, #11634, #17886 ),
 ( #25897, #15887, #13901 ),
 ( #13764, #22034, #15753 ),
 ( #3807, #11912, #18289 ),
 ( #21891, #20034, #1812 ),
 ( #9915, #24015, #1679 ),
 ( #23881, #18021, #8048 ),
 ( #11776, #26170, #16301 ),
 ( #10052, #7772, #8184 ),
 ( #9651, #12180, #3534 ),
 ( #24154, #22302, #7911 ) ),
 .UNSPECIFIED., .F., .F., .F. ) 
 B_SPLINE_SURFACE_WITH_KNOTS ( ( 4, 2, 2, 2, 2, 2, 2, 4 ),
 ( 3, 3 ),
 ( 0.04143342415445357141, 0.04844559399082577766, 0.05195167890901188079, 0.05545776382719797698, 0.06246993366357017630, 0.06422297612266322786, 0.06597601858175627942, 0.06948210349994238255 ),
 ( 0.000000000000000000, 1.000000000000000000 ),
 .UNSPECIFIED. ) 
 GEOMETRIC_REPRESENTATION_ITEM ( )  RATIONAL_B_SPLINE_SURFACE ( (
 ( 1.000000000000000000, 0.9541700779530604137, 1.000000000000000000),
 ( 1.000000000000000000, 0.9520168980299437145, 1.000000000000000000),
 ( 1.000000000000000000, 0.9503263051600997491, 1.000000000000000000),
 ( 1.000000000000000000, 0.9485964699097189090, 1.000000000000000000),
 ( 1.000000000000000000, 0.9481599523400192631, 1.000000000000000000),
 ( 1.000000000000000000, 0.9475783919167657388, 1.000000000000000000),
 ( 1.000000000000000000, 0.9474332805886016562, 1.000000000000000000),
 ( 1.000000000000000000, 0.9474385816642081348, 1.000000000000000000),
 ( 1.000000000000000000, 0.9480200071122316663, 1.000000000000000000),
 ( 1.000000000000000000, 0.9494436219491265705, 1.000000000000000000),
 ( 1.000000000000000000, 0.9497633688929369988, 1.000000000000000000),
 ( 1.000000000000000000, 0.9504729676351979517, 1.000000000000000000),
 ( 1.000000000000000000, 0.9508638236297854984, 1.000000000000000000),
 ( 1.000000000000000000, 0.9521268919818318688, 1.000000000000000000),
 ( 1.000000000000000000, 0.9530924015899474577, 1.000000000000000000),
 ( 1.000000000000000000, 0.9541700779530456478, 1.000000000000000000) ) ) 
 REPRESENTATION_ITEM ( '' )  SURFACE ( )  );
#8040 = PRODUCT_DEFINITION_SHAPE ( 'NONE', 'NONE',  #17594 ) ;
#8041 = DIRECTION ( 'NONE',  ( 0.01051738792037396585, -0.9307051272719674140, 0.3656191332808000904 ) ) ;
#8042 = CARTESIAN_POINT ( 'NONE',  ( 200.0000000000000568, 16.12943746570313053, 10.05448153537135347 ) ) ;
#8043 = UNCERTAINTY_MEASURE_WITH_UNIT (LENGTH_MEASURE( 1.000000000000000082E-05 ), #13101, 'distance_accuracy_value', 'NONE');
#8044 = CARTESIAN_POINT ( 'NONE',  ( 199.9999999999999432, -15.98279859272680170, -10.29025366354621696 ) ) ;
#8045 = CARTESIAN_POINT ( 'NONE',  ( 136.1360204305621266, 3.511608612530757068, -3.511608612530642937 ) ) ;
#8046 = CARTESIAN_POINT ( 'NONE',  ( -30.26275506840322294, -57.76657404653985139, -1.198031551616531853 ) ) ;
#8047 = CARTESIAN_POINT ( 'NONE',  ( -114.4008591471760923, 20.10521893440135699, 8.440277345772122075 ) ) ;
#8048 = CARTESIAN_POINT ( 'NONE',  ( -87.01506749150125586, 18.46228859042466652, -10.84947533657426000 ) ) ;
#8049 = CARTESIAN_POINT ( 'NONE',  ( -213.1075012329537230, -66.26714140136188291, -9.698598906438677503 ) ) ;
#8050 = DIRECTION ( 'NONE',  ( 0.000000000000000000, 0.000000000000000000, 1.000000000000000000 ) ) ;
#8051 = CARTESIAN_POINT ( 'NONE',  ( 200.0000000000000000, -14.14213562373046784, -42.42640687119298804 ) ) ;
#8052 = CARTESIAN_POINT ( 'NONE',  ( -208.1127848780264742, -67.17687982763172272, 10.60833733270744617 ) ) ;
#8053 = CARTESIAN_POINT ( 'NONE',  ( -114.4364955367327497, -20.04994829327637262, -8.644468109209869411 ) ) ;
#8054 = CIRCLE ( 'NONE', #423, 5.000000000000004441 ) ;
#8056 = CARTESIAN_POINT ( 'NONE',  ( 136.1360204305621551, 40.00000000000002842, 4.966164525587208445 ) ) ;
#8055 = CARTESIAN_POINT ( 'NONE',  ( -91.56559293963834989, 12.25131212657497848, -12.25131212657469426 ) ) ;
#8057 = CARTESIAN_POINT ( 'NONE',  ( -30.26275506840324070, 1.198031551616030033, -1.198031551616006496 ) ) ;
#8058 = CARTESIAN_POINT ( 'NONE',  ( 22.17571259162450303, 43.20787961118990950, -23.59965736304651784 ) ) ;
#8059 = CARTESIAN_POINT ( 'NONE',  ( 4.995406935893289102, 55.24977328856464709, -40.00000000000002132 ) ) ;
#8060 = ORIENTED_EDGE ( 'NONE', *, *, #4040, .T. ) ;
#8061 = CARTESIAN_POINT ( 'NONE',  ( -192.9588430854689989, 14.46834944099965981, 0.000000000000000000 ) ) ;
#8062 = CARTESIAN_POINT ( 'NONE',  ( -77.90255099906765679, -20.29001641120677846, 8.064892378658099048 ) ) ;
#8063 = DIRECTION ( 'NONE',  ( 1.000000000000000000, 1.836970198721030181E-16, 0.000000000000000000 ) ) ;
#8064 = ORIENTED_EDGE ( 'NONE', *, *, #10595, .T. ) ;
#8065 = CARTESIAN_POINT ( 'NONE',  ( -192.6562840317106691, -44.11756026581168300, 18.27409180090121410 ) ) ;
#8066 = CARTESIAN_POINT ( 'NONE',  ( 199.9999999999999716, -17.78976893299991247, -6.695511796223322598 ) ) ;
#8067 = ADVANCED_FACE ( 'NONE', ( #20980 ), #10867, .T. ) ;
#8068 = CARTESIAN_POINT ( 'NONE',  ( 21.80484139881139782, -17.98806631652405486, 43.42703366220045780 ) ) ;
#8069 = CARTESIAN_POINT ( 'NONE',  ( 23.72853009152708736, 13.77482773664671711, -46.68009952139264840 ) ) ;
#8070 = CARTESIAN_POINT ( 'NONE',  ( 199.0106728332879698, -5.188592077825961546, -19.31531804097554073 ) ) ;
#8071 = CARTESIAN_POINT ( 'NONE',  ( 23.37394308801977871, -13.80096434448300613, 46.80823611210190904 ) ) ;
#8072 = LINE ( 'NONE', #7797, #25352 ) ;
#8073 = CARTESIAN_POINT ( 'NONE',  ( -726.9846540392142060, -52.49999999999972999, -82.49999999999998579 ) ) ;
#8074 = CARTESIAN_POINT ( 'NONE',  ( 146.6084372240433993, 3.800685668858732935, -3.800685668858610367 ) ) ;
#8075 = CARTESIAN_POINT ( 'NONE',  ( 19.06497207195981503, -14.19242893257840166, 0.000000000000000000 ) ) ;
#8077 = CARTESIAN_POINT ( 'NONE',  ( 19.06497207195980792, 10.03556273973447155, -10.03556273973422286 ) ) ;
#8076 = CARTESIAN_POINT ( 'NONE',  ( -194.4222169614336622, 24.44978956118432123, -44.35789444896231259 ) ) ;
#8078 = FACE_OUTER_BOUND ( 'NONE', #8667, .T. ) ;
#8079 = EDGE_CURVE ( 'NONE', #16477, #15766, #23515, .T. ) ;
#8080 = CARTESIAN_POINT ( 'NONE',  ( -56.48582580120557850, -30.84685318188645198, -2.449293598294708485E-15 ) ) ;
#8081 = CARTESIAN_POINT ( 'NONE',  ( 57.59792236341147031, 37.56421063658187620, 40.00000000000002132 ) ) ;
#8082 = CARTESIAN_POINT ( 'NONE',  ( 170.2234770963711128, 1.955190573858485757E-13, -15.44714144992816074 ) ) ;
#8083 = CARTESIAN_POINT ( 'NONE',  ( 184.8905102610680444, -14.79361573936389540, 41.77492675555996016 ) ) ;
#8084 = CARTESIAN_POINT ( 'NONE',  ( 192.4448373802100889, -1.741373372144848397E-13, 20.00000000003942091 ) ) ;
#8085 = CARTESIAN_POINT ( 'NONE',  ( 0.2972598230769976091, -10.13633138497465147, -10.13633138497482733 ) ) ;
#8086 = ORIENTED_EDGE ( 'NONE', *, *, #24913, .T. ) ;
#8087 = FACE_OUTER_BOUND ( 'NONE', #21679, .T. ) ;
#8088 = CARTESIAN_POINT ( 'NONE',  ( -97.73860346104329722, -8.987542150717732881, 20.56359266935457342 ) ) ;
#8089 = CONTEXT_DEPENDENT_SHAPE_REPRESENTATION ( #18355, #18463 ) ;
#8090 = ORIENTED_EDGE ( 'NONE', *, *, #5017, .F. ) ;
#8091 = ORIENTED_EDGE ( 'NONE', *, *, #10586, .F. ) ;
#8092 = CARTESIAN_POINT ( 'NONE',  ( -213.1075012329537230, -66.26714140138676612, 9.698598906462487790 ) ) ;
#8093 = CARTESIAN_POINT ( 'NONE',  ( 23.41418334855299221, -42.84479974151761184, -23.33148157649304366 ) ) ;
#8094 = EDGE_LOOP ( 'NONE', ( #21217, #8700 ) ) ;
#8095 = CARTESIAN_POINT ( 'NONE',  ( 151.7948205124836534, 6.767089262349062828, -40.00000000000002132 ) ) ;
#8096 = CARTESIAN_POINT ( 'NONE',  ( -100.0968563617800271, -20.41799937591574832, 8.893120081479189309 ) ) ;
#8098 = VERTEX_POINT ( 'NONE', #7126 ) ;
#8097 = EDGE_CURVE ( 'NONE', #16256, #6362, #22153, .T. ) ;
#8099 = CARTESIAN_POINT ( 'NONE',  ( 199.9999999999999432, 14.48708306876533136, 12.30466461812483914 ) ) ;
#8100 = CARTESIAN_POINT ( 'NONE',  ( -362.0709805440841365, -4.857225732735059864E-14, 0.000000000000000000 ) ) ;
#8101 = CARTESIAN_POINT ( 'NONE',  ( -100.7734535825088500, 12.25131212657490209, -44.31723036834897300 ) ) ;
#8102 = CARTESIAN_POINT ( 'NONE',  ( -188.8384220655415788, -43.28887647197276323, -17.93083973458484692 ) ) ;
#8103 = CARTESIAN_POINT ( 'NONE',  ( -91.56559293963834989, -39.99999999999995737, -22.67402823373205933 ) ) ;
#8104 = CARTESIAN_POINT ( 'NONE',  ( -259.2033419157646676, -9.517827891722680178, 40.00000000000002132 ) ) ;
#8105 = CARTESIAN_POINT ( 'NONE',  ( 19.06497207195981858, 10.03556273973516078, -66.60410523465806421 ) ) ;
#8106 = CARTESIAN_POINT ( 'NONE',  ( 199.0259813356335883, -9.719824439858887999, 17.48565896982476175 ) ) ;
#8107 = VECTOR ( 'NONE', #1463, 1000.000000000000000 ) ;
#8108 = AXIS2_PLACEMENT_3D ( 'NONE', #10204, #4234, #16713 ) ;
#8109 = AXIS2_PLACEMENT_3D ( 'NONE', #10823, #14936, #20940 ) ;
#8110 = CARTESIAN_POINT ( 'NONE',  ( -56.48582580120559271, 2.158176344243877536E-14, -9.153146818113587102 ) ) ;
#8111 = CARTESIAN_POINT ( 'NONE',  ( -192.9588430854689989, -2.280704836619014309E-13, 54.46834944099972375 ) ) ;
#8112 = AXIS2_PLACEMENT_3D ( 'NONE', #5591, #21820, #7704 ) ;
#8113 = CARTESIAN_POINT ( 'NONE',  ( 57.59792236341149163, -39.99999999999961631, -37.56421063658228832 ) ) ;
#8114 = CARTESIAN_POINT ( 'NONE',  ( -280.0000000000000568, 40.00000000000004263, -19.99999999999987210 ) ) ;
#8115 = FACE_BOUND ( 'NONE', #9067, .T. ) ;
#8116 = CARTESIAN_POINT ( 'NONE',  ( 57.59792236341148453, -54.84617931850877426, -1.722363176415331099 ) ) ;
#8117 = CARTESIAN_POINT ( 'NONE',  ( -135.8532207217289738, 9.153146818113548022, -40.00000000000002132 ) ) ;
#8118 = CARTESIAN_POINT ( 'NONE',  ( 0.2972598230770153171, -66.70487387989861361, 10.13633138497438324 ) ) ;
#8119 = CARTESIAN_POINT ( 'NONE',  ( 200.0000000000000000, 40.00000000000006395, 0.000000000000000000 ) ) ;
#8120 = CARTESIAN_POINT ( 'NONE',  ( 3.854699808470075428, -48.95177852071786617, 14.12217777258779172 ) ) ;
#8121 = CARTESIAN_POINT ( 'NONE',  ( -91.56559293963834989, -2.543181659092656077E-13, 22.67402823373191723 ) ) ;
#8122 = CARTESIAN_POINT ( 'NONE',  ( 151.7948205124836250, 1.807796684091926154E-15, 6.767089262349031742 ) ) ;
#8123 = CARTESIAN_POINT ( 'NONE',  ( -56.48582580120559982, 50.09629031063966664, -6.472252184284094767 ) ) ;
#8124 = CARTESIAN_POINT ( 'NONE',  ( 4.995406935893293543, -10.78321810388990265, -10.78321810389009272 ) ) ;
#8125 = CARTESIAN_POINT ( 'NONE',  ( -192.1964066537693441, -24.16259023441511644, -43.96877160660515216 ) ) ;
#8126 = CARTESIAN_POINT ( 'NONE',  ( -192.9588430854690273, -38.51493924976932703, -18.05360324515463688 ) ) ;
#8127 = ORIENTED_EDGE ( 'NONE', *, *, #20727, .T. ) ;
#8128 = CARTESIAN_POINT ( 'NONE',  ( 184.8905102610680444, -43.07788698682556827, -13.49065550809859104 ) ) ;
#8129 = CARTESIAN_POINT ( 'NONE',  ( 190.0000000000000000, -52.49999999999970868, 82.49999999999998579 ) ) ;
#8130 = DIRECTION ( 'NONE',  ( -1.000000000000000000, 1.836970198721030181E-16, 0.000000000000000000 ) ) ;
#8131 = CARTESIAN_POINT ( 'NONE',  ( -87.13361725327074225, 15.19799821270847850, -15.19799821270833284 ) ) ;
#8132 = CARTESIAN_POINT ( 'NONE',  ( -280.0000000000000568, -14.14213562373049449, -42.42640687119305198 ) ) ;
#8133 = CARTESIAN_POINT ( 'NONE',  ( -87.08748155317879025, 3.397954955031054158, 21.19318107435227816 ) ) ;
#8134 = EDGE_LOOP ( 'NONE', ( #23670, #25437, #24038, #18738 ) ) ;
#8135 = VECTOR ( 'NONE', #4431, 1000.000000000000000 ) ;
#8136 = CARTESIAN_POINT ( 'NONE',  ( 199.9999999999999716, 18.87797660738322847, 2.189960623836138875 ) ) ;
#8137 = CARTESIAN_POINT ( 'NONE',  ( 18.90082831370061101, -24.18116416851801276, 43.99399836018049825 ) ) ;
#8138 = CARTESIAN_POINT ( 'NONE',  ( -3.406542234096830768, 17.94112998239669565, 43.31371932780069045 ) ) ;
#8139 = ORIENTED_EDGE ( 'NONE', *, *, #17195, .F. ) ;
#8140 = ORIENTED_EDGE ( 'NONE', *, *, #11404, .T. ) ;
#8141 = CARTESIAN_POINT ( 'NONE',  ( -192.9588430854689989, 14.46834944099965981, 0.000000000000000000 ) ) ;
#8142 = CARTESIAN_POINT ( 'NONE',  ( 199.0061077845142279, 7.790749371913985755, -18.41559517569303495 ) ) ;
#8143 = CARTESIAN_POINT ( 'NONE',  ( 160.9163046357249129, -125.7889608577475400, 61.61140153332250691 ) ) ;
#8144 =( NAMED_UNIT ( * ) PLANE_ANGLE_UNIT ( ) SI_UNIT ( $, .RADIAN. ) );
#8145 = EDGE_CURVE ( 'NONE', #4791, #2760, #17107, .T. ) ;
#8146 = CARTESIAN_POINT ( 'NONE',  ( -4.039451493210501454, 43.00522595894040734, -23.44932283416630270 ) ) ;
#8147 = CARTESIAN_POINT ( 'NONE',  ( -105.3755690713226727, -2.472783935621397949E-13, 21.75974354311649961 ) ) ;
#8148 = CARTESIAN_POINT ( 'NONE',  ( 200.0000000000005400, -16.47398309245309278, 9.506867245997410620 ) ) ;
#8149 = CARTESIAN_POINT ( 'NONE',  ( -656.7826941990241494, 39.84779524062224709, 4.035097616097491624 ) ) ;
#8150 = AXIS2_PLACEMENT_3D ( 'NONE', #2988, #19713, #13467 ) ;
#8151 = DIRECTION ( 'NONE',  ( 1.000000000000000000, 1.836970198721030181E-16, 0.000000000000000000 ) ) ;
#8152 = CARTESIAN_POINT ( 'NONE',  ( 199.0224671581742371, 2.272106995489924230, 19.87442369886018767 ) ) ;
#8153 = CARTESIAN_POINT ( 'NONE',  ( -192.4602856790872067, 43.06412164779830221, 17.83774323820395935 ) ) ;
#8154 = CARTESIAN_POINT ( 'NONE',  ( 12.77879914700383601, -18.55776024548864100, -44.80239647190805385 ) ) ;
#8155 = CARTESIAN_POINT ( 'NONE',  ( 151.7948205124836250, -4.785054706301600902, -4.785054706301715477 ) ) ;
#8156 = B_SPLINE_CURVE_WITH_KNOTS ( 'NONE', 3,
 ( #23217, #9234, #13102, #21223, #11224, #11100, #2600, #998, #8845, #9101, #17210, #12841, #21350, #25348, #7105, #19340 ),
 .UNSPECIFIED., .F., .F.,
 ( 4, 2, 2, 2, 2, 2, 2, 4 ),
 ( 0.0003146141176185928779, 0.002410294611460639825, 0.003458134858381662919, 0.004505975105302687314, 0.008697336092986771017, 0.01079301658682881374, 0.01288869708067085298, 0.01708005806835492801 ),
 .UNSPECIFIED. ) ;
#8157 = CARTESIAN_POINT ( 'NONE',  ( -114.6380801921473136, 5.502540229729388166, -21.35054024078830182 ) ) ;
#8158 = CARTESIAN_POINT ( 'NONE',  ( -135.8532207217289738, -50.09629031063965243, -6.472252184284438492 ) ) ;
#8159 = DIRECTION ( 'NONE',  ( 0.000000000000000000, 0.000000000000000000, 1.000000000000000000 ) ) ;
#8160 = CARTESIAN_POINT ( 'NONE',  ( -86.96347745069644475, 15.38646221621772092, 15.38646221621800336 ) ) ;
#8161 = CARTESIAN_POINT ( 'NONE',  ( 14.38125909742182884, -55.17850393972636169, -2.449293598294708485E-15 ) ) ;
#8162 = EDGE_CURVE ( 'NONE', #11812, #7311, #10369, .T. ) ;
#8163 = CARTESIAN_POINT ( 'NONE',  ( 98.29820294267436509, 14.14213562374297695, -14.14213562372651189 ) ) ;
#8164 = CARTESIAN_POINT ( 'NONE',  ( -30.26275506840322649, -41.69427246844630019, -2.449293598294708485E-15 ) ) ;
#8165 = CARTESIAN_POINT ( 'NONE',  ( -105.2066640875961667, 15.82458427809276635, 14.56001627727798997 ) ) ;
#8166 = CARTESIAN_POINT ( 'NONE',  ( -259.2033419157646676, 2.741182173978444749E-13, -30.48217210827739621 ) ) ;
#8167 = CARTESIAN_POINT ( 'NONE',  ( 151.7948205124836250, -23.49921654116339553, -23.49921654116350211 ) ) ;
#8168 = CARTESIAN_POINT ( 'NONE',  ( 151.7948205124836534, -33.23291073765550863, -40.00000000000002132 ) ) ;
#8169 = ORIENTED_EDGE ( 'NONE', *, *, #5638, .T. ) ;
#8170 = EDGE_LOOP ( 'NONE', ( #2942, #2696, #18443, #20520 ) ) ;
#8171 = CARTESIAN_POINT ( 'NONE',  ( 19.06497207195980792, 14.19242893257840699, 40.00000000000002132 ) ) ;
#8172 = CARTESIAN_POINT ( 'NONE',  ( -220.0000000000000284, 75.00000000000000000, 0.000000000000000000 ) ) ;
#8173 = CARTESIAN_POINT ( 'NONE',  ( -162.0762913951021176, 39.99999999999998579, 1.694272876828463614 ) ) ;
#8174 = CARTESIAN_POINT ( 'NONE',  ( -259.2033419157646676, 49.83842185052017015, 6.730120644404137487 ) ) ;
#8175 = CARTESIAN_POINT ( 'NONE',  ( -259.2033419157646676, -9.517827891722680178, 40.00000000000002132 ) ) ;
#8176 = PRODUCT_DEFINITION ( 'UNKNOWN', '', #21086, #2993 ) ;
#8177 = CARTESIAN_POINT ( 'NONE',  ( -199.9999999999999432, -55.16984130226904171, -4.865628651906555469 ) ) ;
#8178 = DIRECTION ( 'NONE',  ( 1.000000000000000000, 0.000000000000000000, 0.000000000000000000 ) ) ;
#8179 = CARTESIAN_POINT ( 'NONE',  ( 199.9999999999999716, 15.96353534131429797, 10.31599105002992545 ) ) ;
#8180 = CARTESIAN_POINT ( 'NONE',  ( 199.9999999999999147, -11.07985673941785976, -15.44349624739909643 ) ) ;
#8181 = CARTESIAN_POINT ( 'NONE',  ( 0.2972598230769959993, 38.42060263243713081, -38.42060263243619289 ) ) ;
#8182 = CARTESIAN_POINT ( 'NONE',  ( 4.995406935893312195, -67.35176059882525124, -10.78321810390210445 ) ) ;
#8183 = CARTESIAN_POINT ( 'NONE',  ( -114.6510887843185458, 21.42093443206506365, 5.129768820901790427 ) ) ;
#8184 = CARTESIAN_POINT ( 'NONE',  ( -86.94888381183984905, 19.08739374734031102, -9.627065680628259514 ) ) ;
#8185 = CARTESIAN_POINT ( 'NONE',  ( -192.9588430854690273, -66.79921049721887982, -10.23066800229569040 ) ) ;
#8186 = CARTESIAN_POINT ( 'NONE',  ( 14.38125909742180752, 10.73282306404735387, -10.73282306404708919 ) ) ;
#8187 = CARTESIAN_POINT ( 'NONE',  ( -208.1127848780264742, -17.67593391476659548, 38.89260858015730804 ) ) ;
#8188 = EDGE_CURVE ( 'NONE', #13247, #25916, #19618, .T. ) ;
#8189 = CARTESIAN_POINT ( 'NONE',  ( 130.8568914410475088, -4.207082182989324792, -52.36146031193423056 ) ) ;
#8190 = CARTESIAN_POINT ( 'NONE',  ( 199.0199803820819966, 7.637620434976441608, 18.48637365640330188 ) ) ;
#8192 = CARTESIAN_POINT ( 'NONE',  ( 184.8905102610680444, -3.509827109981123710E-14, 19.07866798485558490 ) ) ;
#8191 = CARTESIAN_POINT ( 'NONE',  ( -198.0356074513804572, 39.15871834505956173, -39.15871834505865223 ) ) ;
#8193 = CARTESIAN_POINT ( 'NONE',  ( 57.59792236341147031, 54.84617931850878136, 1.722363176415705910 ) ) ;
#8194 = CARTESIAN_POINT ( 'NONE',  ( 22.98934664983196896, 43.11412319250747771, -17.85845455615981692 ) ) ;
#8195 = CARTESIAN_POINT ( 'NONE',  ( -208.1127848780264742, 55.00245453010919050, -40.00000000000002132 ) ) ;
#8196 = EDGE_LOOP ( 'NONE', ( #24874, #16484 ) ) ;
#8197 = CARTESIAN_POINT ( 'NONE',  ( 22.27781863241737881, -23.58928354682958428, -43.19367102561737681 ) ) ;
#8198 = CARTESIAN_POINT ( 'NONE',  ( -24.51100708749678958, -37.39427017799431496, 15.48921386276234635 ) ) ;
#8199 = CARTESIAN_POINT ( 'NONE',  ( -162.0762913951020892, 41.69427287682832173, 2.449293598294708485E-15 ) ) ;
#8200 = ORIENTED_EDGE ( 'NONE', *, *, #10443, .F. ) ;
#8201 = CARTESIAN_POINT ( 'NONE',  ( 199.9999999999996589, -18.76526504493254777, 3.099636891498418478 ) ) ;
#8202 = CARTESIAN_POINT ( 'NONE',  ( 8.602182264134457412, -18.59145335917481390, 44.88373884392621704 ) ) ;
#8203 = CARTESIAN_POINT ( 'NONE',  ( 7.112934525910308281, 18.57375239870144057, -44.84100494513564428 ) ) ;
#8204 = CARTESIAN_POINT ( 'NONE',  ( 199.0078145870362221, 1.786107411569149317, -19.91668635079984284 ) ) ;
#8205 = CARTESIAN_POINT ( 'NONE',  ( -87.13361725327075646, -15.19799821270861706, 15.19799821270823159 ) ) ;
#8206 = FACE_BOUND ( 'NONE', #17081, .T. ) ;
#8207 = CARTESIAN_POINT ( 'NONE',  ( 14.38125909742181108, -5.035366881890652543E-14, 15.17850393972633682 ) ) ;
#8208 = CARTESIAN_POINT ( 'NONE',  ( -280.0000000000000568, -14.14213562373049449, -42.42640687119305198 ) ) ;
#8209 = CARTESIAN_POINT ( 'NONE',  ( -30.26275506840324070, -1.694272468446265112, 0.000000000000000000 ) ) ;
#8211 = CARTESIAN_POINT ( 'NONE',  ( -213.1075012329537230, 9.698598906450543566, -9.698598906450348167 ) ) ;
#8210 = CARTESIAN_POINT ( 'NONE',  ( -188.6013942375886643, 23.51434495930266166, -43.09289976588191706 ) ) ;
#8212 = CARTESIAN_POINT ( 'NONE',  ( -280.0000000000000568, 14.14213562373038968, 42.42640687119305198 ) ) ;
#8213 = CARTESIAN_POINT ( 'NONE',  ( -91.56559293963834989, -17.32597176626812896, -2.449293598294708485E-15 ) ) ;
#8214 = CARTESIAN_POINT ( 'NONE',  ( -198.0356074513804572, 55.37879056874818673, -40.00000000000002132 ) ) ;
#8215 = CARTESIAN_POINT ( 'NONE',  ( 57.59792236341148453, -40.00000000000003553, 2.435789363417741438 ) ) ;
#8216 = CARTESIAN_POINT ( 'NONE',  ( 91.82158438592158234, -12.16597498400057198, 44.40256751092329779 ) ) ;
#8217 = CARTESIAN_POINT ( 'NONE',  ( -96.94475454973485284, 20.92018922310817430, -8.190683501891818707 ) ) ;
#8218 = CARTESIAN_POINT ( 'NONE',  ( -198.0356074513804572, -10.87444709758429262, -67.44298959250878056 ) ) ;
#8219 = EDGE_LOOP ( 'NONE', ( #11928, #4385, #8729, #16345, #15842, #734, #11962, #18193 ) ) ;
#8220 = CARTESIAN_POINT ( 'NONE',  ( -259.2033419157646676, -6.730120644403570829, -6.730120644403545960 ) ) ;
#8221 = CARTESIAN_POINT ( 'NONE',  ( -94.58360650938116976, 9.000712009833122806, 20.58386743644784289 ) ) ;
#8222 = APPLICATION_PROTOCOL_DEFINITION ( 'draft international standard', 'automotive_design', 1998, #17728 ) ;
#8223 = ORIENTED_EDGE ( 'NONE', *, *, #22077, .T. ) ;
#8224 = ORIENTED_EDGE ( 'NONE', *, *, #23857, .F. ) ;
#8225 = CARTESIAN_POINT ( 'NONE',  ( -280.0000000000000568, -42.42640687119285303, -14.14213562373118371 ) ) ;
#8226 = CARTESIAN_POINT ( 'NONE',  ( 21.45050411889744879, -43.51299627225506583, -18.02367319544785218 ) ) ;
#8227 = ORIENTED_EDGE ( 'NONE', *, *, #8079, .F. ) ;
#8228 = CARTESIAN_POINT ( 'NONE',  ( 192.4448373802100889, -20.00000000003938538, 0.000000000000000000 ) ) ;
#8229 = FACE_BOUND ( 'NONE', #17260, .T. ) ;
#8230 = VERTEX_POINT ( 'NONE', #23999 ) ;
#8231 = CARTESIAN_POINT ( 'NONE',  ( 199.9999999999998863, 8.393744152662998559, 17.05383455604227905 ) ) ;
#8232 = CARTESIAN_POINT ( 'NONE',  ( -105.2054292635175869, -15.19799821370180126, -15.19799821370278892 ) ) ;
#8233 = CARTESIAN_POINT ( 'NONE',  ( -91.56559293963834989, -16.03295912088706388, -16.03295912088710651 ) ) ;
#8234 = CARTESIAN_POINT ( 'NONE',  ( -188.9001659262688406, -43.30536839095038459, -17.93767091109504008 ) ) ;
#8235 = CARTESIAN_POINT ( 'NONE',  ( 57.59792236341148453, -40.00000000000000000, -2.435789363418300546 ) ) ;
#8236 = CARTESIAN_POINT ( 'NONE',  ( 19.06497207195980792, 14.19242893257840876, 0.000000000000000000 ) ) ;
#8237 = CARTESIAN_POINT ( 'NONE',  ( -86.96347745069644475, 12.89780903124419353, -12.89780903124389333 ) ) ;
#8238 = CARTESIAN_POINT ( 'NONE',  ( 199.0262910934941942, -12.18938195246538037, 15.86593956234834479 ) ) ;
#8239 = CARTESIAN_POINT ( 'NONE',  ( 57.59792236341148453, -40.00000000000000000, -2.435789363418300546 ) ) ;
#8240 = CARTESIAN_POINT ( 'NONE',  ( 0.2972598230770103767, -40.00000000000021316, 54.33493731733921805 ) ) ;
#8241 = CARTESIAN_POINT ( 'NONE',  ( 4.995406935893283773, 39.99999999999997158, 15.24977328854846803 ) ) ;
#8242 = CARTESIAN_POINT ( 'NONE',  ( -105.3755690713226869, 21.75974354311648540, -0.000000000000000000 ) ) ;
#8243 = CARTESIAN_POINT ( 'NONE',  ( -213.1075012329536946, -37.98287015391263566, 37.98287015391218802 ) ) ;
#8244 = CARTESIAN_POINT ( 'NONE',  ( -105.3755690713226585, 21.75974354311648185, -40.00000000000002132 ) ) ;
#8245 = CARTESIAN_POINT ( 'NONE',  ( -30.26275506840322649, -29.48230279907810925, 29.48230279907778950 ) ) ;
#8246 = DIRECTION ( 'NONE',  ( 0.000000000000000000, 1.000000000000000000, 0.000000000000000000 ) ) ;
#8247 = ADVANCED_FACE ( 'NONE', ( #5644 ), #3793, .T. ) ;
#8248 = FACE_BOUND ( 'NONE', #8296, .T. ) ;
#8249 = CARTESIAN_POINT ( 'NONE',  ( -135.8532207217289738, 3.005970985514575011E-13, -30.84685318188645553 ) ) ;
#8250 = CARTESIAN_POINT ( 'NONE',  ( -192.9588430854690273, -40.00000000000024158, 54.46834944101708231 ) ) ;
#8251 = CARTESIAN_POINT ( 'NONE',  ( -208.1127848780264742, 38.89260858015732936, -17.67593391476642140 ) ) ;
#8252 = CARTESIAN_POINT ( 'NONE',  ( -83.21262154144099554, -33.12752917118399409, 13.72187187061446956 ) ) ;
#8253 = CARTESIAN_POINT ( 'NONE',  ( -192.9370379451175097, -24.26711011075247271, -44.11033005021999998 ) ) ;
#8254 = CARTESIAN_POINT ( 'NONE',  ( -259.2033419157646676, -21.55415060305854524, 21.55415060305827524 ) ) ;
#8255 = ORIENTED_EDGE ( 'NONE', *, *, #20606, .F. ) ;
#8256 = CARTESIAN_POINT ( 'NONE',  ( -30.26275506840324070, -27.08623969584554558, -29.48230279907826912 ) ) ;
#8257 = CYLINDRICAL_SURFACE ( 'NONE', #2548, 5.000000000000011546 ) ;
#8258 = CARTESIAN_POINT ( 'NONE',  ( 14.38125909742182884, -55.17850393972636169, -2.449293598294708485E-15 ) ) ;
#8259 = CARTESIAN_POINT ( 'NONE',  ( -200.0000000000000000, -82.49999999999990052, 52.49999999999977263 ) ) ;
#8260 = SHAPE_REPRESENTATION_RELATIONSHIP ( 'NONE' , 'NONE' ,  #24774, #25803 ) ;
#8261 = ORIENTED_EDGE ( 'NONE', *, *, #22837, .F. ) ;
#8262 = ORIENTED_EDGE ( 'NONE', *, *, #21113, .F. ) ;
#8263 = CARTESIAN_POINT ( 'NONE',  ( 200.0000000000000000, 8.256023932303243384, 17.12527061769673153 ) ) ;
#8264 = CARTESIAN_POINT ( 'NONE',  ( 4.990269915386278399, -24.74342916192414776, 44.75621547178053561 ) ) ;
#8265 = CARTESIAN_POINT ( 'NONE',  ( -4.112199523541869794, 13.82298295336142324, 46.96527782736819034 ) ) ;
#8266 = ORIENTED_EDGE ( 'NONE', *, *, #19899, .F. ) ;
#8267 = ORIENTED_EDGE ( 'NONE', *, *, #1200, .T. ) ;
#8268 = PRODUCT_DEFINITION_SHAPE ( 'NONE', 'NONE',  #26362 ) ;
#8269 = CARTESIAN_POINT ( 'NONE',  ( 146.6084372240433709, -34.62501878078303008, -40.00000000000002132 ) ) ;
#8270 = CARTESIAN_POINT ( 'NONE',  ( 199.0060114145493912, 8.242208747961328186, -18.21796198456784666 ) ) ;
#8271 = CARTESIAN_POINT ( 'NONE',  ( -77.55640685876515761, -15.64922766773196905, -15.64922766773223195 ) ) ;
#8272 = CARTESIAN_POINT ( 'NONE',  ( -259.2033419157646676, -6.730120644403570829, -6.730120644403545960 ) ) ;
#8273 = CARTESIAN_POINT ( 'NONE',  ( -102.4309680866095817, -8.733065089892845023, -20.17061239845038756 ) ) ;
#8274 = CARTESIAN_POINT ( 'NONE',  ( 91.82158438592158234, 2.580785920671402147E-13, -22.79471317813470321 ) ) ;
#8275 = CARTESIAN_POINT ( 'NONE',  ( 192.4448373802101173, 39.99999999999985079, 20.00000000003984013 ) ) ;
#8276 = CARTESIAN_POINT ( 'NONE',  ( -126.6834154282237250, 24.89646316986586783, -9.107266658309480789 ) ) ;
#8277 = DIRECTION ( 'NONE',  ( 0.000000000000000000, 1.000000000000000000, 0.000000000000000000 ) ) ;
#8278 = CARTESIAN_POINT ( 'NONE',  ( 199.0176798082135008, 11.64390658120213828, 16.27508030683247497 ) ) ;
#8279 = CARTESIAN_POINT ( 'NONE',  ( -188.8948201289223618, 17.93709820916097186, 43.30398576617481154 ) ) ;
#8280 = CARTESIAN_POINT ( 'NONE',  ( 23.36462152323051811, -23.34178792078175491, -42.86003749000681751 ) ) ;
#8281 = CARTESIAN_POINT ( 'NONE',  ( 136.1360204305621551, -31.79587985999279454, 24.77266263493094911 ) ) ;
#8282 = CARTESIAN_POINT ( 'NONE',  ( -88.39148973765144035, 19.92926839984422926, -8.577159256668510423 ) ) ;
#8283 = CARTESIAN_POINT ( 'NONE',  ( -213.1075012329536946, -37.98287015391263566, 37.98287015391218802 ) ) ;
#8284 = DIRECTION ( 'NONE',  ( 1.000000000000000000, -1.836970198721030181E-16, -0.000000000000000000 ) ) ;
#8285 = FACE_OUTER_BOUND ( 'NONE', #12089, .T. ) ;
#8286 = CARTESIAN_POINT ( 'NONE',  ( -213.1075012329537230, -53.71589010950170717, 40.00000000000002132 ) ) ;
#8287 = CARTESIAN_POINT ( 'NONE',  ( -192.9588430854689989, 10.23066800230756712, -10.23066800230735396 ) ) ;
#8288 = CARTESIAN_POINT ( 'NONE',  ( -280.0000000000000568, -20.00000000000007105, 40.00000000000002132 ) ) ;
#8289 = CARTESIAN_POINT ( 'NONE',  ( -105.2034101837812727, 14.35414403269573391, 16.06048591665815906 ) ) ;
#8290 = CARTESIAN_POINT ( 'NONE',  ( 146.6084372240433709, 39.99999999999968026, 34.62501878078347772 ) ) ;
#8291 = CARTESIAN_POINT ( 'NONE',  ( 184.8905102610680444, -14.79361573936379415, -14.79361573936387941 ) ) ;
#8292 = CARTESIAN_POINT ( 'NONE',  ( 170.2234770963711128, -24.55285855007184281, -40.00000000000002132 ) ) ;
#8293 = ORIENTED_EDGE ( 'NONE', *, *, #7839, .F. ) ;
#8294 = ADVANCED_FACE ( 'NONE', ( #22022 ), #11489, .T. ) ;
#8295 = ORIENTED_EDGE ( 'NONE', *, *, #24365, .T. ) ;
#8296 = EDGE_LOOP ( 'NONE', ( #1202, #23202 ) ) ;
#8297 = CARTESIAN_POINT ( 'NONE',  ( -91.56559293963834989, -22.67402823373193499, 0.000000000000000000 ) ) ;
#8298 = CIRCLE ( 'NONE', #14656, 10.00000000000000000 ) ;
#8299=STYLED_ITEM('',(#26402),#8434);
#8300 = VECTOR ( 'NONE', #3378, 1000.000000000000000 ) ;
#8301 = CARTESIAN_POINT ( 'NONE',  ( 57.59792236341147031, 54.84617931850878136, 1.722363176415705910 ) ) ;
#8302 = CARTESIAN_POINT ( 'NONE',  ( -105.3901353553978737, -20.30436174851991282, -6.689050419658350677 ) ) ;
#8303 = CARTESIAN_POINT ( 'NONE',  ( -114.4364955367327497, -8.064892380842218600, -20.29001642038850406 ) ) ;
#8304 = CARTESIAN_POINT ( 'NONE',  ( 180.0000000000000284, -135.7889608577475542, -82.49999999999998579 ) ) ;
#8305 = CARTESIAN_POINT ( 'NONE',  ( 199.9999999999998579, 13.31531350134012648, 13.56203446005050317 ) ) ;
#8306 = VECTOR ( 'NONE', #13372, 1000.000000000000000 ) ;
#8307 = CARTESIAN_POINT ( 'NONE',  ( 199.9999999999999716, -18.96854328187948369, -1.244406218240217799 ) ) ;
#8308 = VECTOR ( 'NONE', #13906, 1000.000000000000000 ) ;
#8310 = VECTOR ( 'NONE', #11872, 1000.000000000000000 ) ;
#8309 = CARTESIAN_POINT ( 'NONE',  ( 184.8905102610680444, 41.77492675555983936, 14.79361573936436081 ) ) ;
#8311 = CARTESIAN_POINT ( 'NONE',  ( 151.7948205124836250, -4.785054706301600902, -4.785054706301715477 ) ) ;
#8312 = LINE ( 'NONE', #341, #7581 ) ;
#8313 = CARTESIAN_POINT ( 'NONE',  ( -208.1127848780264742, 40.00000000000055422, -55.00245453014380814 ) ) ;
#8314 = CARTESIAN_POINT ( 'NONE',  ( -91.56559293963836410, -12.25131212657524138, 44.31723036834888774 ) ) ;
#8315 = CARTESIAN_POINT ( 'NONE',  ( -91.56559293963834989, -16.03295912088728414, 16.03295912088688269 ) ) ;
#8316 = CARTESIAN_POINT ( 'NONE',  ( 151.7948205124836250, -23.49921654116339553, -23.49921654116350211 ) ) ;
#8317 = CARTESIAN_POINT ( 'NONE',  ( 192.4448373802101173, -14.14213562370283128, -42.42640687122081999 ) ) ;
#8318 = DIRECTION ( 'NONE',  ( 1.000000000000000000, 1.836970198721030181E-16, 0.000000000000000000 ) ) ;
#8320 = CARTESIAN_POINT ( 'NONE',  ( -162.0762913951020892, -1.777970010055771463E-13, 41.69427287682835015 ) ) ;
#8319 = CARTESIAN_POINT ( 'NONE',  ( 130.8568914410475088, 32.49135343045448820, 24.07718906446946860 ) ) ;
#8321 = CARTESIAN_POINT ( 'NONE',  ( -198.0356074513804572, 67.44298959250878056, -10.87444709758402261 ) ) ;
#8322 = AXIS2_PLACEMENT_3D ( 'NONE', #3838, #4246, #6222 ) ;
#8323 = CARTESIAN_POINT ( 'NONE',  ( 23.36462152323054653, 42.86003749000685303, -23.34178792078203912 ) ) ;
#8324 = CARTESIAN_POINT ( 'NONE',  ( -105.3755690713226727, 18.24025645688350750, 2.449293598294708485E-15 ) ) ;
#8325 = CARTESIAN_POINT ( 'NONE',  ( 4.995406935893288214, 15.24977328854832770, 0.000000000000000000 ) ) ;
#8326 = ADVANCED_FACE ( 'NONE', ( #25628 ), #3522, .F. ) ;
#8327 = CARTESIAN_POINT ( 'NONE',  ( -3.449394506061680854, -43.30266483527573484, 17.93655106166770707 ) ) ;
#8328 = CARTESIAN_POINT ( 'NONE',  ( -56.48582580120559271, 30.84685318188643066, 2.449293598294708485E-15 ) ) ;
#8329 = EDGE_CURVE ( 'NONE', #14785, #21989, #13496, .T. ) ;
#8330 = VECTOR ( 'NONE', #17781, 1000.000000000000000 ) ;
#8331 = ORIENTED_EDGE ( 'NONE', *, *, #25405, .F. ) ;
#8332 = CARTESIAN_POINT ( 'NONE',  ( 17.76569343199605200, 24.33587863439607801, -44.20364726159859003 ) ) ;
#8333 = CARTESIAN_POINT ( 'NONE',  ( -162.0762913951021176, -27.08623940707624911, 29.48230308784761888 ) ) ;
#8334 = CARTESIAN_POINT ( 'NONE',  ( -77.90255099906870839, -8.064892378658434779, 20.29001641120621713 ) ) ;
#8335 = EDGE_CURVE ( 'NONE', #6393, #23049, #15612, .T. ) ;
#8336 = EDGE_CURVE ( 'NONE', #3196, #14641, #19726, .T. ) ;
#8337 = CARTESIAN_POINT ( 'NONE',  ( -4.022465846214160479, 23.45302613997645125, -43.01021959554122276 ) ) ;
#8338 = CARTESIAN_POINT ( 'NONE',  ( 199.0166470710653925, -15.03895783737594805, -13.18902814565699266 ) ) ;
#8339 = AXIS2_PLACEMENT_3D ( 'NONE', #6500, #2520, #254 ) ;
#8340 = CARTESIAN_POINT ( 'NONE',  ( -105.3755690713226727, -2.472783935621397949E-13, 21.75974354311649961 ) ) ;
#8341 = CARTESIAN_POINT ( 'NONE',  ( 170.0000000000000284, -22.62041470344884431, 9.369682556672202622 ) ) ;
#8342 = CARTESIAN_POINT ( 'NONE',  ( -188.6013942375983561, -13.84412886956598499, 47.09843442133357883 ) ) ;
#8343 = CARTESIAN_POINT ( 'NONE',  ( 184.8905102610680444, -14.79361573936330565, -41.77492675556016621 ) ) ;
#8344 = CARTESIAN_POINT ( 'NONE',  ( 199.9999999999999432, 20.00000000000013856, 0.000000000000000000 ) ) ;
#8346 = CARTESIAN_POINT ( 'NONE',  ( 184.8905102610680444, -14.79361573936399665, 14.79361573936367158 ) ) ;
#8345 = CARTESIAN_POINT ( 'NONE',  ( -195.1685814578025600, 24.52825302092950110, -44.46431112710755684 ) ) ;
#8347 = CARTESIAN_POINT ( 'NONE',  ( -100.7734535825088500, 40.53558337403654832, 16.03295912088756481 ) ) ;
#8348 = CARTESIAN_POINT ( 'NONE',  ( -86.96347745069643054, -18.24025645688353947, 40.00000000000002132 ) ) ;
#8349 = CARTESIAN_POINT ( 'NONE',  ( -100.7734535825088500, 17.32597176626809699, -40.00000000000002132 ) ) ;
#8350 = CARTESIAN_POINT ( 'NONE',  ( 200.0000000000000000, -39.99999999999977973, -20.00000000000034817 ) ) ;
#8351 = CARTESIAN_POINT ( 'NONE',  ( -198.0356074513804572, 39.15871834505901461, 39.15871834505919935 ) ) ;
#8352 = AXIS2_PLACEMENT_3D ( 'NONE', #21830, #3600, #19829 ) ;
#8353 = CARTESIAN_POINT ( 'NONE',  ( -97.73860346100398999, 20.89580782304006590, -8.185503821071858255 ) ) ;
#8354 = CARTESIAN_POINT ( 'NONE',  ( -86.96347745069643054, 15.38646221621821297, -41.18208027870583265 ) ) ;
#8355 = CARTESIAN_POINT ( 'NONE',  ( -114.7469200037856041, 2.762404124414770568, 21.93717741968527335 ) ) ;
#8356 = EDGE_LOOP ( 'NONE', ( #8973, #11864, #12964, #17976 ) ) ;
#8357 = CARTESIAN_POINT ( 'NONE',  ( 184.8905102610680444, -43.07788698682576722, 13.49065550809799063 ) ) ;
#8358 = CARTESIAN_POINT ( 'NONE',  ( -96.94475454968154793, 8.190683501883270878, 20.92018922311200413 ) ) ;
#8359 = CARTESIAN_POINT ( 'NONE',  ( 130.8568914410475088, 24.07718906446891793, 32.49135343045489321 ) ) ;
#8360 = CARTESIAN_POINT ( 'NONE',  ( -4.031723327955742064, -46.99313739789356248, -13.82865651623149894 ) ) ;
#8361 = ORIENTED_EDGE ( 'NONE', *, *, #15865, .T. ) ;
#8362 = CARTESIAN_POINT ( 'NONE',  ( -91.56559293963834989, -22.67402823373193499, 0.000000000000000000 ) ) ;
#8363 = FACE_BOUND ( 'NONE', #5748, .T. ) ;
#8364 = ORIENTED_EDGE ( 'NONE', *, *, #19523, .T. ) ;
#8365 = CARTESIAN_POINT ( 'NONE',  ( 200.0000000000001421, 16.91347576093571803, -8.662591770200990027 ) ) ;
#8366 = CARTESIAN_POINT ( 'NONE',  ( -315.0000000000000568, -4.857225732735059864E-14, 0.000000000000000000 ) ) ;
#8367 = CARTESIAN_POINT ( 'NONE',  ( -348.0000000000001137, -4.857225732735059864E-14, 0.000000000000000000 ) ) ;
#8368 = CARTESIAN_POINT ( 'NONE',  ( -188.6013942376021362, -47.09843442133525571, -13.84412886956576827 ) ) ;
#8369 = AXIS2_PLACEMENT_3D ( 'NONE', #15880, #11903, #3940 ) ;
#8370 = CARTESIAN_POINT ( 'NONE',  ( -135.8532207217289738, -40.00000000000014921, 30.84685318188631697 ) ) ;
#8371 = CARTESIAN_POINT ( 'NONE',  ( 57.59792236341147031, 37.56421063658187620, 40.00000000000002132 ) ) ;
#8372 = CARTESIAN_POINT ( 'NONE',  ( -208.1127848780264742, -17.67593391476605547, -38.89260858015755673 ) ) ;
#8373 = CARTESIAN_POINT ( 'NONE',  ( 199.0259577874143417, -9.576177499050416486, 17.56472219104047028 ) ) ;
#8374 = CARTESIAN_POINT ( 'NONE',  ( -135.8532207217289738, 7.002209520526292428E-15, -9.153146818113572891 ) ) ;
#8375 = CARTESIAN_POINT ( 'NONE',  ( -280.0000000000000568, 39.99999999999990763, 20.00000000000015987 ) ) ;
#8376 = CARTESIAN_POINT ( 'NONE',  ( -56.48582580120560692, 40.00000000000004263, -9.153146818113443217 ) ) ;
#8377 = CARTESIAN_POINT ( 'NONE',  ( 136.1360204305621266, 35.03383547441298873, 0.000000000000000000 ) ) ;
#8378 = CARTESIAN_POINT ( 'NONE',  ( 136.1360204305621266, -4.966164525587039691, -2.449293598294708485E-15 ) ) ;
#8379 = CARTESIAN_POINT ( 'NONE',  ( -213.1075012329537230, 18.58567234101121102, 37.98287015391247223 ) ) ;
#8380 = CARTESIAN_POINT ( 'NONE',  ( -198.0356074513804572, 1.247057299367198800E-13, -15.37879056873070560 ) ) ;
#8381 = CARTESIAN_POINT ( 'NONE',  ( 23.37394308801980713, -42.85717664514568526, -23.33966569535099822 ) ) ;
#8382 = CARTESIAN_POINT ( 'NONE',  ( 146.6084372240433993, 8.568076647504290689E-14, -5.374981219216972583 ) ) ;
#8383 = CARTESIAN_POINT ( 'NONE',  ( -86.96347745069644475, -8.210974027862429531E-14, 18.24025645688352881 ) ) ;
#8384 = CARTESIAN_POINT ( 'NONE',  ( 0.2972598230769938343, 10.13633138497472252, 10.13633138497475628 ) ) ;
#8385 = DIRECTION ( 'NONE',  ( 1.000000000000000000, 1.303213150798907793E-16, 2.465190328815661892E-32 ) ) ;
#8386 = CARTESIAN_POINT ( 'NONE',  ( -162.0762913951020892, 1.198031840385732849, -1.198031840385733515 ) ) ;
#8387 = CARTESIAN_POINT ( 'NONE',  ( 130.8568914410475088, -4.207082182989324792, -52.36146031193423056 ) ) ;
#8388 = ORIENTED_EDGE ( 'NONE', *, *, #532, .T. ) ;
#8389 = CARTESIAN_POINT ( 'NONE',  ( -8.720657192084441789, 45.36528685024551066, -13.49580954686349799 ) ) ;
#8390 = DIRECTION ( 'NONE',  ( -0.3301743753960648675, 0.000000000000000000, -0.9439199552037336183 ) ) ;
#8391 = CARTESIAN_POINT ( 'NONE',  ( -208.1127848780264742, -55.00245453012676222, -2.449293598294708485E-15 ) ) ;
#8392 = CARTESIAN_POINT ( 'NONE',  ( -87.13361725327077068, -1.365653317460838734, -21.49321519333430075 ) ) ;
#8393 = CARTESIAN_POINT ( 'NONE',  ( 136.1360204305621266, -24.77266263493151044, 24.77266263493093135 ) ) ;
#8394 = EDGE_LOOP ( 'NONE', ( #18245, #13365, #24746, #17608 ) ) ;
#8395 = ORIENTED_EDGE ( 'NONE', *, *, #8523, .T. ) ;
#8396 = CARTESIAN_POINT ( 'NONE',  ( 199.9999999999998863, 17.79007744789355172, -6.680419707818059827 ) ) ;
#8397 = CARTESIAN_POINT ( 'NONE',  ( -100.0968563617631020, 8.149320301509460407, -20.72609133246983149 ) ) ;
#8398 = CARTESIAN_POINT ( 'NONE',  ( 21.80824205439920505, 13.88338701302733469, 47.36272483143116574 ) ) ;
#8399 = ORIENTED_EDGE ( 'NONE', *, *, #869, .T. ) ;
#8400 = ORIENTED_EDGE ( 'NONE', *, *, #1588, .T. ) ;
#8401 = CARTESIAN_POINT ( 'NONE',  ( -86.96347745069644475, -15.38646221621786125, -15.38646221621789856 ) ) ;
#8402 = CARTESIAN_POINT ( 'NONE',  ( 199.0142478014330720, -11.65985798941387941, -16.24932773989132073 ) ) ;
#8403 = CARTESIAN_POINT ( 'NONE',  ( -105.2054292635175585, 5.571723593410045370E-14, -21.49321519473985731 ) ) ;
#8404 = DIRECTION ( 'NONE',  ( 0.000000000000000000, 0.7071067811865364705, 0.7071067811865586750 ) ) ;
#8405 = CARTESIAN_POINT ( 'NONE',  ( -213.1075012329537230, 37.98287015391236565, -18.58567234101138510 ) ) ;
#8406 = EDGE_CURVE ( 'NONE', #5454, #122, #26156, .T. ) ;
#8407 = CARTESIAN_POINT ( 'NONE',  ( -87.13361725327072804, 5.903697393916396424E-14, -21.49321519333428299 ) ) ;
#8408 = CARTESIAN_POINT ( 'NONE',  ( -103.9663809734738464, -8.026122149642342052, -20.15238534419602701 ) ) ;
#8409 = CARTESIAN_POINT ( 'NONE',  ( 163.1118516004056573, 1.658263919738574066E-13, -12.73709011382475254 ) ) ;
#8410 = CARTESIAN_POINT ( 'NONE',  ( 163.1118516004056573, 39.99999999999976552, 27.26290988616914746 ) ) ;
#8411 = CARTESIAN_POINT ( 'NONE',  ( -654.3715413940425378, 38.07917292905567308, 12.25576229706686426 ) ) ;
#8412 = DIRECTION ( 'NONE',  ( 0.000000000000000000, 1.000000000000000000, 0.000000000000000000 ) ) ;
#8413 = CARTESIAN_POINT ( 'NONE',  ( 199.0095182511445557, 19.82538855659994681, 2.633105091475395287 ) ) ;
#8414 = CARTESIAN_POINT ( 'NONE',  ( -188.8842190493876103, 17.93596163623949735, 43.30124183641348878 ) ) ;
#8415 = CARTESIAN_POINT ( 'NONE',  ( 192.4448373802101173, -14.14213562370342281, 42.42640687122062104 ) ) ;
#8416 = CARTESIAN_POINT ( 'NONE',  ( -200.0000000000000284, 19.98641303047029893, 45.65206365911533481 ) ) ;
#8417 = CARTESIAN_POINT ( 'NONE',  ( 57.59792236341147031, 30.00663442387683588, 26.56190807104703211 ) ) ;
#8418 = DIRECTION ( 'NONE',  ( 7.916033913021854848E-32, -4.182618615277681568E-16, -1.000000000000000000 ) ) ;
#8419 = CARTESIAN_POINT ( 'NONE',  ( 14.38125909742180752, 17.55144818341503665, -39.01709431150898411 ) ) ;
#8420 = DIRECTION ( 'NONE',  ( 0.000000000000000000, -1.000000000000000000, 0.000000000000000000 ) ) ;
#8421 = CARTESIAN_POINT ( 'NONE',  ( 184.8905102610680444, 20.92133201514447194, 40.00000000000002132 ) ) ;
#8422 = EDGE_CURVE ( 'NONE', #9561, #3201, #2798, .T. ) ;
#8423 = CARTESIAN_POINT ( 'NONE',  ( 151.7948205124836250, 23.49921654116361225, -23.49921654116333514 ) ) ;
#8424 = CARTESIAN_POINT ( 'NONE',  ( 170.2234770963711128, 24.55285855007190676, 40.00000000000002132 ) ) ;
#8425 = DIRECTION ( 'NONE',  ( -0.000000000000000000, -1.000000000000000000, -0.000000000000000000 ) ) ;
#8426 = CARTESIAN_POINT ( 'NONE',  ( -208.1127848780264742, 40.00000000000055422, -55.00245453014380814 ) ) ;
#8427 = CARTESIAN_POINT ( 'NONE',  ( 163.1118516004056573, 37.29075403953160617, -19.27778845539222985 ) ) ;
#8428 = EDGE_CURVE ( 'NONE', #23960, #7172, #18616, .T. ) ;
#8429 = CARTESIAN_POINT ( 'NONE',  ( 153.3020327024397318, -11.77299484472972857, 28.42252382389407472 ) ) ;
#8430 = VERTEX_POINT ( 'NONE', #8571 ) ;
#8431 = EDGE_LOOP ( 'NONE', ( #10734, #1503 ) ) ;
#8432 = ORIENTED_EDGE ( 'NONE', *, *, #23306, .F. ) ;
#8433 = CARTESIAN_POINT ( 'NONE',  ( 170.2234770963711128, -24.55285855007184281, 40.00000000000002132 ) ) ;
#8434 = MANIFOLD_SOLID_BREP ( 'Boss-Extrude6', #5368 ) ;
#8435 = CARTESIAN_POINT ( 'NONE',  ( 167.0466155511622048, 9.710058186601536079, 23.44215416552595954 ) ) ;
#8436 = AXIS2_PLACEMENT_3D ( 'NONE', #9712, #13443, #19559 ) ;
#8437 = CARTESIAN_POINT ( 'NONE',  ( -86.96347745069644475, 12.89780903124419353, -12.89780903124389333 ) ) ;
#8438 = CARTESIAN_POINT ( 'NONE',  ( -114.7465989397488926, -21.93543632637401330, 2.774003790514562251 ) ) ;
#8439 = CARTESIAN_POINT ( 'NONE',  ( -199.9999999999999432, -55.16984130226965277, -2.449293598294708091E-15 ) ) ;
#8440 = DIRECTION ( 'NONE',  ( 0.000000000000000000, -1.000000000000000000, 0.000000000000000000 ) ) ;
#8441 = CARTESIAN_POINT ( 'NONE',  ( 200.0000000000000568, 2.475862818518347552, -18.83975305017670365 ) ) ;
#8442 = CARTESIAN_POINT ( 'NONE',  ( 199.9999999999999147, -1.249805991376689018, -18.96320409372175675 ) ) ;
#8443 = CARTESIAN_POINT ( 'NONE',  ( -162.0762913951020892, 1.198031840456041497, -57.76657433537918251 ) ) ;
#8444 = CARTESIAN_POINT ( 'NONE',  ( -259.2033419157646676, -21.55415060305872998, 35.01439189186525880 ) ) ;
#8445 = DIRECTION ( 'NONE',  ( 1.000000000000000000, 1.836970198721030181E-16, 0.000000000000000000 ) ) ;
#8446 = CARTESIAN_POINT ( 'NONE',  ( 184.8905102610680444, -1.851754852062639767E-13, 20.92133201514444352 ) ) ;
#8447 = CARTESIAN_POINT ( 'NONE',  ( 146.6084372240433709, -32.08495691632075619, 24.48358557860298035 ) ) ;
#8448 = CARTESIAN_POINT ( 'NONE',  ( 136.1360204305621266, 35.03383547441298873, 0.000000000000000000 ) ) ;
#8449 = CARTESIAN_POINT ( 'NONE',  ( 98.29820294270304259, -18.47759065022024672, 7.653668647299475047 ) ) ;
#8450 = CARTESIAN_POINT ( 'NONE',  ( -91.56559293963836410, 16.03295912088714203, -16.03295912088699282 ) ) ;
#8451 = CARTESIAN_POINT ( 'NONE',  ( -192.9588430854689989, -14.46834944099973086, 0.000000000000000000 ) ) ;
#8452 = VECTOR ( 'NONE', #4580, 1000.000000000000000 ) ;
#8454 = CARTESIAN_POINT ( 'NONE',  ( -238.4067589809705794, 39.99999999999983658, 40.96449428006354765 ) ) ;
#8453 = CARTESIAN_POINT ( 'NONE',  ( 136.1360204305621266, 3.511608612530757068, -3.511608612530642937 ) ) ;
#8455 = CARTESIAN_POINT ( 'NONE',  ( -105.3755690713226585, 12.89780903124349720, 43.67073346367994446 ) ) ;
#8456 = CARTESIAN_POINT ( 'NONE',  ( 27.55177309528179208, 45.29548561696966402, -13.49150912998460683 ) ) ;
#8457 = CARTESIAN_POINT ( 'NONE',  ( 163.1118516004056573, 12.73709011382478806, -40.00000000000002132 ) ) ;
#8458 = CARTESIAN_POINT ( 'NONE',  ( -100.7734535825088358, -16.03295912088706743, -16.03295912088710296 ) ) ;
#8459 = CARTESIAN_POINT ( 'NONE',  ( 5.009866156928156400, -24.71463403307551587, -44.71726210619360131 ) ) ;
#8460 = AXIS2_PLACEMENT_3D ( 'NONE', #9947, #7545, #26207 ) ;
#8461 = CARTESIAN_POINT ( 'NONE',  ( -24.88648382771649636, -36.77569126515327724, 19.35593139197868240 ) ) ;
#8462 = CARTESIAN_POINT ( 'NONE',  ( 57.59792236341147031, -2.435789363418150000, 40.00000000000002132 ) ) ;
#8463 = ORIENTED_EDGE ( 'NONE', *, *, #2459, .F. ) ;
#8464 = CARTESIAN_POINT ( 'NONE',  ( -210.0000000000000284, 63.70262460423102624, -57.69613583541415380 ) ) ;
#8465 = CARTESIAN_POINT ( 'NONE',  ( -30.26275506840324070, 1.198031551616013601, 1.198031551616023371 ) ) ;
#8466 = CARTESIAN_POINT ( 'NONE',  ( -626.9846540392097722, 75.00000000000000000, 59.99999999999999289 ) ) ;
#8467 = CARTESIAN_POINT ( 'NONE',  ( 9.349823541344651545, 18.59402391556963252, -44.88994471603341196 ) ) ;
#8468 = CARTESIAN_POINT ( 'NONE',  ( 199.0257179982615128, -18.22226585379655361, 8.261159732268383848 ) ) ;
#8469 = FACE_OUTER_BOUND ( 'NONE', #20313, .T. ) ;
#8470 = CARTESIAN_POINT ( 'NONE',  ( -16.41582555400823651, -39.35881747749594695, -21.03675245716867792 ) ) ;
#8471 = CARTESIAN_POINT ( 'NONE',  ( -188.3066136396866170, -23.45085387054212589, 43.00728998844440554 ) ) ;
#8472 = EDGE_CURVE ( 'NONE', #10135, #6105, #3203, .T. ) ;
#8473 = CIRCLE ( 'NONE', #20400, 69.99999999999998579 ) ;
#8474 = CARTESIAN_POINT ( 'NONE',  ( -135.8532207217289738, -6.472252184284280396, 6.472252184284099208 ) ) ;
#8475 = CARTESIAN_POINT ( 'NONE',  ( -86.96347745069645896, 21.75974354311648895, -0.000000000000000000 ) ) ;
#8477 = CARTESIAN_POINT ( 'NONE',  ( -105.3755690713226727, 12.89780903124418998, -12.89780903124389155 ) ) ;
#8476 = CARTESIAN_POINT ( 'NONE',  ( -188.8384220655398451, 17.93083973458498903, -43.28887647197245059 ) ) ;
#8478 = CARTESIAN_POINT ( 'NONE',  ( -100.7734535825088500, 12.25131212657428748, 44.31723036834913643 ) ) ;
#8479 = CARTESIAN_POINT ( 'NONE',  ( 19.06497207195982924, -54.19242893257843008, -2.449293598294708485E-15 ) ) ;
#8480 = CARTESIAN_POINT ( 'NONE',  ( 151.7948205124836250, 6.767089262349059275, 2.449293598294708485E-15 ) ) ;
#8481 = EDGE_CURVE ( 'NONE', #6964, #1593, #21068, .T. ) ;
#8482 = CARTESIAN_POINT ( 'NONE',  ( 0.2972598230769957217, 1.502051041545559470E-13, -14.33493731733933352 ) ) ;
#8483 = CARTESIAN_POINT ( 'NONE',  ( 14.38125909742181108, 39.01709431150907648, 39.01709431150921858 ) ) ;
#8484 = CARTESIAN_POINT ( 'NONE',  ( 98.29820294267304348, -6.423630604792074372, 18.95183585406402571 ) ) ;
#8485 = CARTESIAN_POINT ( 'NONE',  ( 151.7948205124836534, 23.49921654116056047, -33.06932595376338213 ) ) ;
#8486 =( REPRESENTATION_RELATIONSHIP ('NONE','NONE', #23888, #126 ) REPRESENTATION_RELATIONSHIP_WITH_TRANSFORMATION ( #11817 )SHAPE_REPRESENTATION_RELATIONSHIP( ) );
#8487 = EDGE_CURVE ( 'NONE', #3577, #4428, #4359, .T. ) ;
#8488 = CARTESIAN_POINT ( 'NONE',  ( -259.2033419157646676, 6.730120644403521979, -6.730120644403498886 ) ) ;
#8489 = ADVANCED_FACE ( 'NONE', ( #12426 ), #6569, .F. ) ;
#8490 = VERTEX_POINT ( 'NONE', #24414 ) ;
#8491 = CARTESIAN_POINT ( 'NONE',  ( -162.0762913951020892, 1.198031840385716418, 1.198031840385750169 ) ) ;
#8492 = CARTESIAN_POINT ( 'NONE',  ( -100.0968563617871183, 8.893120081520745401, 20.41799937589878411 ) ) ;
#8493 = ITEM_DEFINED_TRANSFORMATION ( 'NONE', 'NONE', #13805,  #21058 ) ;
#8494 = AXIS2_PLACEMENT_3D ( 'NONE', #2297, #22402, #15992 ) ;
#8495 = CARTESIAN_POINT ( 'NONE',  ( 151.7948205124836534, 23.49921654116009506, 33.06932595376371609 ) ) ;
#8496 = CARTESIAN_POINT ( 'NONE',  ( 6.984886629849392570, -49.25486234614436398, -14.16808340396968013 ) ) ;
#8497 = ORIENTED_EDGE ( 'NONE', *, *, #25450, .T. ) ;
#8498 = LINE ( 'NONE', #658, #14322 ) ;
#8499 = CYLINDRICAL_SURFACE ( 'NONE', #24503, 30.00000000000000711 ) ;
#8500 = ORIENTED_EDGE ( 'NONE', *, *, #21918, .T. ) ;
#8501 = CARTESIAN_POINT ( 'NONE',  ( 200.0000000000002842, 18.39723030902092660, -4.753359243483134655 ) ) ;
#8502 = CARTESIAN_POINT ( 'NONE',  ( 14.33519811653600229, 14.14278418308735574, -49.08818492847909454 ) ) ;
#8503 = CARTESIAN_POINT ( 'NONE',  ( -191.2490444016914637, -43.85246840376581190, -18.16428715638521041 ) ) ;
#8504 = CARTESIAN_POINT ( 'NONE',  ( -100.7734535825088358, -8.145438380286941744E-14, 17.32597176626811120 ) ) ;
#8505 = CARTESIAN_POINT ( 'NONE',  ( 0.2972598230769930017, 54.33493731733938148, -40.00000000000002132 ) ) ;
#8506 = CARTESIAN_POINT ( 'NONE',  ( 14.38125909742180752, 10.73282306404735387, -10.73282306404708919 ) ) ;
#8507 = FACE_OUTER_BOUND ( 'NONE', #14079, .T. ) ;
#8508 = CARTESIAN_POINT ( 'NONE',  ( -56.48582580120557850, -40.00000000000014211, 30.84685318188629921 ) ) ;
#8509 = CARTESIAN_POINT ( 'NONE',  ( -192.9588430854690273, 39.99999999999980105, 54.46834944098235809 ) ) ;
#8510 = PLANE ( 'NONE',  #18077 ) ;
#8511 = CARTESIAN_POINT ( 'NONE',  ( 170.2234770963711128, 24.55285855007190321, 0.000000000000000000 ) ) ;
#8512 = CARTESIAN_POINT ( 'NONE',  ( -135.8532207217289454, -30.84685318188648750, -40.00000000000002132 ) ) ;
#8513 = CARTESIAN_POINT ( 'NONE',  ( -135.8532207217289738, 6.472252184283881604, 50.09629031063969506 ) ) ;
#8514 = CARTESIAN_POINT ( 'NONE',  ( 98.29820294268191105, -7.653668647302824368, -18.47759065022797031 ) ) ;
#8515 = VECTOR ( 'NONE', #19432, 1000.000000000000114 ) ;
#8516 = CARTESIAN_POINT ( 'NONE',  ( -296.0000000000000000, -4.857225732735059864E-14, 20.53474504356812247 ) ) ;
#8517 = CARTESIAN_POINT ( 'NONE',  ( 0.2972598230769956662, 40.00000000000058975, -54.33493731733894094 ) ) ;
#8518 = CARTESIAN_POINT ( 'NONE',  ( -135.8532207217289738, -40.00000000000014921, 30.84685318188631697 ) ) ;
#8519 = CARTESIAN_POINT ( 'NONE',  ( 199.0261637166634330, -10.98746419350304748, 16.71832627740758070 ) ) ;
#8520 = DIRECTION ( 'NONE',  ( -1.000000000000000000, 1.836970198721030181E-16, 0.000000000000000000 ) ) ;
#8521 = CARTESIAN_POINT ( 'NONE',  ( -99.29480781227209718, -8.934325994365195811, -20.48155342677144475 ) ) ;
#8522 = CARTESIAN_POINT ( 'NONE',  ( -280.0000000000000000, -14.14213562373108779, 14.14213562373088529 ) ) ;
#8523 = EDGE_CURVE ( 'NONE', #15766, #25369, #22465, .T. ) ;
#8524 = VERTEX_POINT ( 'NONE', #2200 ) ;
#8525 = CARTESIAN_POINT ( 'NONE',  ( -17.28139728229472993, 42.38047544420368240, -12.88180358348748378 ) ) ;
#8526 = CARTESIAN_POINT ( 'NONE',  ( 126.3230993689413708, 28.30579214049057413, -11.72464299830486389 ) ) ;
#8527 = CARTESIAN_POINT ( 'NONE',  ( 146.6084372240433709, -5.374981219216942385, -40.00000000000002132 ) ) ;
#8528 = CARTESIAN_POINT ( 'NONE',  ( -83.21262154144248768, -33.12752917118415752, -13.72187187061501490 ) ) ;
#8529 = CARTESIAN_POINT ( 'NONE',  ( -213.1075012329537230, 9.698598906450543566, -9.698598906450348167 ) ) ;
#8530 = SHAPE_REPRESENTATION_RELATIONSHIP ( 'NONE' , 'NONE' ,  #9131, #22943 ) ;
#8531 = ORIENTED_EDGE ( 'NONE', *, *, #9075, .F. ) ;
#8532 = ORIENTED_EDGE ( 'NONE', *, *, #23375, .F. ) ;
#8533 = CARTESIAN_POINT ( 'NONE',  ( 98.29820294273281434, -7.653668647304240125, 18.47759065023114644 ) ) ;
#8534 = CARTESIAN_POINT ( 'NONE',  ( -96.94475454972737793, 8.190683501884381101, -20.92018922311151741 ) ) ;
#8535 = CARTESIAN_POINT ( 'NONE',  ( 22.72189371635669985, 13.83659596079057685, 47.04833883279033557 ) ) ;
#8536 = ORIENTED_EDGE ( 'NONE', *, *, #24755, .T. ) ;
#8537 = ORIENTED_EDGE ( 'NONE', *, *, #21911, .F. ) ;
#8538 = CARTESIAN_POINT ( 'NONE',  ( 199.9999999999999432, -14.14213562373096345, -14.14213562373104871 ) ) ;
#8539 = CARTESIAN_POINT ( 'NONE',  ( 199.0214947048457077, -19.49260886005912141, -4.535603965114707314 ) ) ;
#8540 = CARTESIAN_POINT ( 'NONE',  ( -110.0791661673311950, -4.394837301258886164, 19.70411816748108436 ) ) ;
#8541 = FILL_AREA_STYLE_COLOUR ( '', #1512 ) ;
#8542 = AXIS2_PLACEMENT_3D ( 'NONE', #4182, #6033, #15997 ) ;
#8543 = CARTESIAN_POINT ( 'NONE',  ( 146.6084372240433993, -24.48358557860319706, -24.48358557860330720 ) ) ;
#8544 = DIRECTION ( 'NONE',  ( 0.000000000000000000, 0.000000000000000000, 1.000000000000000000 ) ) ;
#8545 = CARTESIAN_POINT ( 'NONE',  ( -89.91498783730511946, -8.087768383079360746, -20.43892340026755150 ) ) ;
#8546 = CARTESIAN_POINT ( 'NONE',  ( -162.0762913951021176, 40.00000000000042633, -41.69427287672947102 ) ) ;
#8547 = CARTESIAN_POINT ( 'NONE',  ( -280.0000000000000568, 39.99999999999976552, 20.00000000000043343 ) ) ;
#8548 = CARTESIAN_POINT ( 'NONE',  ( -639.6132534865922707, 29.31434396970803036, 27.21671984979430547 ) ) ;
#8549 = VECTOR ( 'NONE', #1404, 1000.000000000000000 ) ;
#8550 = CARTESIAN_POINT ( 'NONE',  ( 200.0000000000000000, -52.49999999999992895, -52.49999999999999289 ) ) ;
#8551 = CARTESIAN_POINT ( 'NONE',  ( 199.0085879884812243, 19.99611484057871280, 0.3390174452003563710 ) ) ;
#8552 = CARTESIAN_POINT ( 'NONE',  ( -189.2667466962307401, 17.97628569363215689, 43.39859272266379975 ) ) ;
#8553 = CARTESIAN_POINT ( 'NONE',  ( 4.995406935893297984, -39.06748935135205869, 17.50105314357158193 ) ) ;
#8554 = CARTESIAN_POINT ( 'NONE',  ( -102.4068193528169957, 8.735227608996499526, 20.17396017424870536 ) ) ;
#8555 = CARTESIAN_POINT ( 'NONE',  ( 136.1360204305621266, -3.511608612530682905, 3.511608612530666917 ) ) ;
#8556 = CARTESIAN_POINT ( 'NONE',  ( 98.29820294267869940, -15.90088694521850776, 12.38338430224809983 ) ) ;
#8557 = VECTOR ( 'NONE', #13308, 1000.000000000000000 ) ;
#8558 = CARTESIAN_POINT ( 'NONE',  ( -162.0762913951020892, -29.48230308784744125, -29.48230308784792442 ) ) ;
#8559 = CARTESIAN_POINT ( 'NONE',  ( -199.9999999999999432, 45.24754806069008595, -21.40989205436294540 ) ) ;
#8560 = CARTESIAN_POINT ( 'NONE',  ( -135.8532207217289738, 9.153146818113548022, 40.00000000000002132 ) ) ;
#8561 = CARTESIAN_POINT ( 'NONE',  ( -162.0762913951021176, 57.76657433523994456, -1.198031840315424867 ) ) ;
#8562 = AXIS2_PLACEMENT_3D ( 'NONE', #171, #16265, #24394 ) ;
#8563 = CARTESIAN_POINT ( 'NONE',  ( -213.1075012329537230, -13.71589010951915810, 0.000000000000000000 ) ) ;
#8564 = CARTESIAN_POINT ( 'NONE',  ( -608.4139831770295359, 33.82757453087469912, -29.68732721380340678 ) ) ;
#8565 = CARTESIAN_POINT ( 'NONE',  ( -91.56559293963834989, 1.671088883502053755E-13, -17.32597176626811120 ) ) ;
#8566 = CARTESIAN_POINT ( 'NONE',  ( 199.0060256982278588, 8.174003731485944613, -18.24926009350555134 ) ) ;
#8567 = CARTESIAN_POINT ( 'NONE',  ( 128.5824617753799544, -11.99766463964432717, 28.96492468983260338 ) ) ;
#8568 = ORIENTED_EDGE ( 'NONE', *, *, #22836, .F. ) ;
#8569 = VERTEX_POINT ( 'NONE', #14955 ) ;
#8570 = CARTESIAN_POINT ( 'NONE',  ( -213.1075012329537230, 13.71589010951907817, 40.00000000000002132 ) ) ;
#8571 = CARTESIAN_POINT ( 'NONE',  ( -200.0000000000000000, 61.50000000000009948, -66.50000000000005684 ) ) ;
#8572 = AXIS2_PLACEMENT_3D ( 'NONE', #17426, #3087, #13435 ) ;
#8573 = CARTESIAN_POINT ( 'NONE',  ( 19.06497207195980792, 66.60410523465830579, -10.03556273973354251 ) ) ;
#8574 = CARTESIAN_POINT ( 'NONE',  ( 90.68848816928600343, 21.08311784208570572, -9.291443205936941396 ) ) ;
#8575 = ADVANCED_FACE ( 'NONE', ( #23091 ), #17084, .T. ) ;
#8576 = B_SPLINE_CURVE_WITH_KNOTS ( 'NONE', 3,
 ( #9472, #25852, #15708, #23833, #5615, #13721, #24380, #9870, #10136, #12391, #26261, #8396, #1898, #5744, #16252, #10003, #17973, #6275, #18380, #5881, #1762, #3899, #16115, #26119, #2288, #23968, #25, #13849, #18240, #8136, #21984, #24245, #18110, #7861, #3755, #22120, #6018, #7997, #15980, #20253, #14126, #20516, #289, #6144, #4169, #11997, #22254, #4031, #14255, #24108, #10396, #22393, #12263, #12131, #13988, #20120, #2034, #20387, #11860, #18511, #19980, #2162, #10272, #159, #8263, #16383, #24516, #14390, #22521, #4301, #2698, #25048, #4424, #14643, #12929, #24914, #695, #16913, #8801, #15045, #18781, #12657, #21178, #25178, #564, #12517, #10803, #10937, #14518, #6928, #2422, #17043, #8668, #22782, #6799, #20783, #6402, #23176, #18913, #4955, #10531, #2554, #2952, #14910, #4561, #18644, #23052, #10670 ),
 .UNSPECIFIED., .F., .F.,
 ( 4, 2, 1, 2, 2, 2, 2, 2, 1, 2, 2, 2, 2, 2, 2, 2, 1, 2, 2, 2, 2, 2, 1, 2, 2, 2, 2, 2, 2, 2, 2, 2, 2, 2, 1, 2, 2, 2, 1, 2, 2, 2, 2, 2, 2, 2, 1, 2, 2, 2, 2, 2, 1, 2, 2, 2, 2, 4 ),
 ( 0.5000000000000000000, 0.5312500000000004441, 0.5390625000000005551, 0.5429687500000005551, 0.5468750000000005551, 0.5625000000000005551, 0.5703125000000005551, 0.5781250000000005551, 0.5859375000000005551, 0.5898437500000006661, 0.5937500000000006661, 0.6015625000000006661, 0.6093750000000006661, 0.6171875000000007772, 0.6250000000000007772, 0.6406250000000008882, 0.6484375000000008882, 0.6523437500000008882, 0.6562500000000008882, 0.6718750000000008882, 0.6796875000000008882, 0.6875000000000008882, 0.6953125000000008882, 0.6992187500000008882, 0.7031250000000009992, 0.7187500000000008882, 0.7265625000000008882, 0.7343750000000008882, 0.7500000000000008882, 0.7578125000000008882, 0.7656250000000008882, 0.7812500000000008882, 0.7890625000000008882, 0.7968750000000008882, 0.8046875000000008882, 0.8085937500000008882, 0.8125000000000008882, 0.8281250000000008882, 0.8359375000000008882, 0.8398437500000007772, 0.8437500000000006661, 0.8515625000000006661, 0.8593750000000006661, 0.8671875000000005551, 0.8750000000000004441, 0.9062500000000002220, 0.9140625000000002220, 0.9179687500000001110, 0.9218750000000000000, 0.9375000000000000000, 0.9453125000000000000, 0.9531250000000000000, 0.9609375000000000000, 0.9648437500000000000, 0.9687500000000000000, 0.9765625000000000000, 0.9843750000000000000, 1.000000000000000000 ),
 .UNSPECIFIED. ) ;
#8577 = CARTESIAN_POINT ( 'NONE',  ( -114.4364955367314707, 8.064892380844273845, -20.29001642038674902 ) ) ;
#8578 = DIRECTION ( 'NONE',  ( 0.000000000000000000, 1.000000000000000000, 0.000000000000000000 ) ) ;
#8579 = CARTESIAN_POINT ( 'NONE',  ( 199.9999999999999716, 15.97866926103663765, -10.28159943737610860 ) ) ;
#8580 = CARTESIAN_POINT ( 'NONE',  ( 170.0000000000000853, -9.369682556672300322, 22.62041470344878746 ) ) ;
#8581 = CARTESIAN_POINT ( 'NONE',  ( 146.6084372240433709, -52.76785682606510619, -3.800685668859292043 ) ) ;
#8582 = CARTESIAN_POINT ( 'NONE',  ( 130.8568914410475372, 24.07718906447210472, 24.07718906447249907 ) ) ;
#8583 = DIRECTION ( 'NONE',  ( 0.01051738792039683817, -0.9166396752530959757, -0.3995761383056185556 ) ) ;
#8584 = CARTESIAN_POINT ( 'NONE',  ( 163.1118516004056573, 40.00000000000017764, -12.73709011382432976 ) ) ;
#8585 = CARTESIAN_POINT ( 'NONE',  ( -100.7734535825088500, 16.03295912088691821, 16.03295912088721309 ) ) ;
#8586 = CARTESIAN_POINT ( 'NONE',  ( 8.517493190815724091, 14.17913040910384836, 49.32792454093237211 ) ) ;
#8587 = CARTESIAN_POINT ( 'NONE',  ( -238.4067589809705794, 0.6820004457912757223, 0.6820004457913219076 ) ) ;
#8588 = ADVANCED_FACE ( 'NONE', ( #13345 ), #25085, .F. ) ;
#8589 = CARTESIAN_POINT ( 'NONE',  ( -105.3755690713226727, -12.89780903124413847, 12.89780903124398037 ) ) ;
#8590 = CARTESIAN_POINT ( 'NONE',  ( -91.56559293963836410, 22.67402823373189946, -0.000000000000000000 ) ) ;
#8591 = EDGE_CURVE ( 'NONE', #7950, #5117, #21347, .T. ) ;
#8593 = CARTESIAN_POINT ( 'NONE',  ( -91.56559293963834989, -7.976292724337646577E-14, 17.32597176626811120 ) ) ;
#8592 = CARTESIAN_POINT ( 'NONE',  ( 91.82158438592158234, -40.45024623143936537, -16.11829626348475131 ) ) ;
#8594 = CARTESIAN_POINT ( 'NONE',  ( -30.26275506840325136, 29.48230279907760121, 27.08623969584625613 ) ) ;
#8595 = CARTESIAN_POINT ( 'NONE',  ( 23.40652632867984195, 42.84715492600962250, -23.33303889678548160 ) ) ;
#8596 = FACE_OUTER_BOUND ( 'NONE', #1988, .T. ) ;
#8597 = CARTESIAN_POINT ( 'NONE',  ( -91.56559293963834989, -44.31723036834903695, 12.25131212657476709 ) ) ;
#8598 = CARTESIAN_POINT ( 'NONE',  ( 4.995406935893288214, 55.24977328853207581, 40.00000000000002132 ) ) ;
#8599 =( BOUNDED_CURVE ( )  B_SPLINE_CURVE ( 3, ( #19057, #2843, #8814, #10951, #10815, #839, #4835 ),
 .UNSPECIFIED., .F., .F. ) 
 B_SPLINE_CURVE_WITH_KNOTS ( ( 4, 3, 4 ),
 ( 0.007504510840757262248, 0.02318599846099208411, 0.03886748608122998772 ),
 .UNSPECIFIED. ) 
 CURVE ( )  GEOMETRIC_REPRESENTATION_ITEM ( )  RATIONAL_B_SPLINE_CURVE ( ( 0.5852718452494399815, 0.6660804010233956074, 0.8043231192735822432, 1.000000000000000000, 0.8043231192735437185, 0.6660804010233410954, 0.5852718452493922419 ) ) 
 REPRESENTATION_ITEM ( '' )  );
#8600 = CARTESIAN_POINT ( 'NONE',  ( -4.558244102846159329, -46.81081390833291067, 13.79151199599502675 ) ) ;
#8601 = CARTESIAN_POINT ( 'NONE',  ( -198.0356074513804572, 55.37879056871320671, 40.00000000000002132 ) ) ;
#8602 = ORIENTED_EDGE ( 'NONE', *, *, #19395, .T. ) ;
#8603 = CARTESIAN_POINT ( 'NONE',  ( -199.9999999999999147, -49.28189405767606956, -14.17215463606684267 ) ) ;
#8604 = CARTESIAN_POINT ( 'NONE',  ( -198.0356074513804572, 10.87444709759714989, 10.87444709759722450 ) ) ;
#8605 = CARTESIAN_POINT ( 'NONE',  ( -3.443169733045703396, -17.93724492941688453, 43.30433998020581754 ) ) ;
#8606 = MANIFOLD_SOLID_BREP ( 'Chamfer3', #10037 ) ;
#8607 = CARTESIAN_POINT ( 'NONE',  ( -3.117754532606111795, 17.97158175134361002, -43.38723640139075854 ) ) ;
#8608 = CARTESIAN_POINT ( 'NONE',  ( 199.9999999999999716, -11.58333327279321701, 15.07704058621049548 ) ) ;
#8609 = CARTESIAN_POINT ( 'NONE',  ( -162.0762913951021176, 29.48230308784730980, 27.08623940707652622 ) ) ;
#8610 = CARTESIAN_POINT ( 'NONE',  ( -200.0000000000000000, -52.49999999999970868, 82.49999999999998579 ) ) ;
#8611 = CARTESIAN_POINT ( 'NONE',  ( -188.9524938556156712, -23.58789616779396425, 43.19211203808070820 ) ) ;
#8612 = CARTESIAN_POINT ( 'NONE',  ( -259.2033419157646676, 35.01439189186559275, -21.55415060305807984 ) ) ;
#8613 = CARTESIAN_POINT ( 'NONE',  ( 19.06497207195980792, -18.24870850772710540, -38.31983398719647482 ) ) ;
#8614 = DIRECTION ( 'NONE',  ( 1.000000000000000000, 1.836970198721030181E-16, 0.000000000000000000 ) ) ;
#8616 = CARTESIAN_POINT ( 'NONE',  ( 151.7948205124836250, 4.785054706301759886, -4.785054706301612448 ) ) ;
#8615 = CARTESIAN_POINT ( 'NONE',  ( 91.82158438592158234, 12.16597498397756993, 12.16597498397776356 ) ) ;
#8617 = CARTESIAN_POINT ( 'NONE',  ( -280.0000000000000568, 42.42640687119265408, 14.14213562373147504 ) ) ;
#8618 = CARTESIAN_POINT ( 'NONE',  ( -30.26275506840322649, -41.69427246844630019, -2.449293598294708485E-15 ) ) ;
#8619 = CARTESIAN_POINT ( 'NONE',  ( 200.0000000000000000, 19.99999999999995737, 40.00000000000002132 ) ) ;
#8620 = CARTESIAN_POINT ( 'NONE',  ( -30.26275506840324070, -40.00000000000001421, -1.694272468446678559 ) ) ;
#8621 = CARTESIAN_POINT ( 'NONE',  ( 170.2234770963711128, 39.20704971665398375, -17.36149277826984871 ) ) ;
#8622 = CARTESIAN_POINT ( 'NONE',  ( -100.0968563617870899, 20.41799937589586378, -8.893120081528337550 ) ) ;
#8623 = CARTESIAN_POINT ( 'NONE',  ( 184.8905102610680444, 14.79361573936424890, -41.77492675555986068 ) ) ;
#8624 = CARTESIAN_POINT ( 'NONE',  ( 136.1360204305621266, 24.77266263493138965, -24.77266263493110188 ) ) ;
#8625 = ORIENTED_EDGE ( 'NONE', *, *, #5241, .T. ) ;
#8626 = CARTESIAN_POINT ( 'NONE',  ( -259.2033419157646676, -6.730120644403667640, 49.83842185052029805 ) ) ;
#8627 = CARTESIAN_POINT ( 'NONE',  ( -198.0012279374161324, -14.15883993131235030, -49.19397028145281325 ) ) ;
#8628 = CARTESIAN_POINT ( 'NONE',  ( -259.2033419157646676, 35.01439189186528722, 21.55415060305857011 ) ) ;
#8629 = CARTESIAN_POINT ( 'NONE',  ( -2.164901439741091060, -43.53794903249359294, -23.84421257765930591 ) ) ;
#8630 = EDGE_LOOP ( 'NONE', ( #21454, #2660, #2620, #16915 ) ) ;
#8631 = CARTESIAN_POINT ( 'NONE',  ( 12.01361943528962151, -49.30661675909293962, -14.17591515420096648 ) ) ;
#8632 = CARTESIAN_POINT ( 'NONE',  ( -87.13361725327074225, -15.19799821270821560, -15.19799821270861884 ) ) ;
#8633 = EDGE_CURVE ( 'NONE', #15830, #17701, #24958, .T. ) ;
#8634 = ORIENTED_EDGE ( 'NONE', *, *, #13844, .F. ) ;
#8635 = CARTESIAN_POINT ( 'NONE',  ( 199.9999999999998295, 8.257913856993376100, -17.11264870637372226 ) ) ;
#8636 = DIRECTION ( 'NONE',  ( 0.000000000000000000, -0.3028247695821851271, 0.9530462522498561739 ) ) ;
#8637 = EDGE_CURVE ( 'NONE', #20847, #7865, #1085, .T. ) ;
#8638 = CARTESIAN_POINT ( 'NONE',  ( -86.96347745069644475, 18.24025645688351105, 2.449293598294708485E-15 ) ) ;
#8639 = CARTESIAN_POINT ( 'NONE',  ( -105.3755690713226585, -43.67073346367964604, -12.89780903124457545 ) ) ;
#8640 = CARTESIAN_POINT ( 'NONE',  ( 199.0164010208656009, 13.53619804287660777, 14.72436343555392035 ) ) ;
#8641 = B_SPLINE_CURVE_WITH_KNOTS ( 'NONE', 3,
 ( #14412, #10554, #6689, #4322, #46, #2309, #10417, #6555 ),
 .UNSPECIFIED., .F., .F.,
 ( 4, 2, 2, 4 ),
 ( 0.000000000000000000, 0.002089226651506802951, 0.004178453303013605034, 0.008356906606027208334 ),
 .UNSPECIFIED. ) ;
#8642 = CARTESIAN_POINT ( 'NONE',  ( -280.0000000000000568, -14.14213562373137556, 42.42640687119276066 ) ) ;
#8643 = CARTESIAN_POINT ( 'NONE',  ( -135.8532207217289738, -1.351063376314938213E-13, 30.84685318188645553 ) ) ;
#8644 = CARTESIAN_POINT ( 'NONE',  ( 14.38125909742180220, 39.99999999999997158, 15.17850393972647716 ) ) ;
#8645 = DIRECTION ( 'NONE',  ( 1.000000000000000000, -1.937599346585394162E-16, -0.000000000000000000 ) ) ;
#8646 = CARTESIAN_POINT ( 'NONE',  ( 184.8905102610680444, 20.92133201514447549, 0.000000000000000000 ) ) ;
#8647 = B_SPLINE_CURVE_WITH_KNOTS ( 'NONE', 3,
 ( #18909, #14777, #24641, #16773, #12787, #12513, #8392, #2693 ),
 .UNSPECIFIED., .F., .F.,
 ( 4, 2, 2, 4 ),
 ( 0.0002291277466111981624, 0.002289782534336058661, 0.004350437322060919133, 0.008471746897510642679 ),
 .UNSPECIFIED. ) ;
#8648 = CARTESIAN_POINT ( 'NONE',  ( 184.8905102610680444, 14.79361573936396113, -14.79361573936377461 ) ) ;
#8649 = CARTESIAN_POINT ( 'NONE',  ( -56.48582580120558561, -30.84685318188645553, -40.00000000000002132 ) ) ;
#8650 = CARTESIAN_POINT ( 'NONE',  ( 136.1360204305621266, -3.511608612530682905, 3.511608612530666917 ) ) ;
#8651 = CARTESIAN_POINT ( 'NONE',  ( -88.39148973765142614, -8.577159256668775100, 19.92926839984414755 ) ) ;
#8652 = DIRECTION ( 'NONE',  ( -1.000000000000000000, 0.000000000000000000, 0.000000000000000000 ) ) ;
#8653 = CARTESIAN_POINT ( 'NONE',  ( -135.8532207217289738, 40.00000000000031974, -30.84685318188603986 ) ) ;
#8654 = CARTESIAN_POINT ( 'NONE',  ( -86.96347745069643054, -40.00000000000009948, 18.24025645688337960 ) ) ;
#8655 = CARTESIAN_POINT ( 'NONE',  ( -105.3755690713226727, -15.38646221621786481, -15.38646221621789856 ) ) ;
#8656 = LINE ( 'NONE', #552, #13462 ) ;
#8657 = FACE_OUTER_BOUND ( 'NONE', #24237, .T. ) ;
#8658 = CARTESIAN_POINT ( 'NONE',  ( -30.26275506840322649, -29.48230279907810925, 29.48230279907778950 ) ) ;
#8659 = ORIENTED_EDGE ( 'NONE', *, *, #10442, .T. ) ;
#8661 = CARTESIAN_POINT ( 'NONE',  ( -62.72988123315526821, 25.36777511009515962, -10.50767649768604173 ) ) ;
#8660 = CARTESIAN_POINT ( 'NONE',  ( -77.70896657118109374, -5.469334093952031850, -21.30899064119132547 ) ) ;
#8662 = CARTESIAN_POINT ( 'NONE',  ( 140.2235668266256710, 30.42137084504312128, -12.60094438999823296 ) ) ;
#8663 = CARTESIAN_POINT ( 'NONE',  ( 200.0000000000000000, -19.99999999999988631, -40.00000000000002132 ) ) ;
#8664 = CARTESIAN_POINT ( 'NONE',  ( -86.95492415319874624, -20.33918386409409962, -6.698383215768170196 ) ) ;
#8665 = CARTESIAN_POINT ( 'NONE',  ( -162.0762913951020892, 1.198031840385732849, -1.198031840385733515 ) ) ;
#8666 = VERTEX_POINT ( 'NONE', #17340 ) ;
#8667 = EDGE_LOOP ( 'NONE', ( #12093, #8060, #8169, #26349 ) ) ;
#8668 = CARTESIAN_POINT ( 'NONE',  ( 199.9999999999999432, -7.568351747471193214, 17.44130164783803139 ) ) ;
#8669 = CARTESIAN_POINT ( 'NONE',  ( -105.4741150117382062, 8.366608964593805098, -19.60045294982731079 ) ) ;
#8670 = CARTESIAN_POINT ( 'NONE',  ( 17.65190073993491637, 24.35922420889580664, 44.23515346912942192 ) ) ;
#8671 = ORIENTED_EDGE ( 'NONE', *, *, #16818, .F. ) ;
#8672 = ADVANCED_FACE ( 'NONE', ( #15343 ), #18820, .T. ) ;
#8673 = ORIENTED_EDGE ( 'NONE', *, *, #6472, .T. ) ;
#8674 = CARTESIAN_POINT ( 'NONE',  ( 151.7948205124836534, -51.78348778862535795, 4.785054706298367044 ) ) ;
#8675 = CARTESIAN_POINT ( 'NONE',  ( 199.0238156666156044, -19.96322609118500324, 1.315852278599464631 ) ) ;
#8676 = CARTESIAN_POINT ( 'NONE',  ( -105.3394646353391266, -5.712077376943455853, 20.62740382081718238 ) ) ;
#8677 = CARTESIAN_POINT ( 'NONE',  ( -192.9588430854690273, 10.23066800231970319, 66.79921049724369198 ) ) ;
#8678 = DIRECTION ( 'NONE',  ( -0.000000000000000000, 0.000000000000000000, 1.000000000000000000 ) ) ;
#8679 = CARTESIAN_POINT ( 'NONE',  ( 4.995406935893283773, 39.99999999999997158, 15.24977328854846803 ) ) ;
#8680 = CARTESIAN_POINT ( 'NONE',  ( -93.12335834970889437, 6.205946304515388538E-14, -22.67402823373191723 ) ) ;
#8681 = ADVANCED_FACE ( 'NONE', ( #9100 ), #2628, .T. ) ;
#8682 = EDGE_CURVE ( 'NONE', #23802, #18072, #13389, .T. ) ;
#8683 = CARTESIAN_POINT ( 'NONE',  ( -4.039451493210489907, 13.82811171175507603, -46.99046209229789639 ) ) ;
#8684 = CARTESIAN_POINT ( 'NONE',  ( 151.7948205124836534, 40.00000000000012079, -6.767089262348609857 ) ) ;
#8685 = CARTESIAN_POINT ( 'NONE',  ( -192.9588430854689989, 1.161019517985663313E-13, -14.46834944099969533 ) ) ;
#8686 = CARTESIAN_POINT ( 'NONE',  ( -656.1498148884619468, 39.37764844114641960, 7.046424841349725021 ) ) ;
#8687 = CARTESIAN_POINT ( 'NONE',  ( -87.13361725327077068, 14.22820505596910756, 16.16779136944769846 ) ) ;
#8688 = CARTESIAN_POINT ( 'NONE',  ( 199.0060120359516986, 18.22327268582330007, -8.235267977567980680 ) ) ;
#8689 = CARTESIAN_POINT ( 'NONE',  ( -188.8383598209451861, 17.93083279444609701, 43.28885971699654789 ) ) ;
#8690 = CARTESIAN_POINT ( 'NONE',  ( -86.86493150571114086, -7.943527260496002107, 19.77569912839178912 ) ) ;
#8691 = CARTESIAN_POINT ( 'NONE',  ( -77.90255099906769942, -8.644468104261466834, -20.04994828523962980 ) ) ;
#8692 = CARTESIAN_POINT ( 'NONE',  ( 57.59792236341148453, 1.722363176414758668, 54.84617931850880268 ) ) ;
#8693 = CARTESIAN_POINT ( 'NONE',  ( -109.1264249741460617, 13.72187187123938656, 33.12752917269246211 ) ) ;
#8694 = CARTESIAN_POINT ( 'NONE',  ( 163.1118516004056573, 47.56205970284970164, -9.006482792073828847 ) ) ;
#8695 = CARTESIAN_POINT ( 'NONE',  ( -655.1625848890473662, 39.92241353143312921, 20.79055835074375480 ) ) ;
#8696 = CARTESIAN_POINT ( 'NONE',  ( -213.1075012329537230, -13.71589010951915810, 0.000000000000000000 ) ) ;
#8697 = CARTESIAN_POINT ( 'NONE',  ( -198.0356074513804572, 39.15871834505887250, 17.40982414986519089 ) ) ;
#8698 = CARTESIAN_POINT ( 'NONE',  ( -238.4067589809705794, -0.9644942799826263791, 40.00000000000002132 ) ) ;
#8699 = CARTESIAN_POINT ( 'NONE',  ( -601.6618123970941951, 37.95920655747095651, -24.18560810059053168 ) ) ;
#8700 = ORIENTED_EDGE ( 'NONE', *, *, #19855, .F. ) ;
#8701 = CARTESIAN_POINT ( 'NONE',  ( -208.1127848780264742, -39.99999999999990763, -15.00245453012711394 ) ) ;
#8702 = CARTESIAN_POINT ( 'NONE',  ( -265.0000000000000000, 9.999999999999952038, 1.224646799147346551E-15 ) ) ;
#8703 = CARTESIAN_POINT ( 'NONE',  ( 98.29820294273281434, -7.653668647304240125, 18.47759065023114644 ) ) ;
#8704 = ORIENTED_EDGE ( 'NONE', *, *, #1436, .F. ) ;
#8705 = ORIENTED_EDGE ( 'NONE', *, *, #10544, .F. ) ;
#8706 = CARTESIAN_POINT ( 'NONE',  ( -91.56559293963834989, 17.32597176626809343, 2.449293598294708485E-15 ) ) ;
#8707 = DIRECTION ( 'NONE',  ( 1.000000000000000000, -0.000000000000000000, -0.000000000000000000 ) ) ;
#8708 =( BOUNDED_SURFACE ( )  B_SPLINE_SURFACE ( 3, 3, ( 
 ( #11363, #23730, #21612, #19481, #22015, #25492, #11484, #7241, #11617, #1267, #17480, #17604, #19612, #7495, #7368, #17735, #5775, #25876, #15480, #3649, #13745, #23607, #5511, #15735, #23861, #5639, #23485, #1657, #15606, #3786 ),
 ( #21742, #3517, #26017, #7754, #18140, #16417, #2061, #4196, #20417, #12289, #18543, #22284, #325, #6432, #55, #9898, #16011, #22548, #24278, #18002, #24137, #4329, #20547, #8290, #5909, #4454, #10167, #20009, #12419, #22420 ),
 ( #10425, #26288, #18270, #2194, #8426, #10301, #14019, #16546, #18408, #183, #14152, #22148, #20146, #8027, #24545, #1794, #24676, #26148, #14550, #12026, #2317, #4058, #3928, #6173, #14418, #7892, #22680, #1924, #10031, #12160 ),
 ( #6300, #8166, #16144, #6047, #20282, #16279, #24407, #14283, #25339, #18949, #2451, #8565, #15076, #16812, #10561, #16679, #23207, #13094, #859, #24810, #23337, #20950, #12549, #4988, #14948, #7096, #12830, #22944, #9094, #2728 ),
 ( #20681, #17201, #10704, #19078, #15210, #18674, #12959, #594, #17077, #10833, #8968, #460, #25211, #8834, #6562, #730, #21212, #4854, #6959, #20817, #16943, #989, #14678, #22813, #4590, #4723, #2589, #21078, #12687, #25078 ),
 ( #6829, #18814, #2984, #24950, #8701, #10970, #23082, #2863, #11091, #6698, #19207, #14811, #23581, #9223, #9738, #15839, #7467, #21339, #17578, #15582, #3110, #5358, #9347, #17332, #5113, #3234, #13465, #17455, #25466, #1373 ),
 ( #19846, #7727, #23706, #11588, #11339, #25595, #3357, #21713, #13217, #5485, #7217, #11215, #1631, #1114, #19329, #25715, #13585, #15333, #19454, #1498, #21586, #3491, #19710, #9604, #3617, #7341, #11727, #17840, #11459, #23461 ) ),
 .UNSPECIFIED., .T., .F., .T. ) 
 B_SPLINE_SURFACE_WITH_KNOTS ( ( 4, 3, 4 ),
 ( 4, 2, 2, 2, 2, 2, 2, 2, 2, 2, 2, 2, 2, 2, 4 ),
 ( 0.000000000000000000, 0.5000000000000000000, 1.000000000000000000 ),
 ( 0.000000000000000000, 0.1357259735107005372, 0.1651108541090157700, 0.1944957347073310028, 0.3598804999793158710, 0.3867117631979620773, 0.4135430264166082281, 0.5789277916885930964, 0.6062785021374117456, 0.6336292125862302838, 0.8508620842112317728, 0.8814014469398914198, 0.9119408096685510667, 0.9559704048342755334, 1.000000000000000000 ),
 .UNSPECIFIED. ) 
 GEOMETRIC_REPRESENTATION_ITEM ( )  RATIONAL_B_SPLINE_SURFACE ( (
 ( 1.000000000000000000, 1.000000000000000000, 1.000000000000000000, 1.000000000000000000, 1.000000000000000000, 1.000000000000000000, 1.000000000000000000, 1.000000000000000000, 1.000000000000000000, 1.000000000000000000, 1.000000000000000000, 1.000000000000000000, 1.000000000000000000, 1.000000000000000000, 1.000000000000000000, 1.000000000000000000, 1.000000000000000000, 1.000000000000000000, 1.000000000000000000, 1.000000000000000000, 1.000000000000000000, 1.000000000000000000, 1.000000000000000000, 1.000000000000000000, 1.000000000000000000, 1.000000000000000000, 1.000000000000000000, 1.000000000000000000, 1.000000000000000000, 1.000000000000000000),
 ( 0.3333333333333333703, 0.3333333333333333703, 0.3333333333333333703, 0.3333333333333333703, 0.3333333333333333703, 0.3333333333333333703, 0.3333333333333333703, 0.3333333333333333703, 0.3333333333333333703, 0.3333333333333333703, 0.3333333333333333703, 0.3333333333333333703, 0.3333333333333333703, 0.3333333333333333703, 0.3333333333333333703, 0.3333333333333333703, 0.3333333333333333703, 0.3333333333333333703, 0.3333333333333333703, 0.3333333333333333703, 0.3333333333333333703, 0.3333333333333333703, 0.3333333333333333703, 0.3333333333333333703, 0.3333333333333333703, 0.3333333333333333703, 0.3333333333333333703, 0.3333333333333333703, 0.3333333333333333703, 0.3333333333333333703),
 ( 0.3333333333333333703, 0.3333333333333333703, 0.3333333333333333703, 0.3333333333333333703, 0.3333333333333333703, 0.3333333333333333703, 0.3333333333333333703, 0.3333333333333333703, 0.3333333333333333703, 0.3333333333333333703, 0.3333333333333333703, 0.3333333333333333703, 0.3333333333333333703, 0.3333333333333333703, 0.3333333333333333703, 0.3333333333333333703, 0.3333333333333333703, 0.3333333333333333703, 0.3333333333333333703, 0.3333333333333333703, 0.3333333333333333703, 0.3333333333333333703, 0.3333333333333333703, 0.3333333333333333703, 0.3333333333333333703, 0.3333333333333333703, 0.3333333333333333703, 0.3333333333333333703, 0.3333333333333333703, 0.3333333333333333703),
 ( 1.000000000000000000, 1.000000000000000000, 1.000000000000000000, 1.000000000000000000, 1.000000000000000000, 1.000000000000000000, 1.000000000000000000, 1.000000000000000000, 1.000000000000000000, 1.000000000000000000, 1.000000000000000000, 1.000000000000000000, 1.000000000000000000, 1.000000000000000000, 1.000000000000000000, 1.000000000000000000, 1.000000000000000000, 1.000000000000000000, 1.000000000000000000, 1.000000000000000000, 1.000000000000000000, 1.000000000000000000, 1.000000000000000000, 1.000000000000000000, 1.000000000000000000, 1.000000000000000000, 1.000000000000000000, 1.000000000000000000, 1.000000000000000000, 1.000000000000000000),
 ( 0.3333333333333333703, 0.3333333333333333703, 0.3333333333333333703, 0.3333333333333333703, 0.3333333333333333703, 0.3333333333333333703, 0.3333333333333333703, 0.3333333333333333703, 0.3333333333333333703, 0.3333333333333333703, 0.3333333333333333703, 0.3333333333333333703, 0.3333333333333333703, 0.3333333333333333703, 0.3333333333333333703, 0.3333333333333333703, 0.3333333333333333703, 0.3333333333333333703, 0.3333333333333333703, 0.3333333333333333703, 0.3333333333333333703, 0.3333333333333333703, 0.3333333333333333703, 0.3333333333333333703, 0.3333333333333333703, 0.3333333333333333703, 0.3333333333333333703, 0.3333333333333333703, 0.3333333333333333703, 0.3333333333333333703),
 ( 0.3333333333333333703, 0.3333333333333333703, 0.3333333333333333703, 0.3333333333333333703, 0.3333333333333333703, 0.3333333333333333703, 0.3333333333333333703, 0.3333333333333333703, 0.3333333333333333703, 0.3333333333333333703, 0.3333333333333333703, 0.3333333333333333703, 0.3333333333333333703, 0.3333333333333333703, 0.3333333333333333703, 0.3333333333333333703, 0.3333333333333333703, 0.3333333333333333703, 0.3333333333333333703, 0.3333333333333333703, 0.3333333333333333703, 0.3333333333333333703, 0.3333333333333333703, 0.3333333333333333703, 0.3333333333333333703, 0.3333333333333333703, 0.3333333333333333703, 0.3333333333333333703, 0.3333333333333333703, 0.3333333333333333703),
 ( 1.000000000000000000, 1.000000000000000000, 1.000000000000000000, 1.000000000000000000, 1.000000000000000000, 1.000000000000000000, 1.000000000000000000, 1.000000000000000000, 1.000000000000000000, 1.000000000000000000, 1.000000000000000000, 1.000000000000000000, 1.000000000000000000, 1.000000000000000000, 1.000000000000000000, 1.000000000000000000, 1.000000000000000000, 1.000000000000000000, 1.000000000000000000, 1.000000000000000000, 1.000000000000000000, 1.000000000000000000, 1.000000000000000000, 1.000000000000000000, 1.000000000000000000, 1.000000000000000000, 1.000000000000000000, 1.000000000000000000, 1.000000000000000000, 1.000000000000000000) ) ) 
 REPRESENTATION_ITEM ( '' )  SURFACE ( )  );
#8709 = FACE_OUTER_BOUND ( 'NONE', #4593, .T. ) ;
#8710 = FACE_OUTER_BOUND ( 'NONE', #23838, .T. ) ;
#8711 = CARTESIAN_POINT ( 'NONE',  ( -265.0000000000000000, 9.999999999999952038, 1.224646799147346551E-15 ) ) ;
#8712 = CARTESIAN_POINT ( 'NONE',  ( 199.9999999999998863, 12.52392839731578889, -14.30162278802013098 ) ) ;
#8713 = CARTESIAN_POINT ( 'NONE',  ( 199.9999999999999147, 3.090567748620505650, -18.74862269653256419 ) ) ;
#8714 = CARTESIAN_POINT ( 'NONE',  ( 91.82158438592158234, -40.45024623143936537, -16.11829626348475131 ) ) ;
#8715 = CARTESIAN_POINT ( 'NONE',  ( -100.7734535825088500, 16.03295912088691821, 16.03295912088721309 ) ) ;
#8716 = DIRECTION ( 'NONE',  ( 1.000000000000000000, 1.836970198721030427E-16, -0.000000000000000000 ) ) ;
#8717 = CARTESIAN_POINT ( 'NONE',  ( -192.9588430854690273, 40.00000000000014211, -14.46834944099927966 ) ) ;
#8718 = CARTESIAN_POINT ( 'NONE',  ( -30.26275506840324070, -1.198031551616016266, -1.198031551616031587 ) ) ;
#8719 = CARTESIAN_POINT ( 'NONE',  ( -213.1075012329537230, -13.71589010951915810, 0.000000000000000000 ) ) ;
#8720 = CARTESIAN_POINT ( 'NONE',  ( -280.0000000000000568, -42.42640687119295251, 14.14213562373088351 ) ) ;
#8721 = CARTESIAN_POINT ( 'NONE',  ( -135.8532207217289738, -21.81201906317788186, 21.81201906317762962 ) ) ;
#8722 = CARTESIAN_POINT ( 'NONE',  ( 199.0078462942310296, 19.92684364972848243, -1.695029663804312303 ) ) ;
#8724 = CARTESIAN_POINT ( 'NONE',  ( -213.1075012329537230, -8.703598725189323045E-14, 13.71589010951911902 ) ) ;
#8723 = CARTESIAN_POINT ( 'NONE',  ( 19.06497207195980792, -18.24870850772710540, -38.31983398719647482 ) ) ;
#8725 = CARTESIAN_POINT ( 'NONE',  ( 67.79414719548314849, 28.72755866874277686, -14.15005687142633839 ) ) ;
#8726 = CYLINDRICAL_SURFACE ( 'NONE', #11297, 5.000000000000046185 ) ;
#8727 = CARTESIAN_POINT ( 'NONE',  ( -259.2033419157646676, -35.01439189186554302, 21.55415060305832498 ) ) ;
#8728 = CARTESIAN_POINT ( 'NONE',  ( 19.06497207195980792, 14.19242893257840699, 40.00000000000002132 ) ) ;
#8729 = ORIENTED_EDGE ( 'NONE', *, *, #23316, .F. ) ;
#8730 = CARTESIAN_POINT ( 'NONE',  ( -0.5869797817515145510, -43.96874597321873779, 18.21245090264041266 ) ) ;
#8731 = AXIS2_PLACEMENT_3D ( 'NONE', #16754, #23028, #4666 ) ;
#8732 = CARTESIAN_POINT ( 'NONE',  ( -192.9588430854689989, 54.46834944099968823, 2.449293598294708485E-15 ) ) ;
#8733 = ORIENTED_EDGE ( 'NONE', *, *, #5398, .T. ) ;
#8734 = CARTESIAN_POINT ( 'NONE',  ( 20.59039453120235663, 23.90179120638680388, -43.61606461192713624 ) ) ;
#8735 = CARTESIAN_POINT ( 'NONE',  ( -105.3755690713226727, -15.38646221621786481, -15.38646221621789856 ) ) ;
#8736 = CARTESIAN_POINT ( 'NONE',  ( -3.534370630407254854, -17.92707699455397119, 43.27979241395971144 ) ) ;
#8737 = EDGE_CURVE ( 'NONE', #25916, #7784, #24001, .T. ) ;
#8738 = CARTESIAN_POINT ( 'NONE',  ( -4.061681315507501999, 13.82654462146623331, -46.98276670624658635 ) ) ;
#8739 = CARTESIAN_POINT ( 'NONE',  ( 199.0242480509055270, -19.84286657041863933, 2.617213520271152394 ) ) ;
#8740 = CARTESIAN_POINT ( 'NONE',  ( 0.2972598230769886718, 38.42060263243643448, 18.14793986248763957 ) ) ;
#8741 = CARTESIAN_POINT ( 'NONE',  ( -626.9846540392142060, 75.00000000000000000, -65.00000000000004263 ) ) ;
#8742 = CARTESIAN_POINT ( 'NONE',  ( -192.1964066538387783, -14.00508515770005147, 48.17614796926734755 ) ) ;
#8743 = CARTESIAN_POINT ( 'NONE',  ( -280.0000000000000568, 42.42640687119294540, -14.14213562373059041 ) ) ;
#8744 = CARTESIAN_POINT ( 'NONE',  ( -238.4067589809705794, -0.6820004457913680929, 0.6820004457913170226 ) ) ;
#8745 = CARTESIAN_POINT ( 'NONE',  ( -192.9588430854689989, 10.23066800230756712, -10.23066800230735396 ) ) ;
#8746 = CARTESIAN_POINT ( 'NONE',  ( -210.0000000000000284, 52.49999999999988631, -82.49999999999998579 ) ) ;
#8747 = AXIS2_PLACEMENT_3D ( 'NONE', #22162, #24555, #14162 ) ;
#8748 = VECTOR ( 'NONE', #25709, 1000.000000000000000 ) ;
#8750 = CARTESIAN_POINT ( 'NONE',  ( -213.1075012329537230, 66.26714140138673770, -9.698598906462034819 ) ) ;
#8749 = CARTESIAN_POINT ( 'NONE',  ( -213.1075012329537230, 18.58567234101174037, -37.98287015391222354 ) ) ;
#8751 = CARTESIAN_POINT ( 'NONE',  ( -238.4067589809705794, 57.25054294065799354, -0.6820004457334954973 ) ) ;
#8752 = CARTESIAN_POINT ( 'NONE',  ( 151.7948205124836534, -6.767089262349006873, 40.00000000000002132 ) ) ;
#8753 = CARTESIAN_POINT ( 'NONE',  ( -238.4067589809705794, 0.9644942799825385604, -40.00000000000002132 ) ) ;
#8754 = CARTESIAN_POINT ( 'NONE',  ( -30.26275506840325136, 29.48230279907798135, -27.08623969584585112 ) ) ;
#8755 =( BOUNDED_SURFACE ( )  B_SPLINE_SURFACE ( 3, 2, ( 
 ( #3554, #11396, #1305 ),
 ( #25658, #5424, #25275 ),
 ( #7281, #13527, #5049 ),
 ( #15516, #17644, #21781 ),
 ( #7404, #25785, #13280 ),
 ( #19142, #23646, #23522 ),
 ( #5294, #7025, #19518 ),
 ( #15398, #3423, #926 ),
 ( #21651, #13402, #3048 ),
 ( #1052, #11525, #21526 ),
 ( #19650, #7535, #21402 ),
 ( #23274, #3302, #1435 ),
 ( #9158, #15271, #9535 ),
 ( #9036, #25533, #9413 ),
 ( #15644, #17519, #23771 ),
 ( #11155, #17140, #5549 ),
 ( #13156, #13657, #25404 ),
 ( #21276, #19270, #5177 ),
 ( #3175, #17270, #7155 ),
 ( #23401, #11279, #19401 ),
 ( #1183, #9285, #17393 ),
 ( #20056, #8068, #10206 ),
 ( #20321, #26325, #22457 ),
 ( #94, #24176, #18042 ),
 ( #16187, #1835, #15908 ),
 ( #24320, #26055, #22056 ),
 ( #5951, #9936, #24041 ),
 ( #3830, #26197, #13922 ),
 ( #19781, #22192, #7934 ),
 ( #20183, #9805, #6213 ),
 ( #11797, #8202, #5817 ),
 ( #17912, #16320, #16050 ),
 ( #6085, #14190, #14061 ),
 ( #12066, #12199, #7792 ),
 ( #22324, #11931, #14324 ),
 ( #23902, #11655, #3967 ),
 ( #1968, #15774, #4099 ),
 ( #10073, #2097, #18177 ),
 ( #18312, #1567, #24444 ),
 ( #9672, #17776, #25919 ),
 ( #7663, #5678, #13784 ),
 ( #21917, #3690, #19916 ),
 ( #1700, #8605, #16584 ),
 ( #22982, #2763, #16980 ),
 ( #499, #18713, #4491 ),
 ( #20583, #8736, #24986 ),
 ( #24846, #12727, #16715 ),
 ( #6599, #14848, #14719 ),
 ( #363, #10740, #10337 ),
 ( #2357, #20454, #10602 ),
 ( #14458, #22851, #12456 ),
 ( #14982, #4760, #4236 ),
 ( #4626, #10471, #18851 ),
 ( #221, #24717, #6471 ),
 ( #12325, #20850, #2630 ),
 ( #630, #16855, #18446 ),
 ( #6736, #12864, #16458 ),
 ( #20982, #10870, #6866 ),
 ( #18986, #2229, #764 ),
 ( #8869, #25116, #8334 ) ),
 .UNSPECIFIED., .F., .F., .T. ) 
 B_SPLINE_SURFACE_WITH_KNOTS ( ( 4, 2, 2, 2, 2, 2, 2, 2, 2, 2, 2, 2, 2, 2, 2, 2, 2, 2, 2, 2, 2, 2, 2, 2, 2, 2, 2, 2, 2, 4 ),
 ( 3, 3 ),
 ( -6.934549977324601594E-05, 0.02465257023823465635, 0.04937448597624256169, 0.07409640171425047050, 0.08027688064875244944, 0.08066316058215883267, 0.08085630054886201734, 0.08090458554053781004, 0.08095287053221361662, 0.08104944051556520201, 0.08182200038237794071, 0.08336712011600344585, 0.08645735958325442838, 0.09263783851775639344, 0.09881831745225837238, 0.1019085569195093688, 0.1049987963867603513, 0.1111792753212623164, 0.1173597542557642953, 0.1177460341891706785, 0.1179391741558738632, 0.1179874591475496559, 0.1180357441392254625, 0.1181323141225770479, 0.1189048739893897866, 0.1204499937230152917, 0.1235402331902662743, 0.1482621489282741900, 0.1729840646662820780, 0.1977059804042899938 ),
 ( 0.000000000000000000, 1.000000000000000000 ),
 .UNSPECIFIED. ) 
 GEOMETRIC_REPRESENTATION_ITEM ( )  RATIONAL_B_SPLINE_SURFACE ( (
 ( 1.000000000000000000, 1.000000000000000000, 1.000000000000000000),
 ( 1.000000000000000000, 0.9999975583948276237, 1.000000000000000000),
 ( 1.000000000000000000, 0.9982436956964818586, 1.000000000000000000),
 ( 1.000000000000000000, 0.9910288481548262807, 1.000000000000000000),
 ( 1.000000000000000000, 0.9855714588515670505, 1.000000000000000000),
 ( 1.000000000000000000, 0.9705958323316278280, 1.000000000000000000),
 ( 1.000000000000000000, 0.9610788543733380651, 1.000000000000000000),
 ( 1.000000000000000000, 0.9462867046312647412, 1.000000000000000000),
 ( 1.000000000000000000, 0.9431828180755345015, 1.000000000000000000),
 ( 1.000000000000000000, 0.9397240291170321225, 1.000000000000000000),
 ( 1.000000000000000000, 0.9395199791395947297, 1.000000000000000000),
 ( 1.000000000000000000, 0.9392130141387216025, 1.000000000000000000),
 ( 1.000000000000000000, 0.9391105441325042769, 1.000000000000000000),
 ( 1.000000000000000000, 0.9389822709566328918, 1.000000000000000000),
 ( 1.000000000000000000, 0.9389566070380596097, 1.000000000000000000),
 ( 1.000000000000000000, 0.9389052606279760793, 1.000000000000000000),
 ( 1.000000000000000000, 0.9388799835492060986, 1.000000000000000000),
 ( 1.000000000000000000, 0.9388039637710071661, 1.000000000000000000),
 ( 1.000000000000000000, 0.9387533729070444144, 1.000000000000000000),
 ( 1.000000000000000000, 0.9382988607467089848, 1.000000000000000000),
 ( 1.000000000000000000, 0.9379005790853230939, 1.000000000000000000),
 ( 1.000000000000000000, 0.9367237203702156734, 1.000000000000000000),
 ( 1.000000000000000000, 0.9359625442025921727, 1.000000000000000000),
 ( 1.000000000000000000, 0.9337619511409316342, 1.000000000000000000),
 ( 1.000000000000000000, 0.9324064515427418209, 1.000000000000000000),
 ( 1.000000000000000000, 0.9287106072118640476, 1.000000000000000000),
 ( 1.000000000000000000, 0.9267422912947972380, 1.000000000000000000),
 ( 1.000000000000000000, 0.9239539123018306599, 1.000000000000000000),
 ( 1.000000000000000000, 0.9231338493906536824, 1.000000000000000000),
 ( 1.000000000000000000, 0.9228496048507791594, 1.000000000000000000),
 ( 1.000000000000000000, 0.9229135694615112628, 1.000000000000000000),
 ( 1.000000000000000000, 0.9233494155302143236, 1.000000000000000000),
 ( 1.000000000000000000, 0.9237209353788754518, 1.000000000000000000),
 ( 1.000000000000000000, 0.9252744993862994649, 1.000000000000000000),
 ( 1.000000000000000000, 0.9268968421604496521, 1.000000000000000000),
 ( 1.000000000000000000, 0.9311673748453518362, 1.000000000000000000),
 ( 1.000000000000000000, 0.9338157035273875195, 1.000000000000000000),
 ( 1.000000000000000000, 0.9370733336298756599, 1.000000000000000000),
 ( 1.000000000000000000, 0.9372665829346552568, 1.000000000000000000),
 ( 1.000000000000000000, 0.9375588533504852773, 1.000000000000000000),
 ( 1.000000000000000000, 0.9376566762263802701, 1.000000000000000000),
 ( 1.000000000000000000, 0.9377794499114608939, 1.000000000000000000),
 ( 1.000000000000000000, 0.9378038842964712130, 1.000000000000000000),
 ( 1.000000000000000000, 0.9378536652368906212, 1.000000000000000000),
 ( 1.000000000000000000, 0.9378785472098815079, 1.000000000000000000),
 ( 1.000000000000000000, 0.9379531676447474542, 1.000000000000000000),
 ( 1.000000000000000000, 0.9380028806225414462, 1.000000000000000000),
 ( 1.000000000000000000, 0.9384499917948422310, 1.000000000000000000),
 ( 1.000000000000000000, 0.9388452506063807990, 1.000000000000000000),
 ( 1.000000000000000000, 0.9400245377240871170, 1.000000000000000000),
 ( 1.000000000000000000, 0.9408020798629985748, 1.000000000000000000),
 ( 1.000000000000000000, 0.9431089717073132261, 1.000000000000000000),
 ( 1.000000000000000000, 0.9446123105950532395, 1.000000000000000000),
 ( 1.000000000000000000, 0.9578370004756148193, 1.000000000000000000),
 ( 1.000000000000000000, 0.9674308273343072972, 1.000000000000000000),
 ( 1.000000000000000000, 0.9828254127557660702, 1.000000000000000000),
 ( 1.000000000000000000, 0.9886239107116222558, 1.000000000000000000),
 ( 1.000000000000000000, 0.9967564037645807451, 1.000000000000000000),
 ( 1.000000000000000000, 0.9990872413561198151, 1.000000000000000000),
 ( 1.000000000000000000, 0.9997813423572990965, 1.000000000000000000) ) ) 
 REPRESENTATION_ITEM ( '' )  SURFACE ( )  );
#8756 = CARTESIAN_POINT ( 'NONE',  ( -89.91498783734905942, 20.43892340027597854, -8.087768383073672851 ) ) ;
#8757 = CARTESIAN_POINT ( 'NONE',  ( 192.4448373802101173, 14.14213562375922884, -42.42640687116488607 ) ) ;
#8758 = CARTESIAN_POINT ( 'NONE',  ( -188.8383598209457546, 43.28885971699691737, -17.93083279444630662 ) ) ;
#8759 = ORIENTED_EDGE ( 'NONE', *, *, #18586, .T. ) ;
#8760 = CARTESIAN_POINT ( 'NONE',  ( -208.1127848780264742, 67.17687982760683951, 10.60833733268317403 ) ) ;
#8761 = CARTESIAN_POINT ( 'NONE',  ( -102.4309680865787442, 8.733065089997754882, 20.17061239841417475 ) ) ;
#8762 = CARTESIAN_POINT ( 'NONE',  ( -105.3755690713226727, -12.89780903124413847, 12.89780903124398037 ) ) ;
#8763 = CARTESIAN_POINT ( 'NONE',  ( 11.71430589693571989, -44.87285427231137191, -24.82930166508382541 ) ) ;
#8764 = EDGE_CURVE ( 'NONE', #4257, #26122, #16803, .T. ) ;
#8765 = VERTEX_POINT ( 'NONE', #5623 ) ;
#8766 = CARTESIAN_POINT ( 'NONE',  ( 57.59792236341147031, -2.435789363418150444, 0.000000000000000000 ) ) ;
#8767 = CARTESIAN_POINT ( 'NONE',  ( -93.12335834970889437, -16.03295912088706388, -16.03295912088710651 ) ) ;
#8768 = CARTESIAN_POINT ( 'NONE',  ( 200.0000000000000000, 15.45062812681867825, -11.05917137904152625 ) ) ;
#8769 = AXIS2_PLACEMENT_3D ( 'NONE', #7995, #22252, #19494 ) ;
#8770 = CARTESIAN_POINT ( 'NONE',  ( -726.9846540392142060, 82.50000000000008527, 52.49999999999980105 ) ) ;
#8771 = CARTESIAN_POINT ( 'NONE',  ( 0.2972598230769930017, 54.33493731733936016, 40.00000000000002132 ) ) ;
#8772 = CARTESIAN_POINT ( 'NONE',  ( -259.2033419157646676, -6.730120644403663199, 6.730120644403451813 ) ) ;
#8773 = CARTESIAN_POINT ( 'NONE',  ( 199.0157948715101668, 14.36126147255820484, 13.92041998760680066 ) ) ;
#8774 = AXIS2_PLACEMENT_3D ( 'NONE', #3091, #1091, #9199 ) ;
#8775 = CARTESIAN_POINT ( 'NONE',  ( 136.1360204305621266, -3.511608612531119000, 53.05693388239312469 ) ) ;
#8776 = CARTESIAN_POINT ( 'NONE',  ( -91.56559293963836410, 39.99999999999994316, 17.32597176626825330 ) ) ;
#8777 = CARTESIAN_POINT ( 'NONE',  ( -280.0000000000000568, 40.00000000000004263, -19.99999999999987210 ) ) ;
#8778 = CARTESIAN_POINT ( 'NONE',  ( -105.2054292635175869, 15.19799821370233062, -15.19799821370219206 ) ) ;
#8779 = CARTESIAN_POINT ( 'NONE',  ( 0.2972598230770130412, -54.33493731733936016, -2.449293598294708485E-15 ) ) ;
#8781 = CARTESIAN_POINT ( 'NONE',  ( 14.38125909742181285, -10.73282306404727393, 10.73282306404716380 ) ) ;
#8780 = CARTESIAN_POINT ( 'NONE',  ( 23.46661716383002982, -23.32081713244383891, -42.82867125331112845 ) ) ;
#8782 = CARTESIAN_POINT ( 'NONE',  ( 146.6084372240433993, -5.374981219216945938, -2.449293598294708485E-15 ) ) ;
#8783 = CARTESIAN_POINT ( 'NONE',  ( 0.2972598230770100991, -38.42060263243686791, 38.42060263243645579 ) ) ;
#8784 = CARTESIAN_POINT ( 'NONE',  ( 158.3379117892985164, -10.98149362779622251, -26.51167085133963397 ) ) ;
#8785 = CARTESIAN_POINT ( 'NONE',  ( -114.7824662270011657, 14.65611376398968169, -16.64100530757652052 ) ) ;
#8786 = CARTESIAN_POINT ( 'NONE',  ( 0.2972598230770030492, 5.716321584140269555E-13, -54.33493731733936016 ) ) ;
#8787 = CARTESIAN_POINT ( 'NONE',  ( 57.59792236341147031, 39.99999999999990763, 37.56421063658199699 ) ) ;
#8788 = CARTESIAN_POINT ( 'NONE',  ( 91.82158438592158234, 16.11829626348434630, -40.45024623143955012 ) ) ;
#8789 = DIRECTION ( 'NONE',  ( 0.000000000000000000, 0.000000000000000000, 1.000000000000000000 ) ) ;
#8790 = CARTESIAN_POINT ( 'NONE',  ( -96.93773665438902754, -9.001171854902104030, -20.58457565566405734 ) ) ;
#8791 = CARTESIAN_POINT ( 'NONE',  ( 4.995406935893310418, -67.35176059880237176, 10.78321810387813429 ) ) ;
#8792 = ORIENTED_EDGE ( 'NONE', *, *, #3782, .T. ) ;
#8794 = CARTESIAN_POINT ( 'NONE',  ( -210.0000000000000284, 69.29737539576900929, -75.30386416458597409 ) ) ;
#8793 = CARTESIAN_POINT ( 'NONE',  ( -162.0762913951020892, -1.198031840385767266, -1.198031840385758384 ) ) ;
#8795 = DIRECTION ( 'NONE',  ( 0.000000000000000000, 1.000000000000000000, 0.000000000000000000 ) ) ;
#8796 = CARTESIAN_POINT ( 'NONE',  ( -135.8532207217289738, -30.84685318188647685, -2.449293598294708485E-15 ) ) ;
#8797 = CARTESIAN_POINT ( 'NONE',  ( -105.2054292635175727, 15.19799821370213522, 15.19799821370241943 ) ) ;
#8798 = CARTESIAN_POINT ( 'NONE',  ( -56.48582580120559271, -6.472252184284276844, 6.472252184284108978 ) ) ;
#8799 = VERTEX_POINT ( 'NONE', #23588 ) ;
#8800 = VERTEX_POINT ( 'NONE', #3628 ) ;
#8801 = CARTESIAN_POINT ( 'NONE',  ( 199.9999999999999147, 2.157212532375118563, 18.88823879575998177 ) ) ;
#8802 = CARTESIAN_POINT ( 'NONE',  ( -102.4309680866255690, 8.733065090073308667, -20.17061239837894959 ) ) ;
#8803 = VERTEX_POINT ( 'NONE', #5367 ) ;
#8804 = AXIS2_PLACEMENT_3D ( 'NONE', #19728, #6974, #13478 ) ;
#8805 = ORIENTED_EDGE ( 'NONE', *, *, #6809, .F. ) ;
#8806 = CARTESIAN_POINT ( 'NONE',  ( 0.2972598230769990524, -18.14793986248724522, 38.42060263243662632 ) ) ;
#8807 = CARTESIAN_POINT ( 'NONE',  ( 199.0191706476670959, -17.79509468669765226, -9.138050845474172235 ) ) ;
#8808 = CARTESIAN_POINT ( 'NONE',  ( 180.0000000000000000, -35.78896085774753288, 1.496915739050593134E-14 ) ) ;
#8809 = B_SPLINE_CURVE_WITH_KNOTS ( 'NONE', 3,
 ( #10281, #12008, #24120, #6028, #22265, #24657, #12140, #12529, #17981, #24527, #4178, #7870, #12272, #5891, #18390, #8146 ),
 .UNSPECIFIED., .F., .F.,
 ( 4, 2, 2, 2, 2, 2, 2, 4 ),
 ( -5.998499568544072563E-08, 0.003520343011582062996, 0.007040746008159811872, 0.01408155200131532003, 0.01760195499789307325, 0.02112235799447082993, 0.02464276099104858314, 0.02816316398762633982 ),
 .UNSPECIFIED. ) ;
#8810 = CARTESIAN_POINT ( 'NONE',  ( -91.56559293963834989, -16.03295912088716335, 40.53558337403673306 ) ) ;
#8811 = CARTESIAN_POINT ( 'NONE',  ( 163.1118516004056573, -19.27778845538761132, -19.27778845538770724 ) ) ;
#8812 = CARTESIAN_POINT ( 'NONE',  ( -100.7734535825088500, 39.99999999999994316, 17.32597176626825686 ) ) ;
#8813 = CARTESIAN_POINT ( 'NONE',  ( -199.9999999999997726, -24.82633483071077762, 44.86878812508861358 ) ) ;
#8814 = CARTESIAN_POINT ( 'NONE',  ( -199.9999999999999432, -4.865628651906739321, 55.16984130226897776 ) ) ;
#8815 = CARTESIAN_POINT ( 'NONE',  ( 19.06497207195981858, 5.735870351258996432E-13, -54.19242893257843008 ) ) ;
#8816 = CARTESIAN_POINT ( 'NONE',  ( 192.4448373802100889, -1.741373372144848397E-13, 20.00000000003942091 ) ) ;
#8817 = CARTESIAN_POINT ( 'NONE',  ( -77.80807733969351148, 19.71366427569386559, 9.671920888572945074 ) ) ;
#8818 = SPHERICAL_SURFACE ( 'NONE', #11944, 15.00000000000000000 ) ;
#8819 = CARTESIAN_POINT ( 'NONE',  ( 199.0067627483201989, 19.31843298438769807, -5.161535144790875940 ) ) ;
#8820 = CARTESIAN_POINT ( 'NONE',  ( -188.3610564113221812, 13.83140491817328410, 47.01267209787948076 ) ) ;
#8821 = CARTESIAN_POINT ( 'NONE',  ( -30.26275506840324070, -29.48230279907817675, 27.08623969584564151 ) ) ;
#8822 = EDGE_CURVE ( 'NONE', #1453, #13720, #9569, .T. ) ;
#8823 = DIRECTION ( 'NONE',  ( 0.000000000000000000, 0.000000000000000000, -1.000000000000000000 ) ) ;
#8824 = CARTESIAN_POINT ( 'NONE',  ( 184.8905102610680444, -13.49065550809810965, 13.49065550809799596 ) ) ;
#8825 = CARTESIAN_POINT ( 'NONE',  ( -87.05569247514564779, -17.94468678732216915, 11.73639047247333878 ) ) ;
#8826 = CARTESIAN_POINT ( 'NONE',  ( -259.2033419157646676, -21.55415060305824326, -21.55415060305857367 ) ) ;
#8827 = CARTESIAN_POINT ( 'NONE',  ( -200.0000000000000284, 45.65206365911554087, -19.98641303047023854 ) ) ;
#8828 = DIRECTION ( 'NONE',  ( -1.850371707708594760E-15, -0.3995982397413175291, -0.9166903767334096953 ) ) ;
#8829 = CARTESIAN_POINT ( 'NONE',  ( -238.4067589809705794, 57.25054294065799354, -0.6820004457334954973 ) ) ;
#8830 = EDGE_CURVE ( 'NONE', #4362, #24911, #23703, .T. ) ;
#8831 = CARTESIAN_POINT ( 'NONE',  ( 91.82158438592159655, -22.79471317813468900, 40.00000000000002132 ) ) ;
#8832 = CARTESIAN_POINT ( 'NONE',  ( -599.4467069854360943, 39.47241407940956037, 21.63078978636851346 ) ) ;
#8833 = ORIENTED_EDGE ( 'NONE', *, *, #5029, .F. ) ;
#8834 = CARTESIAN_POINT ( 'NONE',  ( -56.48582580120557850, -39.99999999999970868, -30.84685318188687120 ) ) ;
#8835 = EDGE_CURVE ( 'NONE', #19209, #13176, #19881, .T. ) ;
#8836 = CARTESIAN_POINT ( 'NONE',  ( 199.0061118454574114, 7.773422122678746327, -18.42227132588763183 ) ) ;
#8837 = EDGE_CURVE ( 'NONE', #6493, #11418, #11598, .T. ) ;
#8838 = CARTESIAN_POINT ( 'NONE',  ( 190.0000000000000000, -74.99999999999988631, 0.000000000000000000 ) ) ;
#8839 = ORIENTED_EDGE ( 'NONE', *, *, #16631, .T. ) ;
#8840 = ORIENTED_EDGE ( 'NONE', *, *, #25417, .T. ) ;
#8841 = ORIENTED_EDGE ( 'NONE', *, *, #18883, .F. ) ;
#8842 = CARTESIAN_POINT ( 'NONE',  ( 184.8905102610680444, 19.07866798485561333, 40.00000000000002132 ) ) ;
#8843 = DIRECTION ( 'NONE',  ( 0.000000000000000000, -1.000000000000000000, 0.000000000000000000 ) ) ;
#8844 = CARTESIAN_POINT ( 'NONE',  ( 83.06440094971527799, 23.65491511361215160, -10.91839312130610651 ) ) ;
#8845 = CARTESIAN_POINT ( 'NONE',  ( -77.55672185583993894, -16.64541244686190424, 14.65061613760696524 ) ) ;
#8846 = CARTESIAN_POINT ( 'NONE',  ( 4.995406935893290878, -5.232665749138292703E-14, 15.24977328854832592 ) ) ;
#8847 = CARTESIAN_POINT ( 'NONE',  ( 199.9999999999999716, 7.832101404672591194, -17.31171755797958056 ) ) ;
#8848 = CARTESIAN_POINT ( 'NONE',  ( 199.9999999999999147, -9.095991256943364078, -16.68624471194709358 ) ) ;
#8849 = CARTESIAN_POINT ( 'NONE',  ( 4.995406935893297984, 10.78321810390233892, -67.35176059882522281 ) ) ;
#8850 = CARTESIAN_POINT ( 'NONE',  ( -30.26275506840324070, -1.198031551616016266, -1.198031551616031587 ) ) ;
#8851 = CARTESIAN_POINT ( 'NONE',  ( -110.0368417077424965, -18.51665893310755351, -7.992411109430164196 ) ) ;
#8852 = CARTESIAN_POINT ( 'NONE',  ( 200.0000000000000000, 39.99999999999985079, 20.00000000000052225 ) ) ;
#8853 = CARTESIAN_POINT ( 'NONE',  ( 146.6084372240433709, -3.800685668859084210, 52.76785682606516303 ) ) ;
#8854 = CARTESIAN_POINT ( 'NONE',  ( -91.56559293963836410, 22.67402823373189946, -0.000000000000000000 ) ) ;
#8855 = CARTESIAN_POINT ( 'NONE',  ( -198.0356074513804572, -10.87444709760996986, 67.44298959253333692 ) ) ;
#8856 = CARTESIAN_POINT ( 'NONE',  ( 199.0061137528103359, 18.42594117564502909, -7.764722426784522291 ) ) ;
#8858 = CARTESIAN_POINT ( 'NONE',  ( 151.7948205124836534, 40.00000000000017053, -33.23291073765538783 ) ) ;
#8857 = CARTESIAN_POINT ( 'NONE',  ( 0.2972598230769990524, -18.14793986248671231, -38.42060263243687501 ) ) ;
#8859 = CARTESIAN_POINT ( 'NONE',  ( 170.2234770963711128, -24.55285855007183926, 0.000000000000000000 ) ) ;
#8860 = CARTESIAN_POINT ( 'NONE',  ( -56.48582580120559982, -34.75652343174615311, 21.81201906317766870 ) ) ;
#8861 = CARTESIAN_POINT ( 'NONE',  ( -280.0000000000000568, 19.99999999999995737, 40.00000000000002132 ) ) ;
#8862 = VERTEX_POINT ( 'NONE', #25722 ) ;
#8863 = CARTESIAN_POINT ( 'NONE',  ( 19.44355705749374152, -43.94967286772092052, 18.20455056366046165 ) ) ;
#8864 =( BOUNDED_CURVE ( )  B_SPLINE_CURVE ( 3, ( #16486, #6364, #18879, #20884, #6632, #14611, #22743 ),
 .UNSPECIFIED., .F., .F. ) 
 B_SPLINE_CURVE_WITH_KNOTS ( ( 4, 3, 4 ),
 ( 0.007486030685209765952, 0.02316748376737289700, 0.03884893684953920345 ),
 .UNSPECIFIED. ) 
 CURVE ( )  GEOMETRIC_REPRESENTATION_ITEM ( )  RATIONAL_B_SPLINE_CURVE ( ( 0.5852718452494414247, 0.6660804010233971617, 0.8043231192735833535, 1.000000000000000000, 0.8043231192735437185, 0.6660804010233410954, 0.5852718452493922419 ) ) 
 REPRESENTATION_ITEM ( '' )  );
#8865 = CARTESIAN_POINT ( 'NONE',  ( 57.59792236341147031, 37.56421063658187620, -40.00000000000002132 ) ) ;
#8866 = ORIENTED_EDGE ( 'NONE', *, *, #18736, .T. ) ;
#8867 = CARTESIAN_POINT ( 'NONE',  ( 190.0000000000000000, 71.50000000000009948, 66.50000000000005684 ) ) ;
#8868 = CARTESIAN_POINT ( 'NONE',  ( -77.92915424793434909, 20.15198149301296482, 8.347224043097730473 ) ) ;
#8869 = CARTESIAN_POINT ( 'NONE',  ( -77.90255099906872260, -8.644468104261276764, 20.04994828523928163 ) ) ;
#8870 = CARTESIAN_POINT ( 'NONE',  ( -82.25372479520392233, 19.83917633296052685, 3.752706786415938467 ) ) ;
#8871 = MANIFOLD_SOLID_BREP ( 'Mirror2', #16424 ) ;
#8872 = CARTESIAN_POINT ( 'NONE',  ( -6.754359963566859193, 17.56548336386092757, -42.40682816664624966 ) ) ;
#8873 = CARTESIAN_POINT ( 'NONE',  ( 199.0263771350486763, -14.37646237564524476, 13.91501816527019919 ) ) ;
#8874 = CARTESIAN_POINT ( 'NONE',  ( -198.0356074513804572, 10.87444709759730088, -10.87444709759707173 ) ) ;
#8875 = CARTESIAN_POINT ( 'NONE',  ( 180.0000000000000000, -66.50000000000001421, -66.50000000000005684 ) ) ;
#8876 = CARTESIAN_POINT ( 'NONE',  ( 116.7964245048382850, -27.98274000340147794, 0.000000000000000000 ) ) ;
#8877 = CARTESIAN_POINT ( 'NONE',  ( -188.9478905404513114, -17.94277290414816406, 43.31768569177503281 ) ) ;
#8878 = CARTESIAN_POINT ( 'NONE',  ( -192.9588430854689989, -10.23066800230742501, -10.23066800230756712 ) ) ;
#8879 = CARTESIAN_POINT ( 'NONE',  ( -162.0762913951020892, -1.198031840385783919, 1.198031840385741731 ) ) ;
#8880 = CARTESIAN_POINT ( 'NONE',  ( 146.6084372240433709, -24.48358557860284179, -32.08495691632087699 ) ) ;
#8881 = FACE_OUTER_BOUND ( 'NONE', #5840, .T. ) ;
#8883 = CARTESIAN_POINT ( 'NONE',  ( -280.0000000000000568, 42.42640687119265408, 14.14213562373147504 ) ) ;
#8882 = CARTESIAN_POINT ( 'NONE',  ( -105.3755690713226585, 43.67073346367988051, -12.89780903124366418 ) ) ;
#8884 = CARTESIAN_POINT ( 'NONE',  ( 146.6084372240433709, 32.08495691632030145, 24.48358557860365181 ) ) ;
#8885 = CARTESIAN_POINT ( 'NONE',  ( -56.48582580120559982, 9.153146818113574668, 40.00000000000002132 ) ) ;
#8886 = CARTESIAN_POINT ( 'NONE',  ( 170.2234770963711128, -24.55285855007184281, -40.00000000000002132 ) ) ;
#8887 = CARTESIAN_POINT ( 'NONE',  ( 130.8568914410475088, 4.207082182989741348, -52.36146031193420924 ) ) ;
#8888 = DIRECTION ( 'NONE',  ( -1.000000000000000000, -1.836970198721030181E-16, 0.000000000000000000 ) ) ;
#8889 = CARTESIAN_POINT ( 'NONE',  ( 130.8568914410475088, -32.49135343045495006, 24.07718906446878648 ) ) ;
#8890 = CARTESIAN_POINT ( 'NONE',  ( -187.7698581930513058, 46.80706826624110306, -13.79076165500642404 ) ) ;
#8891 = ORIENTED_EDGE ( 'NONE', *, *, #7255, .F. ) ;
#8892 = CARTESIAN_POINT ( 'NONE',  ( 14.38125909742181463, 10.73282306405862485, 67.30136555898259587 ) ) ;
#8893 = CARTESIAN_POINT ( 'NONE',  ( -188.2995950289365226, 23.44932284465886241, 43.00522595870971543 ) ) ;
#8894 = CARTESIAN_POINT ( 'NONE',  ( -259.2033419157646676, -21.55415060305854524, 21.55415060305827524 ) ) ;
#8895 = CARTESIAN_POINT ( 'NONE',  ( -1.624577210513715730, -43.75845733971997475, -18.12534649861195035 ) ) ;
#8896 = ORIENTED_EDGE ( 'NONE', *, *, #21527, .F. ) ;
#8897 = CARTESIAN_POINT ( 'NONE',  ( -210.0000000000000284, -66.50000000000001421, -66.50000000000005684 ) ) ;
#8898 = CARTESIAN_POINT ( 'NONE',  ( -114.6381211271834673, -11.20694786414384936, -18.98758604910076997 ) ) ;
#8899 = CARTESIAN_POINT ( 'NONE',  ( 199.9999999999996021, 9.500464834803043601, -16.45734938164063621 ) ) ;
#8900 = CARTESIAN_POINT ( 'NONE',  ( -188.2995950289364373, 13.82811170417284075, -46.99046209955416487 ) ) ;
#8901 = AXIS2_PLACEMENT_3D ( 'NONE', #18734, #24734, #517 ) ;
#8902 = CARTESIAN_POINT ( 'NONE',  ( 163.1118516004056573, 12.73709011382478273, 2.449293598294708485E-15 ) ) ;
#8903 = CARTESIAN_POINT ( 'NONE',  ( -100.7734535825088500, -44.31723036834885932, -12.25131212657538171 ) ) ;
#8904 = CARTESIAN_POINT ( 'NONE',  ( 199.0111318983613842, 19.03723981379789265, 6.131360352008743853 ) ) ;
#8905 = EDGE_CURVE ( 'NONE', #18174, #1858, #3633, .T. ) ;
#8906 = CARTESIAN_POINT ( 'NONE',  ( 184.8905102610680444, -13.49065550809840630, 43.07788698682565354 ) ) ;
#8907 = CARTESIAN_POINT ( 'NONE',  ( -91.56559293963834989, -7.976292724337646577E-14, 17.32597176626811120 ) ) ;
#8908 = CARTESIAN_POINT ( 'NONE',  ( 130.8568914410475088, 40.00000000000015632, -34.05028731879774284 ) ) ;
#8909 =( BOUNDED_SURFACE ( )  B_SPLINE_SURFACE ( 3, 2, ( 
 ( #15322, #10825, #4978 ),
 ( #19197, #21329, #25583 ),
 ( #13085, #21202, #25456 ),
 ( #17068, #19319, #9085 ),
 ( #11205, #8959, #3222 ),
 ( #17191, #25327, #7086 ),
 ( #18938, #3101, #25202 ),
 ( #11328, #5223, #2853 ),
 ( #1101, #19444, #13327 ),
 ( #20942, #23327, #8825 ),
 ( #5103, #21448, #1232 ),
 ( #10961, #15200, #4845 ),
 ( #9337, #7330, #16935 ),
 ( #15443, #23571, #9211 ),
 ( #17322, #25070, #6821 ),
 ( #14938, #23074, #12951 ) ),
 .UNSPECIFIED., .F., .F., .F. ) 
 B_SPLINE_SURFACE_WITH_KNOTS ( ( 4, 2, 2, 2, 2, 2, 2, 4 ),
 ( 3, 3 ),
 ( 0.04143342415446721327, 0.04844559399082600665, 0.05195167890900539986, 0.05545776382718480002, 0.06246993366354359339, 0.06422297612263329347, 0.06597601858172298661, 0.06948210349990238677 ),
 ( 0.000000000000000000, 1.000000000000000000 ),
 .UNSPECIFIED. ) 
 GEOMETRIC_REPRESENTATION_ITEM ( )  RATIONAL_B_SPLINE_SURFACE ( (
 ( 1.000000000000000000, 0.9541700779530469800, 1.000000000000000000),
 ( 1.000000000000000000, 0.9520168980296377370, 1.000000000000000000),
 ( 1.000000000000000000, 0.9503263051604914358, 1.000000000000000000),
 ( 1.000000000000000000, 0.9485964699095221775, 1.000000000000000000),
 ( 1.000000000000000000, 0.9481599523402173268, 1.000000000000000000),
 ( 1.000000000000000000, 0.9475783919165745584, 1.000000000000000000),
 ( 1.000000000000000000, 0.9474332805886676034, 1.000000000000000000),
 ( 1.000000000000000000, 0.9474385816640782387, 1.000000000000000000),
 ( 1.000000000000000000, 0.9480200071112050431, 1.000000000000000000),
 ( 1.000000000000000000, 0.9494436219493812557, 1.000000000000000000),
 ( 1.000000000000000000, 0.9497633688928907025, 1.000000000000000000),
 ( 1.000000000000000000, 0.9504729676352060563, 1.000000000000000000),
 ( 1.000000000000000000, 0.9508638236298538882, 1.000000000000000000),
 ( 1.000000000000000000, 0.9521268919816204823, 1.000000000000000000),
 ( 1.000000000000000000, 0.9530924015900935631, 1.000000000000000000),
 ( 1.000000000000000000, 0.9541700779530452037, 1.000000000000000000) ) ) 
 REPRESENTATION_ITEM ( '' )  SURFACE ( )  );
#8910 = CARTESIAN_POINT ( 'NONE',  ( -200.0000000000000000, 52.49999999999988631, -82.49999999999998579 ) ) ;
#8911 = CARTESIAN_POINT ( 'NONE',  ( 19.06497207195980792, -14.19242893257839988, -40.00000000000002132 ) ) ;
#8913 = CARTESIAN_POINT ( 'NONE',  ( -611.0434898207377046, 30.88177058762790850, 25.43160472393209659 ) ) ;
#8912 = CARTESIAN_POINT ( 'NONE',  ( 19.94008347559497452, -13.96811062196804443, -47.92933869853823836 ) ) ;
#8914 = CARTESIAN_POINT ( 'NONE',  ( 14.38125909742182884, -55.17850393974264733, -40.00000000000002132 ) ) ;
#8915 = CARTESIAN_POINT ( 'NONE',  ( -162.0762913951020892, -1.198031840385783919, 1.198031840385741731 ) ) ;
#8916 = CARTESIAN_POINT ( 'NONE',  ( -126.6834154282191776, 9.107266658309034923, 24.89646316986419450 ) ) ;
#8917 = CARTESIAN_POINT ( 'NONE',  ( -163.5815439468645991, -18.59457101073928342, 35.61501074489160601 ) ) ;
#8918 = CARTESIAN_POINT ( 'NONE',  ( 151.7948205124836250, 1.012150473917908975E-13, -6.767089262349031742 ) ) ;
#8919 = CARTESIAN_POINT ( 'NONE',  ( -56.48582580120559271, -6.472252184284187138, -6.472252184284199572 ) ) ;
#8920 = CARTESIAN_POINT ( 'NONE',  ( 128.5815561518678294, -28.96468886173051516, -11.99756695644574123 ) ) ;
#8921 = CARTESIAN_POINT ( 'NONE',  ( 170.2234770963711128, 10.92277846919147066, 45.64576402573197811 ) ) ;
#8922 = CARTESIAN_POINT ( 'NONE',  ( -135.8532207217289738, 6.472252184283881604, 50.09629031063969506 ) ) ;
#8923 = EDGE_CURVE ( 'NONE', #6176, #23081, #17366, .T. ) ;
#8924 = ORIENTED_EDGE ( 'NONE', *, *, #23767, .T. ) ;
#8926 = CARTESIAN_POINT ( 'NONE',  ( -6.342283169554340461, 42.32555349774960263, -23.00001740814328954 ) ) ;
#8925 = CARTESIAN_POINT ( 'NONE',  ( -198.0356074513804572, -10.87444709759714634, -10.87444709759729911 ) ) ;
#8927 = CARTESIAN_POINT ( 'NONE',  ( 128.5824617753800680, 28.96492468983282009, -11.99766463964400565 ) ) ;
#8928 = CARTESIAN_POINT ( 'NONE',  ( -238.4067589809705794, -40.96449428006345528, 40.00000000000002132 ) ) ;
#8929 = CIRCLE ( 'NONE', #11870, 69.99999999999998579 ) ;
#8930 = EDGE_CURVE ( 'NONE', #13176, #21839, #18939, .T. ) ;
#8931 = DIRECTION ( 'NONE',  ( 0.000000000000000000, 1.000000000000000000, 0.000000000000000000 ) ) ;
#8932 = CARTESIAN_POINT ( 'NONE',  ( -195.5009199109406666, 44.52807166370264014, -18.44413118942395613 ) ) ;
#8933 =( LENGTH_UNIT ( ) NAMED_UNIT ( * ) SI_UNIT ( .MILLI., .METRE. ) );
#8934 = ORIENTED_EDGE ( 'NONE', *, *, #10106, .T. ) ;
#8935 = VERTEX_POINT ( 'NONE', #20657 ) ;
#8936 = CARTESIAN_POINT ( 'NONE',  ( -100.0753760173605542, 8.894334231739680519, -20.41987330121789768 ) ) ;
#8937 = B_SPLINE_CURVE_WITH_KNOTS ( 'NONE', 3,
 ( #19448, #13459, #7461, #1367, #1887, #5607, #24372, #9992, #26251, #21973 ),
 .UNSPECIFIED., .F., .F.,
 ( 4, 2, 2, 2, 4 ),
 ( 0.7921542097164080420, 0.8508620842112317728, 0.8814014469398914198, 0.9119408096685510667, 0.9406682828395580565 ),
 .UNSPECIFIED. ) ;
#8938 = DIRECTION ( 'NONE',  ( 1.000000000000000000, -0.000000000000000000, -0.000000000000000000 ) ) ;
#8939 = DIRECTION ( 'NONE',  ( 0.000000000000000000, 0.3028247695821862928, -0.9530462522498558409 ) ) ;
#8940 = ORIENTED_EDGE ( 'NONE', *, *, #19486, .T. ) ;
#8941 = CARTESIAN_POINT ( 'NONE',  ( 192.4448373802100889, -14.14213562375876698, -14.14213562375885047 ) ) ;
#8942 = CARTESIAN_POINT ( 'NONE',  ( 199.0170773700648397, -15.56690153483635264, -12.55869779031424116 ) ) ;
#8943 = CARTESIAN_POINT ( 'NONE',  ( -105.2833435977151737, -4.389626034945506738, 20.98775841734936165 ) ) ;
#8944 = CARTESIAN_POINT ( 'NONE',  ( -280.0000000000000568, -42.42640687119295251, 14.14213562373088351 ) ) ;
#8945 = CARTESIAN_POINT ( 'NONE',  ( -105.2990478492033191, 20.88641510963992332, 4.839947517601303595 ) ) ;
#8946 = CARTESIAN_POINT ( 'NONE',  ( 136.1360204305621551, 40.00000000000002842, 4.966164525587208445 ) ) ;
#8947 = DIRECTION ( 'NONE',  ( 1.000000000000000000, 5.508077988093228416E-14, 0.000000000000000000 ) ) ;
#8948 = CARTESIAN_POINT ( 'NONE',  ( -86.86493150571119770, -7.943527260495915066, -19.77569912839184596 ) ) ;
#8949 = AXIS2_PLACEMENT_3D ( 'NONE', #4950, #16645, #6661 ) ;
#8950 = CARTESIAN_POINT ( 'NONE',  ( 146.6084372240433709, -40.00000000000036238, 34.62501878078263218 ) ) ;
#8951 = CARTESIAN_POINT ( 'NONE',  ( -135.8532207217289738, -39.99999999999972289, -30.84685318188688541 ) ) ;
#8952 = CARTESIAN_POINT ( 'NONE',  ( -87.13361725336062591, 15.69997917300612933, 14.69601725244436885 ) ) ;
#8953 = DIRECTION ( 'NONE',  ( 0.000000000000000000, 0.000000000000000000, 1.000000000000000000 ) ) ;
#8954 = CARTESIAN_POINT ( 'NONE',  ( 199.0053905349878107, 15.66748078252780374, -12.42684713134076979 ) ) ;
#8955 = CARTESIAN_POINT ( 'NONE',  ( -197.6434631108650706, 18.53520396667539671, 44.74794079763712773 ) ) ;
#8956 = CARTESIAN_POINT ( 'NONE',  ( -91.56559293963836410, -12.25131212657524138, 44.31723036834888774 ) ) ;
#8957 = CARTESIAN_POINT ( 'NONE',  ( 150.0000000000000284, -125.7889608577475400, -82.49999999999998579 ) ) ;
#8958 = CARTESIAN_POINT ( 'NONE',  ( 192.4448373802101173, 14.14213562375862665, 42.42640687116509213 ) ) ;
#8959 = CARTESIAN_POINT ( 'NONE',  ( -82.24432634622075966, -12.38461122506346435, 15.96101146153378103 ) ) ;
#8960 = CARTESIAN_POINT ( 'NONE',  ( 14.38125909742181996, -10.73282306405815234, -67.30136555898266693 ) ) ;
#8961 = CARTESIAN_POINT ( 'NONE',  ( -636.4062240200004226, 29.79465556942914972, 33.72744621685050959 ) ) ;
#8962 = LINE ( 'NONE', #19201, #20220 ) ;
#8963 = ORIENTED_EDGE ( 'NONE', *, *, #8336, .T. ) ;
#8964 = CARTESIAN_POINT ( 'NONE',  ( -30.26275506840324070, 1.198031551616030033, -1.198031551616006496 ) ) ;
#8965 = CARTESIAN_POINT ( 'NONE',  ( -208.1127848780265026, -15.00245453012673202, 0.000000000000000000 ) ) ;
#8966 = CARTESIAN_POINT ( 'NONE',  ( -619.3049992912841617, 29.30303271858384306, -34.15210011782420452 ) ) ;
#8967 = VERTEX_POINT ( 'NONE', #24525 ) ;
#8968 = CARTESIAN_POINT ( 'NONE',  ( -100.7734535825088500, -39.99999999999986500, -17.32597176626853397 ) ) ;
#8969 = CARTESIAN_POINT ( 'NONE',  ( 199.0094080386897986, -2.402341955940460405, -19.89500313782861696 ) ) ;
#8970 = LINE ( 'NONE', #24954, #10285 ) ;
#8971 = ORIENTED_EDGE ( 'NONE', *, *, #5570, .T. ) ;
#8972 = ORIENTED_EDGE ( 'NONE', *, *, #5245, .F. ) ;
#8973 = ORIENTED_EDGE ( 'NONE', *, *, #22005, .F. ) ;
#8974 = CARTESIAN_POINT ( 'NONE',  ( -192.9588430854690273, 54.46834944101718889, 40.00000000000002132 ) ) ;
#8975 = MANIFOLD_SOLID_BREP ( 'Revolve3', #18975 ) ;
#8976 = CARTESIAN_POINT ( 'NONE',  ( -103.9650464694441041, -20.03380587597265716, -8.298274098614912830 ) ) ;
#8977 = EDGE_CURVE ( 'NONE', #13725, #8230, #1953, .T. ) ;
#8978 = B_SPLINE_CURVE_WITH_KNOTS ( 'NONE', 3,
 ( #1439, #15651, #19653, #21405, #11529, #21530, #23405, #13787 ),
 .UNSPECIFIED., .F., .F.,
 ( 4, 2, 2, 4 ),
 ( 0.008471746897480886968, 0.01057975003218126868, 0.01268775316688165039, 0.01690375943628241728 ),
 .UNSPECIFIED. ) ;
#8979 = CARTESIAN_POINT ( 'NONE',  ( 57.59792236341147031, 1.908507979671054758E-14, -2.435789363418160658 ) ) ;
#8980 = CARTESIAN_POINT ( 'NONE',  ( 200.0000000000000853, 3.093441846007485285, -18.74813587279223981 ) ) ;
#8981 = ADVANCED_FACE ( 'NONE', ( #16658 ), #13189, .T. ) ;
#8982 = CARTESIAN_POINT ( 'NONE',  ( 199.9999999999999147, 7.976971673177774669, -17.24969891087616602 ) ) ;
#8983 = AXIS2_PLACEMENT_3D ( 'NONE', #2178, #18124, #16129 ) ;
#8984 = CARTESIAN_POINT ( 'NONE',  ( -135.8532207217289738, -6.472252184283586729, -50.09629031063973770 ) ) ;
#8985 = B_SPLINE_CURVE_WITH_KNOTS ( 'NONE', 3,
 ( #11867, #4176, #12398, #166, #1771, #8271 ),
 .UNSPECIFIED., .F., .F.,
 ( 4, 2, 4 ),
 ( 0.0003134705440570314063, 0.004478952798826419529, 0.008644435053595807272 ),
 .UNSPECIFIED. ) ;
#8986 = CARTESIAN_POINT ( 'NONE',  ( 136.1360204305621266, 24.77266263493104148, 24.77266263493145004 ) ) ;
#8987 = AXIS2_PLACEMENT_3D ( 'NONE', #17684, #25572, #19952 ) ;
#8988 = CARTESIAN_POINT ( 'NONE',  ( -110.0574659383507878, -18.01685545903095331, -9.172431002379518361 ) ) ;
#8989 = CARTESIAN_POINT ( 'NONE',  ( -56.48582580120558561, 3.151766524733697544E-13, -30.84685318188644132 ) ) ;
#8990 = LINE ( 'NONE', #25101, #19768 ) ;
#8991 = CARTESIAN_POINT ( 'NONE',  ( 0.4289713102705710046, 14.02712011273575676, 48.32239598606143005 ) ) ;
#8992 = CARTESIAN_POINT ( 'NONE',  ( 57.59792236341148453, -54.84617931850877426, -1.722363176415331099 ) ) ;
#8993 = CARTESIAN_POINT ( 'NONE',  ( 199.0118837125828861, 18.49943804575643824, 7.595438918186243171 ) ) ;
#8995 = CARTESIAN_POINT ( 'NONE',  ( 136.1360204305621551, 40.00000000000017053, -35.03383547441281820 ) ) ;
#8994 = CARTESIAN_POINT ( 'NONE',  ( 91.82158438592158234, -12.16597498397778843, 12.16597498397750954 ) ) ;
#8996 = CARTESIAN_POINT ( 'NONE',  ( 146.6084372240433709, -34.62501878078303008, -40.00000000000002132 ) ) ;
#8997 = CARTESIAN_POINT ( 'NONE',  ( -86.96347745069644475, -15.38646221621796073, 41.18208027870593924 ) ) ;
#8998 = CARTESIAN_POINT ( 'NONE',  ( -30.26275506840324425, 41.69427246844627177, 40.00000000000002132 ) ) ;
#8999 = ORIENTED_EDGE ( 'NONE', *, *, #13074, .T. ) ;
#9000 = CARTESIAN_POINT ( 'NONE',  ( 1.925538622543135903, -48.64880301058170886, 14.07631154917441663 ) ) ;
#9001 = CIRCLE ( 'NONE', #13249, 69.99999999999998579 ) ;
#9002 = CARTESIAN_POINT ( 'NONE',  ( -100.7734535825088500, -22.67402823373193499, -40.00000000000002132 ) ) ;
#9003 = DIRECTION ( 'NONE',  ( 0.000000000000000000, -1.000000000000000000, 0.000000000000000000 ) ) ;
#9004 = CARTESIAN_POINT ( 'NONE',  ( -162.0762913951020892, 29.48230308784758691, 29.48230308784772191 ) ) ;
#9005 = CARTESIAN_POINT ( 'NONE',  ( 130.8568914410475088, -39.99999999999988631, -34.05028731879802706 ) ) ;
#9006 = CARTESIAN_POINT ( 'NONE',  ( -82.30220482034330587, 18.74474319042426984, -7.441767004318775136 ) ) ;
#9007 = CARTESIAN_POINT ( 'NONE',  ( -47.30403195813222084, 12.59259458032456713, -30.40121262098807620 ) ) ;
#9008 = CARTESIAN_POINT ( 'NONE',  ( 199.0212029771548430, -19.33411866963394488, -5.169619751639646488 ) ) ;
#9009 = EDGE_CURVE ( 'NONE', #5318, #21077, #13405, .T. ) ;
#9010 = CARTESIAN_POINT ( 'NONE',  ( -213.1075012329537230, 66.26714140138673770, -9.698598906462034819 ) ) ;
#9011 = EDGE_CURVE ( 'NONE', #16736, #2387, #6609, .T. ) ;
#9012 = DIRECTION ( 'NONE',  ( 1.000000000000000000, -0.000000000000000000, 1.224646799147353207E-16 ) ) ;
#9013 = DIRECTION ( 'NONE',  ( 0.000000000000000000, 0.3995982397855803447, 0.9166903767141147963 ) ) ;
#9014 = CARTESIAN_POINT ( 'NONE',  ( 23.37394308801977871, -23.33966569535037294, -42.85717664514612579 ) ) ;
#9015 = CARTESIAN_POINT ( 'NONE',  ( -135.8532207217289738, 34.75652343174625258, -21.81201906317744132 ) ) ;
#9016 = CARTESIAN_POINT ( 'NONE',  ( -238.4067589809705794, 27.60227080167040370, 28.96627169325338613 ) ) ;
#9017 = DIRECTION ( 'NONE',  ( -1.836970198721030427E-16, 1.000000000000000000, -1.682156097916904327E-16 ) ) ;
#9018 = CARTESIAN_POINT ( 'NONE',  ( -56.48582580120559271, 6.472252184284121412, 6.472252184284244869 ) ) ;
#9019 = CIRCLE ( 'NONE', #23051, 5.000000000000004441 ) ;
#9021 = CARTESIAN_POINT ( 'NONE',  ( 14.38125909742180397, 67.30136555898270956, -10.73282306405792319 ) ) ;
#9020 = CARTESIAN_POINT ( 'NONE',  ( -208.1127848780265026, -10.60833733269537227, -10.60833733269551793 ) ) ;
#9022 = CARTESIAN_POINT ( 'NONE',  ( -100.7734535825088500, -16.03295912088659492, -40.53558337403696044 ) ) ;
#9023 = CARTESIAN_POINT ( 'NONE',  ( 146.6084372240433709, 5.374981219217002781, -40.00000000000002132 ) ) ;
#9024 = CARTESIAN_POINT ( 'NONE',  ( 130.8568914410475088, 32.49135343045483637, -24.07718906446901030 ) ) ;
#9025 = DIRECTION ( 'NONE',  ( 1.000000000000000000, -0.000000000000000000, -0.000000000000000000 ) ) ;
#9026 = CARTESIAN_POINT ( 'NONE',  ( -280.0000000000000568, -42.42640687119305198, 14.14213562373058686 ) ) ;
#9027 = CARTESIAN_POINT ( 'NONE',  ( -144.0562564039820188, 31.27039870050057146, -10.50946916206093817 ) ) ;
#9028 = VERTEX_POINT ( 'NONE', #3145 ) ;
#9029 = CARTESIAN_POINT ( 'NONE',  ( -162.0762913951020892, 29.48230308784758691, 29.48230308784772191 ) ) ;
#9030 = DIRECTION ( 'NONE',  ( 0.000000000000000000, -0.3028247695821851271, 0.9530462522498561739 ) ) ;
#9031 = CARTESIAN_POINT ( 'NONE',  ( -91.56559293963836410, 44.31723036834890905, 12.25131212657507795 ) ) ;
#9032 = CARTESIAN_POINT ( 'NONE',  ( 200.0000000000000000, 60.27431767988573341, -73.32453023895050137 ) ) ;
#9033 = EDGE_LOOP ( 'NONE', ( #1630, #21463, #8140, #18034 ) ) ;
#9034 = CARTESIAN_POINT ( 'NONE',  ( -188.2652133075167455, -46.97855991888840066, 13.82568790539422388 ) ) ;
#9035 = CARTESIAN_POINT ( 'NONE',  ( 199.9999999999999147, -10.82539530975288855, -15.62049148088690131 ) ) ;
#9036 = CARTESIAN_POINT ( 'NONE',  ( 23.41418334855306327, -23.33148157649288379, 42.84479974151765447 ) ) ;
#9037 = CARTESIAN_POINT ( 'NONE',  ( 136.1360204305621551, -35.03383547441293899, -40.00000000000002132 ) ) ;
#9038 = CARTESIAN_POINT ( 'NONE',  ( 60.07376046270519510, 13.17995839193378060, -31.81923430133271324 ) ) ;
#9039 = CARTESIAN_POINT ( 'NONE',  ( 199.0122446118616892, 18.20979473430505280, 8.267810710173087330 ) ) ;
#9040 = CARTESIAN_POINT ( 'NONE',  ( -135.8532207217289738, -21.81201906317806305, 34.75652343174590442 ) ) ;
#9041 = CARTESIAN_POINT ( 'NONE',  ( 170.2234770963711128, -2.511315425431857630E-14, 15.44714144992816074 ) ) ;
#9042 = CARTESIAN_POINT ( 'NONE',  ( -213.1075012329537230, -8.703598725189323045E-14, 13.71589010951911902 ) ) ;
#9043 = FACE_OUTER_BOUND ( 'NONE', #3329, .T. ) ;
#9044 = CARTESIAN_POINT ( 'NONE',  ( 130.8568914410475088, 34.05028731879790627, -40.00000000000002132 ) ) ;
#9046 = CARTESIAN_POINT ( 'NONE',  ( 4.995406935893293543, -10.78321810389005364, 10.78321810388994173 ) ) ;
#9045 = CARTESIAN_POINT ( 'NONE',  ( 23.35901252181217913, -23.34306388117422060, -42.86175755505345109 ) ) ;
#9047 = CARTESIAN_POINT ( 'NONE',  ( -100.7734535825088500, 22.67402823373189591, -0.000000000000000000 ) ) ;
#9048 = CARTESIAN_POINT ( 'NONE',  ( -135.8532207217289738, 34.75652343174594705, 21.81201906317792449 ) ) ;
#9049 = CARTESIAN_POINT ( 'NONE',  ( -86.96347745069645896, 40.00000000000019895, -18.24025645688310249 ) ) ;
#9050 = CARTESIAN_POINT ( 'NONE',  ( -114.7465989397677220, 17.47221266595968459, -13.54917888338830068 ) ) ;
#9051 = CARTESIAN_POINT ( 'NONE',  ( -162.0762913951020892, -39.99999999999961631, -41.69427287692722928 ) ) ;
#9052 = CARTESIAN_POINT ( 'NONE',  ( 199.0259577874143417, -9.576177499050416486, 17.56472219104047028 ) ) ;
#9053 = CARTESIAN_POINT ( 'NONE',  ( 149.5792919132162524, -29.41975665910036142, -12.18606220991559219 ) ) ;
#9054 = CARTESIAN_POINT ( 'NONE',  ( 192.4448373802101173, 14.14213562370261279, 42.42640687122091236 ) ) ;
#9055 = CARTESIAN_POINT ( 'NONE',  ( 91.82158438592156813, 40.45024623143950038, 16.11829626348447420 ) ) ;
#9056 = EDGE_LOOP ( 'NONE', ( #25818, #10832, #14814, #16874 ) ) ;
#9058 = CARTESIAN_POINT ( 'NONE',  ( -3.993758944536190736, 47.00698038897044739, -13.83056263162072952 ) ) ;
#9057 = CARTESIAN_POINT ( 'NONE',  ( 4.995406935893293543, -10.78321810388990265, -10.78321810389009272 ) ) ;
#9059 = DIRECTION ( 'NONE',  ( 1.000000000000000000, -1.937599346585394162E-16, -0.000000000000000000 ) ) ;
#9060 = CARTESIAN_POINT ( 'NONE',  ( 14.38125909742181285, -15.17850393972633505, 40.00000000000002132 ) ) ;
#9061 = CARTESIAN_POINT ( 'NONE',  ( -114.4364955367314707, 8.064892380844273845, -20.29001642038674902 ) ) ;
#9062 = ORIENTED_EDGE ( 'NONE', *, *, #4973, .T. ) ;
#9063 = ORIENTED_EDGE ( 'NONE', *, *, #15877, .T. ) ;
#9064 = LINE ( 'NONE', #17671, #5774 ) ;
#9065 = CARTESIAN_POINT ( 'NONE',  ( -295.0000000000000568, -4.611870868841669993E-14, -19.53474504356812602 ) ) ;
#9066 = CARTESIAN_POINT ( 'NONE',  ( 116.7964245048362102, 1.191563696448279148E-13, -27.98274000340060041 ) ) ;
#9067 = EDGE_LOOP ( 'NONE', ( #17634, #5704 ) ) ;
#9068 = CARTESIAN_POINT ( 'NONE',  ( 199.0235864634049108, -19.99353228191618825, 0.6599136639449380004 ) ) ;
#9069 = CARTESIAN_POINT ( 'NONE',  ( -105.2276882639782656, -2.726203881901831050, 21.34721338855225881 ) ) ;
#9070 = CARTESIAN_POINT ( 'NONE',  ( -213.1075012329537230, 9.698598906462684965, 66.26714140138669507 ) ) ;
#9071 = CARTESIAN_POINT ( 'NONE',  ( -259.2033419157646676, -6.730120644403570829, -6.730120644403545960 ) ) ;
#9072 = CARTESIAN_POINT ( 'NONE',  ( -192.9588430854690273, 39.99999999999992895, 14.46834944099983922 ) ) ;
#9073 = CARTESIAN_POINT ( 'NONE',  ( -626.9846540392142060, 90.00000000000000000, -65.00000000000004263 ) ) ;
#9074 = DIRECTION ( 'NONE',  ( 0.000000000000000000, 1.000000000000000000, 0.000000000000000000 ) ) ;
#9075 = EDGE_CURVE ( 'NONE', #7180, #11718, #18987, .T. ) ;
#9076 = CARTESIAN_POINT ( 'NONE',  ( -280.0000000000000568, -40.00000000000028422, 19.99999999999959499 ) ) ;
#9077 = CARTESIAN_POINT ( 'NONE',  ( -30.26275506840324425, 40.00000000000044764, -41.69427246844585255 ) ) ;
#9078 = LINE ( 'NONE', #11197, #25365 ) ;
#9079 = DIRECTION ( 'NONE',  ( 0.000000000000000000, 1.000000000000000000, 0.000000000000000000 ) ) ;
#9080 = CARTESIAN_POINT ( 'NONE',  ( -200.0000000000000000, 20.90527768611954684, -45.34857661735428280 ) ) ;
#9081 = CARTESIAN_POINT ( 'NONE',  ( -195.5009199109816791, 18.44413118942227570, 44.52807166372294745 ) ) ;
#9082 = CARTESIAN_POINT ( 'NONE',  ( -96.93773665438804699, 8.190703376740504638, 20.92028269119447970 ) ) ;
#9083 = CARTESIAN_POINT ( 'NONE',  ( -100.0753760173626290, 8.894334231739064123, 20.41987330121790833 ) ) ;
#9084 = CARTESIAN_POINT ( 'NONE',  ( 146.6084372240433993, 24.48358557860341733, -24.48358557860313311 ) ) ;
#9085 = CARTESIAN_POINT ( 'NONE',  ( -87.08883489502147768, -12.58611167335523007, 17.39766501533223320 ) ) ;
#9086 = CARTESIAN_POINT ( 'NONE',  ( 57.59792236341148453, -26.56190807104663421, -26.56190807104710672 ) ) ;
#9087 = CARTESIAN_POINT ( 'NONE',  ( -166.7090905286406723, -15.35183918171654227, -37.06261835958360962 ) ) ;
#9088 = CARTESIAN_POINT ( 'NONE',  ( -90.07798792367799479, 15.74993999324163951, 15.74993999324193084 ) ) ;
#9089 = ORIENTED_EDGE ( 'NONE', *, *, #3211, .F. ) ;
#9090 = CARTESIAN_POINT ( 'NONE',  ( 146.6084372240433993, -24.48358557860353457, 24.48358557860296258 ) ) ;
#9091 = LINE ( 'NONE', #19579, #11139 ) ;
#9092 = CARTESIAN_POINT ( 'NONE',  ( -622.1724833024856025, 28.60431887920636740, -34.74667818490387816 ) ) ;
#9093 = EDGE_LOOP ( 'NONE', ( #12262, #7720, #4021, #18474 ) ) ;
#9094 = CARTESIAN_POINT ( 'NONE',  ( 192.4448373802100889, 2.472897170449861688E-13, -19.99999999996060751 ) ) ;
#9095 = CARTESIAN_POINT ( 'NONE',  ( 199.0231574205945435, -19.99787883075954653, -0.5143984472968653465 ) ) ;
#9096 = CARTESIAN_POINT ( 'NONE',  ( -199.9999999999999432, 5.435833037453086994E-13, -55.16984130226961724 ) ) ;
#9097 = ORIENTED_EDGE ( 'NONE', *, *, #6370, .F. ) ;
#9098 = ORIENTED_EDGE ( 'NONE', *, *, #20796, .F. ) ;
#9099 = CARTESIAN_POINT ( 'NONE',  ( 130.8568914410475372, 5.949712681206715814, 2.449293598294708485E-15 ) ) ;
#9100 = FACE_OUTER_BOUND ( 'NONE', #21297, .T. ) ;
#9101 = CARTESIAN_POINT ( 'NONE',  ( -77.55625318716886341, -15.17516088037291766, 16.12447834766487276 ) ) ;
#9102 = CARTESIAN_POINT ( 'NONE',  ( -30.26275506840324070, -40.00000000000003553, 1.694272468446120117 ) ) ;
#9103 = CARTESIAN_POINT ( 'NONE',  ( 199.9999999999996305, -13.87326568555608830, -12.99368172854615366 ) ) ;
#9104 = DIRECTION ( 'NONE',  ( -0.2259624731719848123, 0.000000000000000000, -0.9741360072998019870 ) ) ;
#9105 = CARTESIAN_POINT ( 'NONE',  ( -62.72988123312369169, -10.50767649786947366, -25.36777511015252884 ) ) ;
#9106 = CARTESIAN_POINT ( 'NONE',  ( 136.1360204305621266, 53.05693388239320285, -3.511608612530223716 ) ) ;
#9107 = CARTESIAN_POINT ( 'NONE',  ( -77.58504660580179291, -17.50307030595003965, -13.57339709064347488 ) ) ;
#9108 = CARTESIAN_POINT ( 'NONE',  ( -192.9588430854690273, -39.99999999999948841, -54.46834944098263520 ) ) ;
#9109 = CARTESIAN_POINT ( 'NONE',  ( -208.1127848780265026, -10.60833733269537227, -10.60833733269551793 ) ) ;
#9110 = CARTESIAN_POINT ( 'NONE',  ( -162.0762913951021176, -1.694272876828353702, -40.00000000000002132 ) ) ;
#9111 = CARTESIAN_POINT ( 'NONE',  ( -56.48582580120558561, -21.81201906317785699, 21.81201906317761896 ) ) ;
#9112 = CARTESIAN_POINT ( 'NONE',  ( 192.4448373802100889, 20.00000000003945644, 0.000000000000000000 ) ) ;
#9114 = CARTESIAN_POINT ( 'NONE',  ( 146.6084372240433709, 40.00000000000017053, -34.62501878078291639 ) ) ;
#9113 = CARTESIAN_POINT ( 'NONE',  ( -198.0356074513804572, -17.40982414986427429, -39.15871834505933435 ) ) ;
#9115 = CARTESIAN_POINT ( 'NONE',  ( -362.0709805440841365, -4.857225732735059864E-14, 0.000000000000000000 ) ) ;
#9116 = CARTESIAN_POINT ( 'NONE',  ( 14.38125909742180752, 10.73282306404720465, 10.73282306404724018 ) ) ;
#9117 = CARTESIAN_POINT ( 'NONE',  ( 19.06497207195980792, 54.19242893257844429, -40.00000000000002132 ) ) ;
#9118 = ORIENTED_EDGE ( 'NONE', *, *, #7796, .F. ) ;
#9119 = CARTESIAN_POINT ( 'NONE',  ( 20.69615274314397624, -47.71500688527799383, 13.93598092273205680 ) ) ;
#9120 = CARTESIAN_POINT ( 'NONE',  ( -105.3755690713226585, 18.24025645688350750, -40.00000000000002132 ) ) ;
#9121 = DIRECTION ( 'NONE',  ( 0.000000000000000000, 0.3028247695821854046, -0.9530462522498561739 ) ) ;
#9122 = CARTESIAN_POINT ( 'NONE',  ( 130.8568914410475088, -24.07718906446910623, 32.49135343045471558 ) ) ;
#9123 = CARTESIAN_POINT ( 'NONE',  ( -280.0000000000000000, 1.839446121267387017E-14, -20.00000000000001421 ) ) ;
#9124 = CARTESIAN_POINT ( 'NONE',  ( -82.24626550008051140, 20.00141108520265121, 2.782958274668472232 ) ) ;
#9125 = CARTESIAN_POINT ( 'NONE',  ( -3.763361371728485061, -13.84281709279630945, -47.08953757622914083 ) ) ;
#9126 = CARTESIAN_POINT ( 'NONE',  ( 199.9999999999998579, 2.934899133129863280, 18.78102297366244500 ) ) ;
#9127 = CARTESIAN_POINT ( 'NONE',  ( -192.9588430854690273, 66.79921049724377724, -10.23066800231904239 ) ) ;
#9128 = CARTESIAN_POINT ( 'NONE',  ( -87.01506749150250641, -5.383071875687824637, -20.72654704132506609 ) ) ;
#9129 = CARTESIAN_POINT ( 'NONE',  ( -192.9588430854689989, 10.23066800230756712, -10.23066800230735396 ) ) ;
#9130 = CARTESIAN_POINT ( 'NONE',  ( 130.8568914410475372, 24.07718906447210472, 24.07718906447249907 ) ) ;
#9131 = SHAPE_REPRESENTATION ( 'Bolt', ( #21058 ), #4479 ) ;
#9132 = CARTESIAN_POINT ( 'NONE',  ( -105.3755690713226585, 43.67073346367970288, 12.89780903124427702 ) ) ;
#9133 = CARTESIAN_POINT ( 'NONE',  ( -87.08883489501339170, 12.58611167335517855, -17.39766501532976761 ) ) ;
#9134 = CARTESIAN_POINT ( 'NONE',  ( -626.9846540392142060, 90.00000000000000000, -34.99999999999999289 ) ) ;
#9136 = CARTESIAN_POINT ( 'NONE',  ( -105.3755690713226585, -15.38646221621738164, -41.18208027870615240 ) ) ;
#9135 = CARTESIAN_POINT ( 'NONE',  ( -56.48582580120559271, 6.472252184284121412, 6.472252184284244869 ) ) ;
#9137 = CARTESIAN_POINT ( 'NONE',  ( -238.4067589809705794, 0.6820004458491113475, -57.25054294077229144 ) ) ;
#9138 = CARTESIAN_POINT ( 'NONE',  ( -238.4067589809705794, 0.9644942799825386714, 0.000000000000000000 ) ) ;
#9139 = CARTESIAN_POINT ( 'NONE',  ( 14.38125909742180397, 67.30136555895953165, 10.73282306403583242 ) ) ;
#9140 = ADVANCED_FACE ( 'NONE', ( #5147 ), #20652, .T. ) ;
#9141 = CARTESIAN_POINT ( 'NONE',  ( -192.9588430854689989, -8.596193650988133061E-14, 14.46834944099969533 ) ) ;
#9142 = CARTESIAN_POINT ( 'NONE',  ( -213.1075012329537230, -66.26714140136188291, -9.698598906438677503 ) ) ;
#9143 = VECTOR ( 'NONE', #26035, 1000.000000000000000 ) ;
#9144 = EDGE_CURVE ( 'NONE', #60, #19515, #22358, .T. ) ;
#9145 = CARTESIAN_POINT ( 'NONE',  ( -144.0562564043591749, 29.54282788297669171, -14.68019405981451797 ) ) ;
#9146 = ORIENTED_EDGE ( 'NONE', *, *, #8930, .F. ) ;
#9147 = CARTESIAN_POINT ( 'NONE',  ( 163.1118516004056573, 9.006482792069629539, 9.006482792069634868 ) ) ;
#9148 = CARTESIAN_POINT ( 'NONE',  ( 190.0000000000000000, -71.50000000000002842, 66.50000000000005684 ) ) ;
#9149 = CARTESIAN_POINT ( 'NONE',  ( 23.36462152322932440, 13.80148662728997699, 46.81175967489703282 ) ) ;
#9150 = CARTESIAN_POINT ( 'NONE',  ( -39.81953879992323664, -32.18669035975747761, -16.38089232953674923 ) ) ;
#9151 = ADVANCED_FACE ( 'NONE', ( #11493 ), #22198, .T. ) ;
#9152 = ADVANCED_FACE ( 'NONE', ( #10527 ), #2550, .F. ) ;
#9153 = VERTEX_POINT ( 'NONE', #8259 ) ;
#9154 = CARTESIAN_POINT ( 'NONE',  ( -105.3239185089454395, 18.58330222739251525, 10.72756532555027853 ) ) ;
#9155 = B_SPLINE_CURVE_WITH_KNOTS ( 'NONE', 3,
 ( #19271, #19651, #23403, #5178, #4920, #21278 ),
 .UNSPECIFIED., .F., .F.,
 ( 4, 2, 4 ),
 ( -0.0001050551439274930278, 0.04006586859758504843, 0.08023679233909759845 ),
 .UNSPECIFIED. ) ;
#9156 = AXIS2_PLACEMENT_3D ( 'NONE', #23546, #11423, #15419 ) ;
#9157 = CARTESIAN_POINT ( 'NONE',  ( 199.9999999999999432, -6.993216068016765874, -17.67234381275832433 ) ) ;
#9158 = CARTESIAN_POINT ( 'NONE',  ( 23.48902902575118645, -23.31625887490708848, 42.82177761400734539 ) ) ;
#9159 = CARTESIAN_POINT ( 'NONE',  ( 45.01779936580098962, 12.15764947728268019, -38.89115870269903752 ) ) ;
#9160 = CARTESIAN_POINT ( 'NONE',  ( 199.0079837170424923, 19.96494570524563272, -1.290871210190707608 ) ) ;
#9161 = AXIS2_PLACEMENT_3D ( 'NONE', #4159, #20110, #3745 ) ;
#9162 = CARTESIAN_POINT ( 'NONE',  ( 184.8905102610680444, -41.77492675556007384, 14.79361573936348684 ) ) ;
#9163 = CARTESIAN_POINT ( 'NONE',  ( -105.3755690713226727, 5.661656051307470077E-14, -21.75974354311649961 ) ) ;
#9164 = CARTESIAN_POINT ( 'NONE',  ( 184.8905102610680444, 1.070102760522089011E-13, -20.92133201514444352 ) ) ;
#9165 = CARTESIAN_POINT ( 'NONE',  ( 14.32711937312299177, 49.08922911798419619, -14.14294248749816596 ) ) ;
#9166 = CARTESIAN_POINT ( 'NONE',  ( -208.1127848780264742, -55.00245453012676222, -2.449293598294708485E-15 ) ) ;
#9168 = CARTESIAN_POINT ( 'NONE',  ( 192.4448373802100889, 14.14213562375893574, -14.14213562375874922 ) ) ;
#9167 = CARTESIAN_POINT ( 'NONE',  ( 21.25019396253522430, -18.04326867293554315, -43.56030393974957349 ) ) ;
#9169 = CARTESIAN_POINT ( 'NONE',  ( 192.4448373802101173, 20.00000000003945644, 40.00000000000002132 ) ) ;
#9171 = CARTESIAN_POINT ( 'NONE',  ( -30.26275506840324070, -1.198031551616032919, 1.198031551616014712 ) ) ;
#9170 = AXIS2_PLACEMENT_3D ( 'NONE', #7766, #22163, #13500 ) ;
#9172 = CARTESIAN_POINT ( 'NONE',  ( -91.56559293963836410, 40.00000000000019185, -17.32597176626768487 ) ) ;
#9173 = CARTESIAN_POINT ( 'NONE',  ( -110.0563856372988596, 9.155970533494683039, -17.99047586673238541 ) ) ;
#9174 = CARTESIAN_POINT ( 'NONE',  ( 14.38125909742181818, -39.99999999999986500, -15.17850393972675604 ) ) ;
#9175 = CARTESIAN_POINT ( 'NONE',  ( -192.9588430854690273, -40.00000000000011369, 14.46834944099955855 ) ) ;
#9176 = AXIS2_PLACEMENT_3D ( 'NONE', #19103, #25622, #1398 ) ;
#9177 = CARTESIAN_POINT ( 'NONE',  ( 130.1158308416293892, -29.33435477745536701, -12.15068759228604911 ) ) ;
#9178 = CARTESIAN_POINT ( 'NONE',  ( -162.0762913951021176, 29.48230308784730980, 27.08623940707652622 ) ) ;
#9179 = CARTESIAN_POINT ( 'NONE',  ( -213.1075012329537230, 18.58567234101121102, 37.98287015391247223 ) ) ;
#9180 = VERTEX_POINT ( 'NONE', #22908 ) ;
#9182 = CARTESIAN_POINT ( 'NONE',  ( -4.037857402783659566, 43.00569567200389542, -23.44963359339821096 ) ) ;
#9181 = CARTESIAN_POINT ( 'NONE',  ( -210.0000000000000284, -66.50000000000001421, 66.50000000000005684 ) ) ;
#9183 = CARTESIAN_POINT ( 'NONE',  ( -135.8532207217289738, 9.153146818113548022, 40.00000000000002132 ) ) ;
#9184 = CARTESIAN_POINT ( 'NONE',  ( 19.06497207195980792, 10.03556273973447155, -10.03556273973422286 ) ) ;
#9185 = CARTESIAN_POINT ( 'NONE',  ( -199.9999999999998010, 49.28189405767604114, -14.17215463606931181 ) ) ;
#9186 = ORIENTED_EDGE ( 'NONE', *, *, #6541, .F. ) ;
#9187 = ORIENTED_EDGE ( 'NONE', *, *, #22256, .T. ) ;
#9188 = VECTOR ( 'NONE', #16664, 1000.000000000000000 ) ;
#9189 = CARTESIAN_POINT ( 'NONE',  ( -56.48582580120559271, 6.472252184284211118, -6.472252184284153387 ) ) ;
#9190 = CARTESIAN_POINT ( 'NONE',  ( 98.29820294267319980, -18.47759065023120328, -7.653668647304143313 ) ) ;
#9191 = ORIENTED_EDGE ( 'NONE', *, *, #5719, .F. ) ;
#9192 = ORIENTED_EDGE ( 'NONE', *, *, #18043, .T. ) ;
#9193 = CARTESIAN_POINT ( 'NONE',  ( 200.0000000000000000, -12.54535540268124372, 14.29661512548269187 ) ) ;
#9194 = CARTESIAN_POINT ( 'NONE',  ( -188.7701069479165881, 13.85300054332491904, 47.15820909662593863 ) ) ;
#9195 = AXIS2_PLACEMENT_3D ( 'NONE', #1577, #11534, #9816 ) ;
#9196 = CARTESIAN_POINT ( 'NONE',  ( 192.4448373802101173, -42.42640687122073473, 14.14213562370301780 ) ) ;
#9197 = CARTESIAN_POINT ( 'NONE',  ( -190.0000000000000000, -52.49999999999991473, 52.49999999999999289 ) ) ;
#9198 = CARTESIAN_POINT ( 'NONE',  ( 192.4448373802100889, 1.051811698935164031E-13, -20.00000000003942091 ) ) ;
#9199 = DIRECTION ( 'NONE',  ( 0.000000000000000000, -1.000000000000000000, 0.000000000000000000 ) ) ;
#9200 = CARTESIAN_POINT ( 'NONE',  ( 180.0000000000000284, -115.7889608577475542, -82.49999999999998579 ) ) ;
#9201 = CARTESIAN_POINT ( 'NONE',  ( 163.1118516004056573, -40.00000000000027711, 27.26290988616830546 ) ) ;
#9202 = CARTESIAN_POINT ( 'NONE',  ( 19.06497207195980792, 40.00000000000059686, -54.19242893257802507 ) ) ;
#9203 = DIRECTION ( 'NONE',  ( 0.000000000000000000, 1.000000000000000000, 0.000000000000000000 ) ) ;
#9204 = VECTOR ( 'NONE', #3157, 1000.000000000000000 ) ;
#9205 = CARTESIAN_POINT ( 'NONE',  ( -259.2033419157646676, -49.83842185052031937, -6.730120644403796426 ) ) ;
#9206 = CARTESIAN_POINT ( 'NONE',  ( 151.7948205124836250, 1.439163438361279259E-13, -33.23291073765553705 ) ) ;
#9207 = CARTESIAN_POINT ( 'NONE',  ( -200.5022718138936852, 18.58571273880625085, 44.86987976039401360 ) ) ;
#9208 = CARTESIAN_POINT ( 'NONE',  ( 151.0853911467767432, 29.06993079631213206, 12.04115959307993045 ) ) ;
#9209 = CARTESIAN_POINT ( 'NONE',  ( -105.2054292635175727, 7.329160573984922335E-13, -21.49321519473985020 ) ) ;
#9210 = DIRECTION ( 'NONE',  ( 0.000000000000000000, 0.000000000000000000, -1.000000000000000000 ) ) ;
#9211 = CARTESIAN_POINT ( 'NONE',  ( -86.94888381181661430, -19.08739374733235650, 9.627065680632176381 ) ) ;
#9212 = CARTESIAN_POINT ( 'NONE',  ( 200.0000000000000000, -14.14213562373106114, 42.42640687119278908 ) ) ;
#9213 = CARTESIAN_POINT ( 'NONE',  ( -56.48582580120559982, -21.81201906317804173, 34.75652343174591152 ) ) ;
#9214 = CARTESIAN_POINT ( 'NONE',  ( -114.4388184736417031, -8.352332320009672628, -20.16431396440397350 ) ) ;
#9215 = DIRECTION ( 'NONE',  ( -1.000000000000000000, -1.836970198721030181E-16, 0.000000000000000000 ) ) ;
#9216 = VERTEX_POINT ( 'NONE', #6272 ) ;
#9217 = CARTESIAN_POINT ( 'NONE',  ( -198.0356074513804572, 39.15871834505956173, -39.15871834505865223 ) ) ;
#9218 = LINE ( 'NONE', #19451, #22619 ) ;
#9219 = CIRCLE ( 'NONE', #23242, 15.00000000000000178 ) ;
#9220 = AXIS2_PLACEMENT_3D ( 'NONE', #5727, #143, #16364 ) ;
#9221 = DIRECTION ( 'NONE',  ( 1.000000000000000000, 0.000000000000000000, 0.000000000000000000 ) ) ;
#9222 = ORIENTED_EDGE ( 'NONE', *, *, #3391, .T. ) ;
#9223 = CARTESIAN_POINT ( 'NONE',  ( -56.48582580120558561, -40.00000000000012790, 9.153146818113166105 ) ) ;
#9224 = CARTESIAN_POINT ( 'NONE',  ( 199.0254832151936171, -18.68063995892892137, 7.159751105900188151 ) ) ;
#9225 = CARTESIAN_POINT ( 'NONE',  ( 5.009866156928164393, -44.71726210619349473, 24.71463403307577877 ) ) ;
#9226 = ORIENTED_EDGE ( 'NONE', *, *, #12729, .T. ) ;
#9227 = VERTEX_POINT ( 'NONE', #14639 ) ;
#9228 = CARTESIAN_POINT ( 'NONE',  ( -238.4067589809705794, 40.96449427990177128, 40.00000000000002132 ) ) ;
#9229 = CARTESIAN_POINT ( 'NONE',  ( 199.9999999999999432, 14.14213562373113398, -14.14213562373094923 ) ) ;
#9230 = EDGE_CURVE ( 'NONE', #12861, #21077, #20513, .T. ) ;
#9231 = CARTESIAN_POINT ( 'NONE',  ( 146.6084372240433709, 40.00000000000003553, 5.374981219217116468 ) ) ;
#9232 = FILL_AREA_STYLE_COLOUR ( '', #20192 ) ;
#9233 = CONICAL_SURFACE ( 'NONE', #17237, 19.53474504356807273, 0.7853981633974447263 ) ;
#9234 = CARTESIAN_POINT ( 'NONE',  ( -77.84460141634575336, -19.81807444411877128, 9.302297467149831078 ) ) ;
#9235 = CARTESIAN_POINT ( 'NONE',  ( -86.96347745069644475, 5.999880687339585546E-14, -21.75974354311649961 ) ) ;
#9236 = CARTESIAN_POINT ( 'NONE',  ( 199.9999999999999716, -6.704437273156823807, -17.78382994799445527 ) ) ;
#9237 = ADVANCED_FACE ( 'NONE', ( #12788, #20915, #2694, #10799, #4296, #12386 ), #18910, .F. ) ;
#9238 = CARTESIAN_POINT ( 'NONE',  ( -77.58456302900343360, 13.58506799361890671, 17.49509851286743611 ) ) ;
#9239 = CARTESIAN_POINT ( 'NONE',  ( -100.7734535825088358, -16.03295912088728770, 16.03295912088687913 ) ) ;
#9240 = CARTESIAN_POINT ( 'NONE',  ( 151.7948205124835681, 51.78348778862544322, -4.785054706298002891 ) ) ;
#9241 = FACE_OUTER_BOUND ( 'NONE', #1108, .T. ) ;
#9242 = CARTESIAN_POINT ( 'NONE',  ( -280.0000000000000000, 1.605030083646939673E-13, -20.00000000000001421 ) ) ;
#9243 = CARTESIAN_POINT ( 'NONE',  ( 48.46046615278249448, 11.89583623203300888, 37.63122026539858211 ) ) ;
#9244 = CARTESIAN_POINT ( 'NONE',  ( 151.7948205124836534, -6.767089262349000656, -40.00000000000002132 ) ) ;
#9245 = ADVANCED_FACE ( 'NONE', ( #425 ), #13335, .T. ) ;
#9246 = CARTESIAN_POINT ( 'NONE',  ( -213.1075012329537230, 18.58567234101121102, 37.98287015391247223 ) ) ;
#9247 = CARTESIAN_POINT ( 'NONE',  ( -238.4067589809705794, -0.9644942799826263791, -40.00000000000002132 ) ) ;
#9249 = CARTESIAN_POINT ( 'NONE',  ( -162.0762913951021176, 39.99999999999998579, 1.694272876828463614 ) ) ;
#9248 = CARTESIAN_POINT ( 'NONE',  ( -105.2110227778633487, 1.366831978265802938, 21.45666521040861241 ) ) ;
#9250 = CARTESIAN_POINT ( 'NONE',  ( -114.7706029183787848, 22.06581648165141374, -1.595391203485450271 ) ) ;
#9251 = CARTESIAN_POINT ( 'NONE',  ( -91.56559293963834989, 12.25131212657480440, 12.25131212657486834 ) ) ;
#9252 = CARTESIAN_POINT ( 'NONE',  ( 19.06497207195980792, 54.19242893257843718, 2.449293598294708485E-15 ) ) ;
#9253 = EDGE_LOOP ( 'NONE', ( #20479, #13421 ) ) ;
#9254 = EDGE_CURVE ( 'NONE', #3826, #5421, #12430, .T. ) ;
#9255 = CARTESIAN_POINT ( 'NONE',  ( 21.60666276257580876, -43.47550165075017503, 18.00814241471809751 ) ) ;
#9256 = CARTESIAN_POINT ( 'NONE',  ( -105.3175882261743226, 18.50843658928782531, -10.85998092708147666 ) ) ;
#9257 = CARTESIAN_POINT ( 'NONE',  ( -208.1127848780264742, 10.60833733270764867, 67.17687982763166588 ) ) ;
#9258 = CARTESIAN_POINT ( 'NONE',  ( -162.0762913951020892, -3.568845385355699554E-14, 1.694272876828323948 ) ) ;
#9259 = CARTESIAN_POINT ( 'NONE',  ( -82.23674992913811366, 20.20616381366022196, -1.119577663962783909 ) ) ;
#9260 = CARTESIAN_POINT ( 'NONE',  ( -62.69292774213263897, 9.343531400584703661, -25.97703433367446380 ) ) ;
#9261 = CARTESIAN_POINT ( 'NONE',  ( 199.9999999999996589, 6.678198862535981384, 17.79829383751451388 ) ) ;
#9262 = CARTESIAN_POINT ( 'NONE',  ( -654.8952864718139608, 38.45762375594820526, -11.01125294513469122 ) ) ;
#9263 = CARTESIAN_POINT ( 'NONE',  ( -77.61421004775742460, 3.464448011081117773, -21.81743058566524951 ) ) ;
#9264 = CARTESIAN_POINT ( 'NONE',  ( 4.995406935893283773, 39.06748935135171052, 17.50105314357239195 ) ) ;
#9265 = CARTESIAN_POINT ( 'NONE',  ( -280.0000000000000000, -14.14213562373088706, -14.14213562373108424 ) ) ;
#9266 = CARTESIAN_POINT ( 'NONE',  ( -56.48582580120558561, 6.472252184283903809, 50.09629031063968796 ) ) ;
#9267 = CARTESIAN_POINT ( 'NONE',  ( 146.6084372240433993, -24.48358557860353457, 24.48358557860296258 ) ) ;
#9268 = CARTESIAN_POINT ( 'NONE',  ( 136.1360204305621551, 24.77266263493153176, -31.79587985999237887 ) ) ;
#9270 = CARTESIAN_POINT ( 'NONE',  ( -135.8532207217289738, -34.75652343174584757, -21.81201906317816253 ) ) ;
#9269 = CARTESIAN_POINT ( 'NONE',  ( 19.06497207195981858, -10.03556273973377166, -66.60410523465827737 ) ) ;
#9271 = CARTESIAN_POINT ( 'NONE',  ( -208.1127848780264742, 10.60833733268383483, -67.17687982760675425 ) ) ;
#9272 = CARTESIAN_POINT ( 'NONE',  ( -100.7734535825088358, -22.67402823373193499, 0.000000000000000000 ) ) ;
#9273 = FACE_BOUND ( 'NONE', #4827, .T. ) ;
#9274 = DIRECTION ( 'NONE',  ( 0.000000000000000000, -1.000000000000000000, 0.000000000000000000 ) ) ;
#9275 = CARTESIAN_POINT ( 'NONE',  ( 19.06497207195981858, -38.31983398719641087, 18.24870850772724040 ) ) ;
#9276 = CARTESIAN_POINT ( 'NONE',  ( -185.5190358318141932, 42.39054933786154322, -17.55874045218388346 ) ) ;
#9277 = ORIENTED_EDGE ( 'NONE', *, *, #6868, .F. ) ;
#9278 = CARTESIAN_POINT ( 'NONE',  ( 91.82158438592158234, 44.40256751092336884, -12.16597498400043342 ) ) ;
#9279 = CARTESIAN_POINT ( 'NONE',  ( -190.1760717698577423, 23.85870456551995744, 43.55712811721888045 ) ) ;
#9280 = CARTESIAN_POINT ( 'NONE',  ( 23.17367289774858108, 13.81211338457322846, 46.88342923877236501 ) ) ;
#9281 = CARTESIAN_POINT ( 'NONE',  ( -87.13361725327072804, -21.49321519333431141, -3.542586001259484843E-15 ) ) ;
#9282 = ORIENTED_EDGE ( 'NONE', *, *, #8487, .F. ) ;
#9283 = CARTESIAN_POINT ( 'NONE',  ( -151.7004365447935754, -32.50163950444082417, 13.46261988216328120 ) ) ;
#9284 = CARTESIAN_POINT ( 'NONE',  ( 200.0000000000002558, 2.008769787671115026, -18.89534854373681938 ) ) ;
#9285 = CARTESIAN_POINT ( 'NONE',  ( 22.33254948917040750, -17.93222939140373384, 43.29223140032068784 ) ) ;
#9286 = AXIS2_PLACEMENT_3D ( 'NONE', #7227, #3501, #13474 ) ;
#9287 = ADVANCED_FACE ( 'NONE', ( #18419 ), #12173, .F. ) ;
#9288 = B_SPLINE_CURVE_WITH_KNOTS ( 'NONE', 3,
 ( #8813, #16924, #2295, #21055, #2840, #1472, #7193, #7570, #13316, #23436, #9575, #7443 ),
 .UNSPECIFIED., .F., .F.,
 ( 4, 2, 2, 2, 2, 4 ),
 ( 2.797157557069881010E-17, 0.005971652981263651967, 0.008957479471895464507, 0.01045039271721137121, 0.01119684933986928033, 0.01194330596252718944 ),
 .UNSPECIFIED. ) ;
#9289 = CARTESIAN_POINT ( 'NONE',  ( 90.71510531247511722, 8.810647085256718469, -21.27078368625871718 ) ) ;
#9290 = CARTESIAN_POINT ( 'NONE',  ( 199.0060114145493912, 8.242208747961328186, -18.21796198456784666 ) ) ;
#9291 = EDGE_CURVE ( 'NONE', #25465, #14912, #24666, .T. ) ;
#9292 = CARTESIAN_POINT ( 'NONE',  ( -77.55640685876512919, -9.396736996787174904E-14, 22.13135000837103661 ) ) ;
#9293 = CARTESIAN_POINT ( 'NONE',  ( 184.8905102610680444, 39.99999999999999289, 19.07866798485573057 ) ) ;
#9294 = FACE_OUTER_BOUND ( 'NONE', #17839, .T. ) ;
#9295 = CARTESIAN_POINT ( 'NONE',  ( 7.340276806054842673, 49.28408872342602365, -14.17250878947606907 ) ) ;
#9296 = CARTESIAN_POINT ( 'NONE',  ( -259.2033419157646676, -30.48217210827743884, -40.00000000000002132 ) ) ;
#9298 = CARTESIAN_POINT ( 'NONE',  ( -599.8048379379712287, 37.93045404823428868, -12.70834960012116710 ) ) ;
#9297 = FACE_OUTER_BOUND ( 'NONE', #10936, .T. ) ;
#9299 = ADVANCED_FACE ( 'NONE', ( #6058 ), #18282, .F. ) ;
#9300 = CARTESIAN_POINT ( 'NONE',  ( -238.4067589809705794, -0.9644942799826263791, 40.00000000000002132 ) ) ;
#9301 = CARTESIAN_POINT ( 'NONE',  ( -192.9588430854689989, -10.23066800230756890, 10.23066800230742501 ) ) ;
#9302 = CARTESIAN_POINT ( 'NONE',  ( -213.1075012329537230, 40.00000000000012790, -13.71589010951869980 ) ) ;
#9303 = CARTESIAN_POINT ( 'NONE',  ( -192.9588430854690273, -39.99999999999991473, -14.46834944100011633 ) ) ;
#9304 = CARTESIAN_POINT ( 'NONE',  ( 110.0526450532112648, -22.72553370033782016, -9.413224270846754393 ) ) ;
#9305 = EDGE_LOOP ( 'NONE', ( #23894, #12227, #19972, #9737 ) ) ;
#9307 = CARTESIAN_POINT ( 'NONE',  ( -4.260882601030786532, 42.93997571557897430, -23.40615483283743714 ) ) ;
#9306 = DIRECTION ( 'NONE',  ( -1.000000000000000000, -0.000000000000000000, -0.000000000000000000 ) ) ;
#9308 = CARTESIAN_POINT ( 'NONE',  ( -192.9588430854690273, -54.46834944098226572, 40.00000000000002132 ) ) ;
#9309 = SURFACE_STYLE_USAGE ( .BOTH. , #7554 ) ;
#9310 = CARTESIAN_POINT ( 'NONE',  ( -198.9234529669418521, 44.84148137680994495, -24.80620787425045393 ) ) ;
#9311 = ORIENTED_EDGE ( 'NONE', *, *, #10302, .F. ) ;
#9312 = ORIENTED_EDGE ( 'NONE', *, *, #22980, .T. ) ;
#9313 = LINE ( 'NONE', #7308, #19368 ) ;
#9314 = CARTESIAN_POINT ( 'NONE',  ( 137.0939645874030930, 12.56330697291270049, -30.33050608226187705 ) ) ;
#9315 = AXIS2_PLACEMENT_3D ( 'NONE', #19681, #25823, #11189 ) ;
#9316 = ORIENTED_EDGE ( 'NONE', *, *, #3118, .T. ) ;
#9317 = ORIENTED_EDGE ( 'NONE', *, *, #1264, .F. ) ;
#9318 = CARTESIAN_POINT ( 'NONE',  ( 199.9999999999998295, 0.2943743412949595961, 19.00910698902408669 ) ) ;
#9319 = CYLINDRICAL_SURFACE ( 'NONE', #8572, 31.79780246617542616 ) ;
#9320 = CARTESIAN_POINT ( 'NONE',  ( -91.56559293963834989, 40.53558337403677569, -16.03295912088699993 ) ) ;
#9321 = CARTESIAN_POINT ( 'NONE',  ( 170.0000000000000853, 9.369682556672316309, -22.62041470344884075 ) ) ;
#9322 = CARTESIAN_POINT ( 'NONE',  ( -91.56559293963834989, 6.234561990864368500E-14, -22.67402823373191723 ) ) ;
#9323 = CARTESIAN_POINT ( 'NONE',  ( 170.0000000000000000, 3.122849337825751958E-14, 0.000000000000000000 ) ) ;
#9324 = DIRECTION ( 'NONE',  ( 9.935246354362821010E-15, 0.7071067811865517916, -0.7071067811865432429 ) ) ;
#9325 = CARTESIAN_POINT ( 'NONE',  ( 98.29820294267314296, 18.47759065023127079, 7.653668647304075812 ) ) ;
#9326 = CARTESIAN_POINT ( 'NONE',  ( -135.8532207217289738, -39.99999999999972289, -30.84685318188688541 ) ) ;
#9327 = CARTESIAN_POINT ( 'NONE',  ( 151.7948205124836250, 1.012150473917908975E-13, -6.767089262349031742 ) ) ;
#9328 = DIRECTION ( 'NONE',  ( 1.000000000000000000, 1.836970198721030181E-16, 0.000000000000000000 ) ) ;
#9329 = CARTESIAN_POINT ( 'NONE',  ( -198.0356074513804572, -10.87444709759729911, 10.87444709759714812 ) ) ;
#9330 = CARTESIAN_POINT ( 'NONE',  ( 184.8905102610680444, 40.00000000000013500, -20.92133201514430141 ) ) ;
#9331 = EDGE_CURVE ( 'NONE', #4727, #525, #16747, .T. ) ;
#9332 = CARTESIAN_POINT ( 'NONE',  ( -192.9370391625440959, 24.26711063095210363, 44.11033075277109106 ) ) ;
#9333 = CARTESIAN_POINT ( 'NONE',  ( 135.5356265174576151, 30.20731421070342293, 12.51227922893899525 ) ) ;
#9334 = CIRCLE ( 'NONE', #3815, 44.99999999999997158 ) ;
#9335 = DIRECTION ( 'NONE',  ( 0.000000000000000000, -1.000000000000000000, 2.775557561562890858E-16 ) ) ;
#9336 = FACE_OUTER_BOUND ( 'NONE', #18904, .T. ) ;
#9337 = CARTESIAN_POINT ( 'NONE',  ( -77.72936527557085640, -19.09948130763599750, 10.88227939678934142 ) ) ;
#9338 = CARTESIAN_POINT ( 'NONE',  ( 91.82158438592158234, -40.45024623143958564, 16.11829626348418998 ) ) ;
#9339 = CARTESIAN_POINT ( 'NONE',  ( 163.1118516004056573, -37.29075403953166301, 19.27778845539196695 ) ) ;
#9340 = CARTESIAN_POINT ( 'NONE',  ( -185.5190930960787057, -17.55874694108960199, -42.39056500338028854 ) ) ;
#9341 = CARTESIAN_POINT ( 'NONE',  ( 8.517493242715987734, 24.85395068094660687, 44.90626920808405487 ) ) ;
#9342 = VERTEX_POINT ( 'NONE', #2071 ) ;
#9343 = CARTESIAN_POINT ( 'NONE',  ( 19.06497207195981147, 38.31983398719673772, -38.31983398719579981 ) ) ;
#9344 = CARTESIAN_POINT ( 'NONE',  ( -626.9846540392142060, -82.50099999999990530, 0.000000000000000000 ) ) ;
#9345 = LINE ( 'NONE', #7215, #1701 ) ;
#9346 = ORIENTED_EDGE ( 'NONE', *, *, #11744, .F. ) ;
#9347 = CARTESIAN_POINT ( 'NONE',  ( 136.1360204305621551, -40.00000000000036238, 35.03383547441254109 ) ) ;
#9348 = CARTESIAN_POINT ( 'NONE',  ( 199.0196838869227633, -18.24539314265820877, -8.197241283090187736 ) ) ;
#9349 = ORIENTED_EDGE ( 'NONE', *, *, #22155, .T. ) ;
#9350 = ORIENTED_EDGE ( 'NONE', *, *, #19871, .F. ) ;
#9351 = CARTESIAN_POINT ( 'NONE',  ( -162.0762913951021176, -29.48230308784755493, -27.08623940707632372 ) ) ;
#9352 = CARTESIAN_POINT ( 'NONE',  ( -208.1127848780264742, 39.99999999999992895, 15.00245453012683683 ) ) ;
#9353 = CARTESIAN_POINT ( 'NONE',  ( -88.38011429825068888, -20.03522015641036447, -8.298859913963124058 ) ) ;
#9354 = AXIS2_PLACEMENT_3D ( 'NONE', #20115, #14385, #5739 ) ;
#9355 = CARTESIAN_POINT ( 'NONE',  ( 151.7948205124836250, 4.785054706301759886, -4.785054706301612448 ) ) ;
#9356 = CARTESIAN_POINT ( 'NONE',  ( -86.96347745069643054, -39.99999999999995737, -21.75974354311664527 ) ) ;
#9357 = CARTESIAN_POINT ( 'NONE',  ( 200.0000000000000000, -19.00702131438069031, 0.3144861700050793352 ) ) ;
#9358 = CARTESIAN_POINT ( 'NONE',  ( -82.23726319249655603, 14.28014421912408771, 14.28014421912425114 ) ) ;
#9359 = CARTESIAN_POINT ( 'NONE',  ( -17.28139728231930405, -20.85871090883866685, -39.07633224428978025 ) ) ;
#9360 = CARTESIAN_POINT ( 'NONE',  ( 57.59792236341147031, 30.00663442387720181, -26.56190807104661289 ) ) ;
#9361 = CARTESIAN_POINT ( 'NONE',  ( -83.28983882461055543, -35.99236576815650324, -3.542586001259484843E-15 ) ) ;
#9362 = CARTESIAN_POINT ( 'NONE',  ( -30.26275506840323359, -39.99999999999959499, -41.69427246844670520 ) ) ;
#9363 = LINE ( 'NONE', #9492, #23198 ) ;
#9364 = CARTESIAN_POINT ( 'NONE',  ( 192.4448373802101173, -19.99999999996057554, 40.00000000000002132 ) ) ;
#9365 = CARTESIAN_POINT ( 'NONE',  ( 163.1118516004056573, -12.73709011382471878, -40.00000000000002132 ) ) ;
#9366 = CARTESIAN_POINT ( 'NONE',  ( -135.8532207217289738, 6.472252184284186249, -6.472252184284142729 ) ) ;
#9367 = CARTESIAN_POINT ( 'NONE',  ( 0.2972598230770129857, -54.33493731733936016, -40.00000000000002132 ) ) ;
#9368 = CIRCLE ( 'NONE', #8033, 20.53474504356812247 ) ;
#9370 = FACE_OUTER_BOUND ( 'NONE', #18612, .T. ) ;
#9369 = DIRECTION ( 'NONE',  ( 0.2259624730582905916, 0.000000000000000000, -0.9741360073261747798 ) ) ;
#9371 = CARTESIAN_POINT ( 'NONE',  ( -114.6557802242318616, 21.44605415401110093, 5.040599680926282744 ) ) ;
#9372 = CARTESIAN_POINT ( 'NONE',  ( -30.26275506840323715, 29.48230279907789253, 29.48230279907799556 ) ) ;
#9373 = CARTESIAN_POINT ( 'NONE',  ( -86.96347745069644475, 18.24025645688350750, -40.00000000000002132 ) ) ;
#9374 = ORIENTED_EDGE ( 'NONE', *, *, #22018, .T. ) ;
#9375 = CARTESIAN_POINT ( 'NONE',  ( 23.26364522860156825, -46.84987168986953776, 13.80713620122656948 ) ) ;
#9376 = ADVANCED_FACE ( 'NONE', ( #2204 ), #14297, .T. ) ;
#9377 = CARTESIAN_POINT ( 'NONE',  ( -83.21262154144250189, 33.12752917118434226, -13.72187187061452995 ) ) ;
#9378 = CARTESIAN_POINT ( 'NONE',  ( 4.995406935893297096, 10.78321810387837232, 67.35176059880234334 ) ) ;
#9379 = CARTESIAN_POINT ( 'NONE',  ( -56.48582580120559271, 2.158176344243877536E-14, -9.153146818113587102 ) ) ;
#9380 = CARTESIAN_POINT ( 'NONE',  ( -77.81429512171635565, 20.74621013857194995, 7.173374844106962911 ) ) ;
#9381 = CIRCLE ( 'NONE', #1318, 5.000000000000004441 ) ;
#9382 = CIRCLE ( 'NONE', #24276, 29.99999999999999645 ) ;
#9383 = CARTESIAN_POINT ( 'NONE',  ( -16.37606550795825200, 16.46709356870534435, -39.75508062650778385 ) ) ;
#9384 = CARTESIAN_POINT ( 'NONE',  ( 200.0000000000001421, 9.088304224312857116, 16.69380151103622012 ) ) ;
#9385 = DIRECTION ( 'NONE',  ( 1.000000000000000000, 0.000000000000000000, 0.000000000000000000 ) ) ;
#9386 = EDGE_CURVE ( 'NONE', #14641, #9227, #10713, .T. ) ;
#9387 = CARTESIAN_POINT ( 'NONE',  ( -77.72936527556018405, -5.810439193549020942, -21.20030630601272748 ) ) ;
#9388 = CARTESIAN_POINT ( 'NONE',  ( -86.96347745069644475, -15.38646221621807442, 15.38646221621768184 ) ) ;
#9389 = CARTESIAN_POINT ( 'NONE',  ( 184.8905102610680444, 43.07788698682591644, -13.49065550809769221 ) ) ;
#9390 = EDGE_CURVE ( 'NONE', #1078, #22053, #17341, .T. ) ;
#9391 = CARTESIAN_POINT ( 'NONE',  ( -114.7711211671578724, 22.06863527409988990, -1.563052705007634158 ) ) ;
#9392 = DIRECTION ( 'NONE',  ( -1.000000000000000000, 0.000000000000000000, 0.000000000000000000 ) ) ;
#9393 = CARTESIAN_POINT ( 'NONE',  ( 19.06497207195980792, 18.24870850772790831, -38.31983398719609824 ) ) ;
#9395 = CARTESIAN_POINT ( 'NONE',  ( -86.96347745069644475, -15.38646221621738164, -41.18208027870615240 ) ) ;
#9394 = CARTESIAN_POINT ( 'NONE',  ( -100.7734535825088500, 16.03295912088740494, -40.53558337403661938 ) ) ;
#9396 = CARTESIAN_POINT ( 'NONE',  ( 91.82158438592158234, 44.40256751092319121, 12.16597498400105515 ) ) ;
#9397 = CARTESIAN_POINT ( 'NONE',  ( 91.82158438592158234, -17.20528682183298486, 0.000000000000000000 ) ) ;
#9398 = CARTESIAN_POINT ( 'NONE',  ( -612.0709805440841365, -1.322736627157445917E-16, 0.000000000000000000 ) ) ;
#9399 = DIRECTION ( 'NONE',  ( 1.000000000000000000, -0.000000000000000000, -0.000000000000000000 ) ) ;
#9400 = CARTESIAN_POINT ( 'NONE',  ( -259.2033419157646676, 6.730120644403426944, 6.730120644403592145 ) ) ;
#9401 = VECTOR ( 'NONE', #18233, 1000.000000000000000 ) ;
#9402 = CARTESIAN_POINT ( 'NONE',  ( 136.1360204305621551, -35.03383547441293899, 40.00000000000002132 ) ) ;
#9404 = ORIENTED_EDGE ( 'NONE', *, *, #14642, .T. ) ;
#9403 = B_SPLINE_CURVE_WITH_KNOTS ( 'NONE', 3,
 ( #14410, #8282, #18399, #24399, #176, #18262, #16408, #22412, #22276, #4320, #6292, #22671 ),
 .UNSPECIFIED., .F., .F.,
 ( 4, 2, 2, 2, 2, 4 ),
 ( 5.572756979560850756E-17, 0.004680202113613629415, 0.009360404227227203319, 0.01170050528403401152, 0.01404060634084081972, 0.01872080845445443439 ),
 .UNSPECIFIED. ) ;
#9405 = CARTESIAN_POINT ( 'NONE',  ( -280.0000000000000568, 14.14213562373097943, -42.42640687119285303 ) ) ;
#9406 = VECTOR ( 'NONE', #4971, 1000.000000000000000 ) ;
#9407 = CARTESIAN_POINT ( 'NONE',  ( 5.897475806298555945, 43.62364094500643574, 18.06950371951458578 ) ) ;
#9408 = DIRECTION ( 'NONE',  ( -1.000000000000000000, -0.000000000000000000, -0.000000000000000000 ) ) ;
#9409 = CARTESIAN_POINT ( 'NONE',  ( -4.810655158400459541, -42.93528531927712777, -17.78437748360806481 ) ) ;
#9410 = ORIENTED_EDGE ( 'NONE', *, *, #2584, .F. ) ;
#9411 = CARTESIAN_POINT ( 'NONE',  ( -188.3065677117048153, -46.99298756134898269, 13.82848612971595159 ) ) ;
#9412 = CARTESIAN_POINT ( 'NONE',  ( 199.9999999999999716, -15.72304121538119936, -10.67928908684366540 ) ) ;
#9413 = CARTESIAN_POINT ( 'NONE',  ( 23.41418334855255523, -13.79799959793976960, 46.79369727367425469 ) ) ;
#9414 = CARTESIAN_POINT ( 'NONE',  ( 60.28378959954358862, 10.93033916075795808, -33.17072922778727673 ) ) ;
#9415 = CARTESIAN_POINT ( 'NONE',  ( 199.0055623607443636, 10.83365079593514757, -16.80863377785637169 ) ) ;
#9416 = DIRECTION ( 'NONE',  ( 1.000000000000000000, -0.000000000000000000, -0.000000000000000000 ) ) ;
#9417 = CARTESIAN_POINT ( 'NONE',  ( 4.995406935893292655, 39.99999999999982947, 55.24977328856478209 ) ) ;
#9418 = CARTESIAN_POINT ( 'NONE',  ( -105.3755690713226727, 5.661656051307470077E-14, -21.75974354311649961 ) ) ;
#9419 = CARTESIAN_POINT ( 'NONE',  ( -210.0000000000000284, 61.50000000000009237, -66.50000000000005684 ) ) ;
#9420 = CARTESIAN_POINT ( 'NONE',  ( 14.38125909742182884, -55.17850393971007605, 40.00000000000002132 ) ) ;
#9422 = CARTESIAN_POINT ( 'NONE',  ( -619.8916681553856733, 27.37461815474928173, -29.16715517154350934 ) ) ;
#9421 = CARTESIAN_POINT ( 'NONE',  ( -105.4741150117366431, -7.943527260727707429, 19.77569912956141707 ) ) ;
#9423 = CARTESIAN_POINT ( 'NONE',  ( -198.0356074513804572, -15.37879056873074290, 0.000000000000000000 ) ) ;
#9424 = CARTESIAN_POINT ( 'NONE',  ( 130.8568914410475088, 52.36146031193420924, 4.207082182989907437 ) ) ;
#9425 = CARTESIAN_POINT ( 'NONE',  ( 163.1118516004056573, -27.26290988616869626, 0.000000000000000000 ) ) ;
#9426 = CARTESIAN_POINT ( 'NONE',  ( -238.4067589809705794, 39.99999999999999289, -0.9644942799821634161 ) ) ;
#9427 = CARTESIAN_POINT ( 'NONE',  ( -162.0762913951021176, -40.00000000000003553, -1.694272876828743168 ) ) ;
#9428 = CARTESIAN_POINT ( 'NONE',  ( 98.66317599405236649, -18.61194787003555362, -7.709321229950748311 ) ) ;
#9429 = ORIENTED_EDGE ( 'NONE', *, *, #18093, .F. ) ;
#9431 = CARTESIAN_POINT ( 'NONE',  ( -3.993758944536740518, 43.01863922058846157, -23.45926997169882711 ) ) ;
#9430 = CARTESIAN_POINT ( 'NONE',  ( 200.0000000000000000, 75.52305771588345351, -68.47933392563552957 ) ) ;
#9432 = CARTESIAN_POINT ( 'NONE',  ( -100.7734535825088500, -17.32597176626813251, 40.00000000000002132 ) ) ;
#9433 = CARTESIAN_POINT ( 'NONE',  ( -198.0356074513804572, 10.87444709759730088, -10.87444709759707173 ) ) ;
#9434 = CARTESIAN_POINT ( 'NONE',  ( -188.3610564113338626, 43.02325945309135591, -23.46269903113386945 ) ) ;
#9435 = DIRECTION ( 'NONE',  ( -1.000000000000000000, 0.000000000000000000, 0.000000000000000000 ) ) ;
#9436 = ORIENTED_EDGE ( 'NONE', *, *, #8637, .T. ) ;
#9437 = ORIENTED_EDGE ( 'NONE', *, *, #3123, .T. ) ;
#9438 = AXIS2_PLACEMENT_3D ( 'NONE', #19539, #17537, #15664 ) ;
#9439 = LINE ( 'NONE', #15299, #7891 ) ;
#9440 = CARTESIAN_POINT ( 'NONE',  ( -210.0000000000000000, -82.49999999999991473, -52.49999999999977973 ) ) ;
#9441 = ORIENTED_EDGE ( 'NONE', *, *, #880, .F. ) ;
#9442 = ORIENTED_EDGE ( 'NONE', *, *, #26237, .F. ) ;
#9443 = VERTEX_POINT ( 'NONE', #20425 ) ;
#9444 =( BOUNDED_SURFACE ( )  B_SPLINE_SURFACE ( 3, 3, ( 
 ( #7316, #3589, #23557, #23807, #15308, #13820, #25570, #17310, #13563, #17430, #1219, #3465, #15430, #5211, #11435, #1471, #17682, #25824, #5589, #21435, #11694, #19819, #25441, #9707, #17812, #25958, #7701, #11831, #15812, #23938 ),
 ( #3208, #13315, #2132, #18351, #16492, #14096, #9175, #5987, #24216, #10108, #14225, #8103, #20224, #22225, #14489, #131, #11968, #2002, #1871, #8235, #26093, #24617, #18209, #3865, #4141, #22622, #6248, #12100, #14361, #10240 ),
 ( #16224, #12233, #24353, #26233, #6371, #6117, #22364, #4001, #8370, #15947, #22491, #12358, #9842, #24078, #5852, #4397, #18082, #19949, #20357, #13958, #4270, #16353, #24486, #20489, #2262, #10370, #7967, #17946, #18480, #16086 ),
 ( #7829, #22092, #20092, #1733, #261, #9974, #400, #20616, #6505, #24751, #8504, #14615, #16618, #22750, #10504, #12491, #2392, #18618, #13858, #15460, #17462, #5366, #17585, #7224, #9612, #15340, #23712, #17717, #23587, #13471 ),
 ( #3498, #1379, #25721, #21853, #21993, #11345, #15715, #5492, #21464, #11735, #19461, #5622, #7474, #1638, #3625, #25997, #21592, #19853, #9747, #25602, #11465, #15588, #3364, #9231, #13592, #1506, #17847, #11223, #21723, #11597 ),
 ( #3241, #19718, #1248, #23468, #9352, #19592, #9479, #25859, #7603, #5239, #23842, #13728, #1125, #7348, #7734, #15846, #23976, #19336, #5752, #17339, #25472, #13344, #25833, #11443, #1357, #7578, #23442, #9330, #15316, #7201 ),
 ( #11572, #17562, #13703, #15438, #17690, #23565, #17440, #13571, #13322, #15565, #9456, #7451, #9585, #7081, #11078, #5468, #5340, #1226, #5218, #13450, #3342, #21442, #21569, #25578, #9206, #15690, #11323, #19565, #3217, #23815 ) ),
 .UNSPECIFIED., .T., .F., .F. ) 
 B_SPLINE_SURFACE_WITH_KNOTS ( ( 4, 3, 4 ),
 ( 4, 2, 2, 2, 2, 2, 2, 2, 2, 2, 2, 2, 2, 2, 4 ),
 ( 0.000000000000000000, 0.5000000000000000000, 1.000000000000000000 ),
 ( 0.000000000000000000, 0.1357259735107005372, 0.1651108541090157700, 0.1944957347073310028, 0.3598804999793158710, 0.3867117631979620773, 0.4135430264166082281, 0.5789277916885930964, 0.6062785021374117456, 0.6336292125862302838, 0.8508620842112317728, 0.8814014469398914198, 0.9119408096685510667, 0.9559704048342755334, 1.000000000000000000 ),
 .UNSPECIFIED. ) 
 GEOMETRIC_REPRESENTATION_ITEM ( )  RATIONAL_B_SPLINE_SURFACE ( (
 ( 1.000000000000000000, 1.000000000000000000, 1.000000000000000000, 1.000000000000000000, 1.000000000000000000, 1.000000000000000000, 1.000000000000000000, 1.000000000000000000, 1.000000000000000000, 1.000000000000000000, 1.000000000000000000, 1.000000000000000000, 1.000000000000000000, 1.000000000000000000, 1.000000000000000000, 1.000000000000000000, 1.000000000000000000, 1.000000000000000000, 1.000000000000000000, 1.000000000000000000, 1.000000000000000000, 1.000000000000000000, 1.000000000000000000, 1.000000000000000000, 1.000000000000000000, 1.000000000000000000, 1.000000000000000000, 1.000000000000000000, 1.000000000000000000, 1.000000000000000000),
 ( 0.3333333333333333703, 0.3333333333333333703, 0.3333333333333333703, 0.3333333333333333703, 0.3333333333333333703, 0.3333333333333333703, 0.3333333333333333703, 0.3333333333333333703, 0.3333333333333333703, 0.3333333333333333703, 0.3333333333333333703, 0.3333333333333333703, 0.3333333333333333703, 0.3333333333333333703, 0.3333333333333333703, 0.3333333333333333703, 0.3333333333333333703, 0.3333333333333333703, 0.3333333333333333703, 0.3333333333333333703, 0.3333333333333333703, 0.3333333333333333703, 0.3333333333333333703, 0.3333333333333333703, 0.3333333333333333703, 0.3333333333333333703, 0.3333333333333333703, 0.3333333333333333703, 0.3333333333333333703, 0.3333333333333333703),
 ( 0.3333333333333333703, 0.3333333333333333703, 0.3333333333333333703, 0.3333333333333333703, 0.3333333333333333703, 0.3333333333333333703, 0.3333333333333333703, 0.3333333333333333703, 0.3333333333333333703, 0.3333333333333333703, 0.3333333333333333703, 0.3333333333333333703, 0.3333333333333333703, 0.3333333333333333703, 0.3333333333333333703, 0.3333333333333333703, 0.3333333333333333703, 0.3333333333333333703, 0.3333333333333333703, 0.3333333333333333703, 0.3333333333333333703, 0.3333333333333333703, 0.3333333333333333703, 0.3333333333333333703, 0.3333333333333333703, 0.3333333333333333703, 0.3333333333333333703, 0.3333333333333333703, 0.3333333333333333703, 0.3333333333333333703),
 ( 1.000000000000000000, 1.000000000000000000, 1.000000000000000000, 1.000000000000000000, 1.000000000000000000, 1.000000000000000000, 1.000000000000000000, 1.000000000000000000, 1.000000000000000000, 1.000000000000000000, 1.000000000000000000, 1.000000000000000000, 1.000000000000000000, 1.000000000000000000, 1.000000000000000000, 1.000000000000000000, 1.000000000000000000, 1.000000000000000000, 1.000000000000000000, 1.000000000000000000, 1.000000000000000000, 1.000000000000000000, 1.000000000000000000, 1.000000000000000000, 1.000000000000000000, 1.000000000000000000, 1.000000000000000000, 1.000000000000000000, 1.000000000000000000, 1.000000000000000000),
 ( 0.3333333333333333703, 0.3333333333333333703, 0.3333333333333333703, 0.3333333333333333703, 0.3333333333333333703, 0.3333333333333333703, 0.3333333333333333703, 0.3333333333333333703, 0.3333333333333333703, 0.3333333333333333703, 0.3333333333333333703, 0.3333333333333333703, 0.3333333333333333703, 0.3333333333333333703, 0.3333333333333333703, 0.3333333333333333703, 0.3333333333333333703, 0.3333333333333333703, 0.3333333333333333703, 0.3333333333333333703, 0.3333333333333333703, 0.3333333333333333703, 0.3333333333333333703, 0.3333333333333333703, 0.3333333333333333703, 0.3333333333333333703, 0.3333333333333333703, 0.3333333333333333703, 0.3333333333333333703, 0.3333333333333333703),
 ( 0.3333333333333333703, 0.3333333333333333703, 0.3333333333333333703, 0.3333333333333333703, 0.3333333333333333703, 0.3333333333333333703, 0.3333333333333333703, 0.3333333333333333703, 0.3333333333333333703, 0.3333333333333333703, 0.3333333333333333703, 0.3333333333333333703, 0.3333333333333333703, 0.3333333333333333703, 0.3333333333333333703, 0.3333333333333333703, 0.3333333333333333703, 0.3333333333333333703, 0.3333333333333333703, 0.3333333333333333703, 0.3333333333333333703, 0.3333333333333333703, 0.3333333333333333703, 0.3333333333333333703, 0.3333333333333333703, 0.3333333333333333703, 0.3333333333333333703, 0.3333333333333333703, 0.3333333333333333703, 0.3333333333333333703),
 ( 1.000000000000000000, 1.000000000000000000, 1.000000000000000000, 1.000000000000000000, 1.000000000000000000, 1.000000000000000000, 1.000000000000000000, 1.000000000000000000, 1.000000000000000000, 1.000000000000000000, 1.000000000000000000, 1.000000000000000000, 1.000000000000000000, 1.000000000000000000, 1.000000000000000000, 1.000000000000000000, 1.000000000000000000, 1.000000000000000000, 1.000000000000000000, 1.000000000000000000, 1.000000000000000000, 1.000000000000000000, 1.000000000000000000, 1.000000000000000000, 1.000000000000000000, 1.000000000000000000, 1.000000000000000000, 1.000000000000000000, 1.000000000000000000, 1.000000000000000000) ) ) 
 REPRESENTATION_ITEM ( '' )  SURFACE ( )  );
#9445 = CARTESIAN_POINT ( 'NONE',  ( 199.9999999999999432, -7.567711247534615993, 17.44155761536767812 ) ) ;
#9446 = PLANE ( 'NONE',  #25585 ) ;
#9447 = CARTESIAN_POINT ( 'NONE',  ( 146.6084372240433709, 32.08495691632064961, -24.48358557860320417 ) ) ;
#9448 = CARTESIAN_POINT ( 'NONE',  ( -100.7734535825088358, 6.065416334915073333E-14, -22.67402823373191723 ) ) ;
#9449 = CARTESIAN_POINT ( 'NONE',  ( -105.2054292635176580, -14.22820505692067528, -16.16779137048389003 ) ) ;
#9450 = CARTESIAN_POINT ( 'NONE',  ( 160.9163046357249129, -205.7889608577475542, -55.61140153332243585 ) ) ;
#9451 = CARTESIAN_POINT ( 'NONE',  ( -280.0000000000000000, 1.839446121267387017E-14, -20.00000000000001421 ) ) ;
#9452 = CARTESIAN_POINT ( 'NONE',  ( 19.06497207195981858, -39.99999999999987210, -14.19242893257882621 ) ) ;
#9453 = CARTESIAN_POINT ( 'NONE',  ( -238.4067589809705794, -39.99999999999963762, -40.96449428006383187 ) ) ;
#9454 = CARTESIAN_POINT ( 'NONE',  ( -105.2833435977022987, -11.73665196258528987, 17.94452063502825467 ) ) ;
#9455 = CARTESIAN_POINT ( 'NONE',  ( 19.06497207195981858, -38.31983398719616218, -18.24870850772777331 ) ) ;
#9456 = CARTESIAN_POINT ( 'NONE',  ( -100.7734535825088358, 6.065416334915073333E-14, -22.67402823373191723 ) ) ;
#9457 = CARTESIAN_POINT ( 'NONE',  ( -105.3755690713226727, 15.38646221621793231, -15.38646221621779020 ) ) ;
#9458 = CARTESIAN_POINT ( 'NONE',  ( 156.1979191798867532, 27.38417834433174036, 11.34289806466604134 ) ) ;
#9459 = CARTESIAN_POINT ( 'NONE',  ( -77.58523997990521082, 17.50224656894025088, -13.57278374163336920 ) ) ;
#9460 = CARTESIAN_POINT ( 'NONE',  ( -238.4067589809705794, -0.6820004457913680929, 0.6820004457913170226 ) ) ;
#9461 = CARTESIAN_POINT ( 'NONE',  ( 184.8905102610680444, 1.070102760522089011E-13, -20.92133201514444352 ) ) ;
#9462 = CARTESIAN_POINT ( 'NONE',  ( 163.1118516004056573, -47.56205970284957374, 9.006482792074162802 ) ) ;
#9463 = CARTESIAN_POINT ( 'NONE',  ( -30.26275506840322649, -29.48230279907769358, -29.48230279907820162 ) ) ;
#9464 = CARTESIAN_POINT ( 'NONE',  ( -642.7011836544691050, 32.34672097386517464, -31.29233336928180620 ) ) ;
#9465 = CARTESIAN_POINT ( 'NONE',  ( 3.854700064722247799, 24.62824689552012103, 44.60002223906890606 ) ) ;
#9466 = ORIENTED_EDGE ( 'NONE', *, *, #26065, .F. ) ;
#9467 = CARTESIAN_POINT ( 'NONE',  ( 170.2234770963711128, 10.92277846919216522, -10.92277846919186501 ) ) ;
#9468 = DIRECTION ( 'NONE',  ( 1.000000000000000000, 1.303213150798907793E-16, 2.465190328815661892E-32 ) ) ;
#9469 = EDGE_CURVE ( 'NONE', #4824, #6965, #5758, .T. ) ;
#9470 = CARTESIAN_POINT ( 'NONE',  ( -612.2488540682973053, 31.87925413264133923, 31.76643078590619851 ) ) ;
#9471 = ORIENTED_EDGE ( 'NONE', *, *, #10438, .T. ) ;
#9472 = CARTESIAN_POINT ( 'NONE',  ( 199.9999999999998863, 13.43021917686961331, -13.43983678748323918 ) ) ;
#9473 = CARTESIAN_POINT ( 'NONE',  ( 199.0263771574038856, -15.03208543695887300, 13.25939591991213717 ) ) ;
#9474 = EDGE_CURVE ( 'NONE', #15543, #18337, #18823, .T. ) ;
#9475 = CARTESIAN_POINT ( 'NONE',  ( -47.65341557541689355, 14.80716566684846569, 29.74088027406873280 ) ) ;
#9476 = ORIENTED_EDGE ( 'NONE', *, *, #4206, .F. ) ;
#9477 = ORIENTED_EDGE ( 'NONE', *, *, #24685, .T. ) ;
#9478 = CARTESIAN_POINT ( 'NONE',  ( 4.995406935893293543, -10.78321810389005364, 10.78321810388994173 ) ) ;
#9479 = CARTESIAN_POINT ( 'NONE',  ( -192.9588430854690273, 39.99999999999992895, 14.46834944099983922 ) ) ;
#9480 = EDGE_CURVE ( 'NONE', #8002, #21682, #19361, .T. ) ;
#9481 = EDGE_CURVE ( 'NONE', #15971, #23760, #25962, .T. ) ;
#9482 = CARTESIAN_POINT ( 'NONE',  ( -86.86578273022543328, -19.68494377654098670, -8.153770686795214218 ) ) ;
#9483 = CARTESIAN_POINT ( 'NONE',  ( -162.0762913951020892, 29.48230308784799902, -29.48230308784730980 ) ) ;
#9484 = CARTESIAN_POINT ( 'NONE',  ( -30.26275506840323359, -1.535832457777009877E-13, 41.69427246844629309 ) ) ;
#9485 = CARTESIAN_POINT ( 'NONE',  ( 200.0000000000001137, -18.99355687379454949, 0.7833857536329088544 ) ) ;
#9486 = CARTESIAN_POINT ( 'NONE',  ( 163.1118516004056573, 40.00000000000000711, 12.73709011382489642 ) ) ;
#9487 = FACE_OUTER_BOUND ( 'NONE', #11308, .T. ) ;
#9488 = CARTESIAN_POINT ( 'NONE',  ( -5.152948516943237856, -23.23217004668927643, -42.67688069069051693 ) ) ;
#9489 = CARTESIAN_POINT ( 'NONE',  ( -259.2033419157646676, 35.01439189186559275, -21.55415060305807984 ) ) ;
#9490 = CARTESIAN_POINT ( 'NONE',  ( -4.039451493210478361, -43.00522595893993838, -23.44932283416681429 ) ) ;
#9491 = CARTESIAN_POINT ( 'NONE',  ( -198.0356074513804572, 1.247057299367198800E-13, -15.37879056873070560 ) ) ;
#9492 = CARTESIAN_POINT ( 'NONE',  ( -370.0000000000001137, -4.857225732735059864E-14, -19.53474504356807273 ) ) ;
#9493 = CARTESIAN_POINT ( 'NONE',  ( -238.4067589809705794, -0.9644942799826263791, 40.00000000000002132 ) ) ;
#9494 = CARTESIAN_POINT ( 'NONE',  ( -198.0356074513804572, -55.37879056871328487, -40.00000000000002132 ) ) ;
#9495 = CARTESIAN_POINT ( 'NONE',  ( -192.9588430854689989, -10.23066800230756890, 10.23066800230742501 ) ) ;
#9496 = CARTESIAN_POINT ( 'NONE',  ( -213.1075012329537230, -13.71589010951915810, -40.00000000000002132 ) ) ;
#9498 = CARTESIAN_POINT ( 'NONE',  ( -80.82924211444361617, 19.36828989313945826, 8.022608353712277207 ) ) ;
#9497 = CARTESIAN_POINT ( 'NONE',  ( 22.26816181513975224, -43.18156009806480000, -23.58015273002475354 ) ) ;
#9499 = PLANE ( 'NONE',  #14701 ) ;
#9500 = CARTESIAN_POINT ( 'NONE',  ( 19.06497207195981147, 38.31983398719620482, 38.31983398719633271 ) ) ;
#9501 = CARTESIAN_POINT ( 'NONE',  ( 151.7948205124836534, 6.767089262349056611, 40.00000000000002132 ) ) ;
#9502 = VERTEX_POINT ( 'NONE', #6971 ) ;
#9503 = CARTESIAN_POINT ( 'NONE',  ( 67.79414719533728828, -30.31905270963927279, 10.30785037361772005 ) ) ;
#9504 = VECTOR ( 'NONE', #9030, 1000.000000000000114 ) ;
#9505 = CARTESIAN_POINT ( 'NONE',  ( 190.0000000000000000, 66.50000000000009948, -66.50000000000005684 ) ) ;
#9506 = CARTESIAN_POINT ( 'NONE',  ( 200.0000000000000000, -42.42640687119293119, 14.14213562373082134 ) ) ;
#9507 = CARTESIAN_POINT ( 'NONE',  ( -192.9588430854689989, -8.596193650988133061E-14, 14.46834944099969533 ) ) ;
#9508 = CARTESIAN_POINT ( 'NONE',  ( -213.1075012329537230, 9.698598906450543566, -9.698598906450348167 ) ) ;
#9509 = CARTESIAN_POINT ( 'NONE',  ( -198.0356074513804572, 15.37879056873066830, -40.00000000000002132 ) ) ;
#9510 = DIRECTION ( 'NONE',  ( -1.000000000000000000, 0.000000000000000000, 0.000000000000000000 ) ) ;
#9511 = CARTESIAN_POINT ( 'NONE',  ( 199.9999999999998863, 6.967860089407453827, 17.68684069956508154 ) ) ;
#9512 = CARTESIAN_POINT ( 'NONE',  ( -82.24297220888483650, -2.527436275905056817, -20.07419058344045126 ) ) ;
#9513 = CARTESIAN_POINT ( 'NONE',  ( -91.56559293963834989, 12.25131212657428748, 44.31723036834913643 ) ) ;
#9514 = CARTESIAN_POINT ( 'NONE',  ( 4.995406935893300648, -10.78321810387790514, -67.35176059880241439 ) ) ;
#9515 = CARTESIAN_POINT ( 'NONE',  ( -199.9999999999999147, -14.17215463606695280, 49.28189405767609088 ) ) ;
#9516 = CARTESIAN_POINT ( 'NONE',  ( -105.2054292635175585, -15.19799821370250825, 15.19799821370211923 ) ) ;
#9517 = CARTESIAN_POINT ( 'NONE',  ( -259.2033419157646676, 6.730120644403918995, -49.83842185052024831 ) ) ;
#9519 = CARTESIAN_POINT ( 'NONE',  ( 146.6084372240433709, -52.76785682606510619, -3.800685668859292043 ) ) ;
#9518 = CARTESIAN_POINT ( 'NONE',  ( 170.2234770963711128, 45.64576402573196390, -10.92277846919159856 ) ) ;
#9520 = CARTESIAN_POINT ( 'NONE',  ( -100.7734535825088358, -16.03295912088728770, 16.03295912088687913 ) ) ;
#9521 = CARTESIAN_POINT ( 'NONE',  ( -726.9846540392142060, 52.50000000000007816, -52.49999999999999289 ) ) ;
#9522 = DIRECTION ( 'NONE',  ( 0.000000000000000000, -1.000000000000000000, 0.000000000000000000 ) ) ;
#9523 = CARTESIAN_POINT ( 'NONE',  ( 200.0000000000000000, -39.99999999999991473, -20.00000000000024514 ) ) ;
#9524 = CARTESIAN_POINT ( 'NONE',  ( -198.0356074513804572, 10.87444709759730088, -10.87444709759707173 ) ) ;
#9525 = CARTESIAN_POINT ( 'NONE',  ( -30.26275506840324425, 1.694272468446254232, 40.00000000000002132 ) ) ;
#9526 = ORIENTED_EDGE ( 'NONE', *, *, #4443, .F. ) ;
#9527 = CARTESIAN_POINT ( 'NONE',  ( 200.0000000000000000, 14.14213562373100608, -42.42640687119291698 ) ) ;
#9528 = CARTESIAN_POINT ( 'NONE',  ( -1.776459010276445705, 42.72191398789923511, 17.69599618432451393 ) ) ;
#9529 = CARTESIAN_POINT ( 'NONE',  ( 44.82887508594575365, 18.94256811214892977, 36.15717056695527276 ) ) ;
#9530 = CARTESIAN_POINT ( 'NONE',  ( -105.4288953903209318, -7.317865678924526662, 20.05883966466176815 ) ) ;
#9531 = VERTEX_POINT ( 'NONE', #4601 ) ;
#9532 = LINE ( 'NONE', #9670, #9643 ) ;
#9533 = CARTESIAN_POINT ( 'NONE',  ( 199.9999999999999147, -14.49496992596536771, -12.29673964441684042 ) ) ;
#9534 = EDGE_CURVE ( 'NONE', #6406, #25369, #6883, .T. ) ;
#9535 = CARTESIAN_POINT ( 'NONE',  ( 23.48902902575320795, -13.79248457098053215, 46.76665409567269194 ) ) ;
#9536 = CARTESIAN_POINT ( 'NONE',  ( 16.03312633937180109, 18.43342098166968768, -44.50221493478129986 ) ) ;
#9537 = CARTESIAN_POINT ( 'NONE',  ( 199.0054956575951621, 16.44889389956343706, -11.36889162147346255 ) ) ;
#9538 =( BOUNDED_CURVE ( )  B_SPLINE_CURVE ( 3, ( #628, #6469, #6597, #20581, #14583, #4489, #2355 ),
 .UNSPECIFIED., .F., .F. ) 
 B_SPLINE_CURVE_WITH_KNOTS ( ( 4, 3, 4 ),
 ( 0.007485919821752121811, 0.02392635744100474887, 0.04567102422631708070 ),
 .UNSPECIFIED. ) 
 CURVE ( )  GEOMETRIC_REPRESENTATION_ITEM ( )  RATIONAL_B_SPLINE_CURVE ( ( 0.5852718452494397594, 0.6660804010233953854, 0.8043231192735821322, 1.000000000000000000, 0.7411912828888134186, 0.5828554938567341859, 0.5249926329037621908 ) ) 
 REPRESENTATION_ITEM ( '' )  );
#9539 = UNCERTAINTY_MEASURE_WITH_UNIT (LENGTH_MEASURE( 1.000000000000000082E-05 ), #1206, 'distance_accuracy_value', 'NONE');
#9540 = CARTESIAN_POINT ( 'NONE',  ( -77.58504658346102190, -2.778652059942609664, 21.97438119294674763 ) ) ;
#9541 = CARTESIAN_POINT ( 'NONE',  ( -208.1127848780265026, -9.061048840815752106E-14, 15.00245453012669472 ) ) ;
#9542 = CARTESIAN_POINT ( 'NONE',  ( 199.9999999999999432, 1.065690307512836407E-13, -20.00000000000010303 ) ) ;
#9543 = DIRECTION ( 'NONE',  ( 0.000000000000000000, -1.000000000000000000, 0.000000000000000000 ) ) ;
#9544 = CARTESIAN_POINT ( 'NONE',  ( 57.59792236341148453, -37.56421063658185489, 40.00000000000002132 ) ) ;
#9546 = DIRECTION ( 'NONE',  ( 1.000000000000000000, 1.836970198721030427E-16, -0.000000000000000000 ) ) ;
#9545 = CARTESIAN_POINT ( 'NONE',  ( 98.29820294267327085, -7.653668647303853767, -18.47759065023127434 ) ) ;
#9547 = CARTESIAN_POINT ( 'NONE',  ( 57.59792236341148453, -37.56421063658185489, 40.00000000000002132 ) ) ;
#9548 = CARTESIAN_POINT ( 'NONE',  ( -100.7734535825088500, 22.67402823373189946, -40.00000000000002132 ) ) ;
#9549 = CARTESIAN_POINT ( 'NONE',  ( -259.2033419157646676, -9.517827891722680178, 40.00000000000002132 ) ) ;
#9550 = CARTESIAN_POINT ( 'NONE',  ( 14.38125909742181818, 5.830552384690105017E-13, -55.17850393972636880 ) ) ;
#9551 = CARTESIAN_POINT ( 'NONE',  ( -213.1075012329537230, 1.045191102001431893E-13, -13.71589010951911902 ) ) ;
#9552 = CARTESIAN_POINT ( 'NONE',  ( 4.995406935893293543, -10.78321810388990265, -10.78321810389009272 ) ) ;
#9553 = EDGE_CURVE ( 'NONE', #7462, #10069, #26181, .T. ) ;
#9554 = VERTEX_POINT ( 'NONE', #870 ) ;
#9555 = CARTESIAN_POINT ( 'NONE',  ( -87.13361725327072804, 21.49321519333428299, -1.365653317446499981 ) ) ;
#9556 = CARTESIAN_POINT ( 'NONE',  ( 0.2972598230769938343, 10.13633138497472252, 10.13633138497475628 ) ) ;
#9557 = SURFACE_STYLE_USAGE ( .BOTH. , #3322 ) ;
#9558 = CARTESIAN_POINT ( 'NONE',  ( -190.6721449140022173, 47.76494005424142841, -13.94344083317845850 ) ) ;
#9559 =( GEOMETRIC_REPRESENTATION_CONTEXT ( 3 ) GLOBAL_UNCERTAINTY_ASSIGNED_CONTEXT ( ( #17337 ) ) GLOBAL_UNIT_ASSIGNED_CONTEXT ( ( #12387, #15836, #1895 ) ) REPRESENTATION_CONTEXT ( 'NONE', 'WORKASPACE' ) );
#9560 = ORIENTED_EDGE ( 'NONE', *, *, #18585, .F. ) ;
#9561 = VERTEX_POINT ( 'NONE', #5124 ) ;
#9562 = CARTESIAN_POINT ( 'NONE',  ( -93.02511667906881598, 8.946512270084880925, -20.50052124204823656 ) ) ;
#9563 = DIRECTION ( 'NONE',  ( -1.000000000000000000, -1.836970198721030181E-16, -0.000000000000000000 ) ) ;
#9564 = ORIENTED_EDGE ( 'NONE', *, *, #23937, .F. ) ;
#9565 = CARTESIAN_POINT ( 'NONE',  ( -103.9663809735407369, -19.92521373251424777, 8.574562935515732676 ) ) ;
#9566 = VERTEX_POINT ( 'NONE', #6572 ) ;
#9567 = B_SPLINE_CURVE_WITH_KNOTS ( 'NONE', 3,
 ( #12911, #22505, #14372, #2810, #8916, #547 ),
 .UNSPECIFIED., .F., .F.,
 ( 4, 2, 4 ),
 ( -6.000000005839790033E-08, 0.03937727647058165970, 0.07875461294116338495 ),
 .UNSPECIFIED. ) ;
#9568 = CARTESIAN_POINT ( 'NONE',  ( 200.0000000000001990, -4.022463818607304731, 18.57981244883409744 ) ) ;
#9569 = CIRCLE ( 'NONE', #10862, 15.00000000000000000 ) ;
#9570 = AXIS2_PLACEMENT_3D ( 'NONE', #18264, #16802, #24669 ) ;
#9571 = CARTESIAN_POINT ( 'NONE',  ( -189.4799703873390797, 13.88847319136869096, 47.39666448643363594 ) ) ;
#9572 = CARTESIAN_POINT ( 'NONE',  ( 184.8905102610680444, 41.77492675556005253, -14.79361573936377461 ) ) ;
#9573 = DIRECTION ( 'NONE',  ( 0.000000000000000000, -1.000000000000000000, 0.000000000000000000 ) ) ;
#9574 = CARTESIAN_POINT ( 'NONE',  ( 136.1360204305621266, 1.473277640373554421E-13, -35.03383547441296741 ) ) ;
#9575 = CARTESIAN_POINT ( 'NONE',  ( -188.5332406156854006, -23.50029615566145580, 43.07394490461352632 ) ) ;
#9576 = DIRECTION ( 'NONE',  ( 1.000000000000000000, -1.836970198721030181E-16, -0.000000000000000000 ) ) ;
#9577 = CIRCLE ( 'NONE', #24468, 4.999999999999997335 ) ;
#9578 = AXIS2_PLACEMENT_3D ( 'NONE', #20131, #8012, #23847 ) ;
#9579 = CARTESIAN_POINT ( 'NONE',  ( -190.0000000000000000, -61.50000000000001421, -66.50000000000005684 ) ) ;
#9580 = DIRECTION ( 'NONE',  ( 0.000000000000000000, 1.000000000000000000, 0.000000000000000000 ) ) ;
#9581 = CARTESIAN_POINT ( 'NONE',  ( -184.9730489281052144, -45.83721239348559351, -13.59277546673601833 ) ) ;
#9582 = CARTESIAN_POINT ( 'NONE',  ( -30.26275506840323359, -39.99999999999959499, -41.69427246844670520 ) ) ;
#9583 = CARTESIAN_POINT ( 'NONE',  ( -105.2502192157150063, -17.39781795296958222, 12.58588914170264594 ) ) ;
#9584 = CARTESIAN_POINT ( 'NONE',  ( -280.0000000000000568, -14.14213562373078226, -42.42640687119295251 ) ) ;
#9585 = CARTESIAN_POINT ( 'NONE',  ( -86.96347745069644475, 5.999880687339585546E-14, -21.75974354311649961 ) ) ;
#9586 = CARTESIAN_POINT ( 'NONE',  ( 170.2234770963711128, -39.20704971665379190, -17.36149277827012938 ) ) ;
#9587 = LINE ( 'NONE', #13573, #11699 ) ;
#9588 = CARTESIAN_POINT ( 'NONE',  ( -77.70077460412309733, 11.21025402036413965, -18.98542998413455507 ) ) ;
#9589 = DIRECTION ( 'NONE',  ( 0.000000000000000000, 0.000000000000000000, 1.000000000000000000 ) ) ;
#9590 = CARTESIAN_POINT ( 'NONE',  ( -105.3755690713226585, -39.99999999999996447, -21.75974354311664527 ) ) ;
#9591 = CARTESIAN_POINT ( 'NONE',  ( -238.4067589809705794, 28.96627169325315165, 28.96627169325329731 ) ) ;
#9592 = VECTOR ( 'NONE', #17529, 1000.000000000000000 ) ;
#9593 = CARTESIAN_POINT ( 'NONE',  ( -56.48582580120558561, -50.09629031063971638, 6.472252184283745713 ) ) ;
#9594 = CARTESIAN_POINT ( 'NONE',  ( -129.2920262389484662, -10.46331600572290199, -25.26067940852896854 ) ) ;
#9595 = CARTESIAN_POINT ( 'NONE',  ( 170.2234770963711128, 17.36149277827004411, -17.36149277826983095 ) ) ;
#9596 = ORIENTED_EDGE ( 'NONE', *, *, #1640, .T. ) ;
#9597 = CARTESIAN_POINT ( 'NONE',  ( 14.38125909742181108, 39.01709431150961649, -39.01709431150867147 ) ) ;
#9598 = CARTESIAN_POINT ( 'NONE',  ( -190.0000000000000000, -66.50000000000001421, -66.50000000000005684 ) ) ;
#9599 =( BOUNDED_SURFACE ( )  B_SPLINE_SURFACE ( 3, 2, ( 
 ( #1501, #7344, #15456 ),
 ( #23583, #5360, #21588 ),
 ( #3359, #11461, #19585 ),
 ( #9475, #17581, #25717 ),
 ( #7469, #21715, #7598 ),
 ( #9606, #17711, #15710 ),
 ( #3620, #1633, #4033 ),
 ( #18112, #12133, #9872 ),
 ( #161, #17975, #10005 ),
 ( #22122, #24382, #22395 ),
 ( #26263, #15841, #6147 ),
 ( #15982, #5883, #23970 ),
 ( #8000, #14128, #16117 ),
 ( #24247, #19982, #21848 ),
 ( #6020, #16386, #18382 ),
 ( #3757, #11730, #12000 ),
 ( #5746, #19848, #9741 ),
 ( #17842, #16254, #8265 ),
 ( #22257, #25991, #26121 ),
 ( #20255, #11862, #7863 ),
 ( #1765, #2036, #7729 ),
 ( #13852, #21987, #27 ),
 ( #20122, #8138, #24111 ),
 ( #10138, #4171, #20390 ),
 ( #18242, #5617, #14257 ),
 ( #3901, #13723, #1900 ),
 ( #12265, #2164, #13990 ),
 ( #10274, #16520, #2289 ),
 ( #12519, #2556, #20786 ),
 ( #16652, #16779, #10672 ),
 ( #23395, #10398, #20649 ),
 ( #22651, #19393, #15266 ),
 ( #13275, #18646, #6667 ),
 ( #10533, #3170, #11273 ),
 ( #8670, #1047, #6277 ),
 ( #5171, #2700, #431 ),
 ( #12659, #14645, #17264 ),
 ( #24647, #18783, #8398 ),
 ( #6404, #14520, #12393 ),
 ( #19265, #21397, #8535 ),
 ( #7150, #4303, #18513 ),
 ( #1178, #24916, #9280 ),
 ( #566, #4426, #14392 ),
 ( #2424, #24782, #20518 ),
 ( #292, #6534, #9149 ),
 ( #22523, #14783, #22784 ),
 ( #4563, #4692, #22913 ),
 ( #12794, #20920, #10805 ),
 ( #25399, #24518, #19513 ),
 ( #25914, #15769, #13916 ),
 ( #19773, #23897, #7787 ),
 ( #5544, #17637, #21646 ),
 ( #23517, #23641, #15392 ),
 ( #5289, #13520, #3295 ),
 ( #5811, #15903, #19911 ),
 ( #25527, #13396, #17388 ),
 ( #9529, #13652, #19645 ),
 ( #11650, #1829, #22051 ),
 ( #7655, #15511, #11926 ),
 ( #17513, #3825, #11520 ),
 ( #5419, #3418, #20051 ),
 ( #1429, #1562, #25780 ) ),
 .UNSPECIFIED., .F., .F., .F. ) 
 B_SPLINE_SURFACE_WITH_KNOTS ( ( 4, 2, 2, 2, 2, 2, 2, 2, 2, 2, 2, 2, 2, 2, 2, 2, 2, 2, 2, 2, 2, 2, 2, 2, 2, 2, 2, 2, 2, 2, 4 ),
 ( 3, 3 ),
 ( 0.005118828937691504918, 0.02956064127318995538, 0.05400245360868840411, 0.07844426594418685283, 0.08149949248612416153, 0.08302710575709282281, 0.08379091239257714652, 0.08417281571031931531, 0.08436376736919039276, 0.08445924319862593843, 0.08450698111334370433, 0.08455471902806147022, 0.09066517211193608761, 0.09677562519581070499, 0.09983085173774799981, 0.1028860782796853085, 0.1089965313635599120, 0.1151069844474345294, 0.1181622109893718381, 0.1196898242603404994, 0.1204536308958248231, 0.1208355342135669919, 0.1208594031709258748, 0.1208832721282847578, 0.1209310100430025237, 0.1210264858724380693, 0.1212174375313091468, 0.1273278906151837642, 0.1517697029506822060, 0.1762115152861806755, 0.2006533276216791173 ),
 ( 0.000000000000000000, 1.000000000000000000 ),
 .UNSPECIFIED. ) 
 GEOMETRIC_REPRESENTATION_ITEM ( )  RATIONAL_B_SPLINE_SURFACE ( (
 ( 1.000000000000000000, 0.9997813423572993186, 1.000000000000000000),
 ( 1.000000000000000000, 0.9990919206322248503, 1.000000000000000000),
 ( 1.000000000000000000, 0.9967874177836960614, 1.000000000000000000),
 ( 1.000000000000000000, 0.9887544623284959533, 1.000000000000000000),
 ( 1.000000000000000000, 0.9830290792194851246, 1.000000000000000000),
 ( 1.000000000000000000, 0.9678345454226107147, 1.000000000000000000),
 ( 1.000000000000000000, 0.9583650305386990365, 1.000000000000000000),
 ( 1.000000000000000000, 0.9453335293273732454, 1.000000000000000000),
 ( 1.000000000000000000, 0.9438523872746359400, 1.000000000000000000),
 ( 1.000000000000000000, 0.9415799504611032100, 1.000000000000000000),
 ( 1.000000000000000000, 0.9408140170424519333, 1.000000000000000000),
 ( 1.000000000000000000, 0.9396523143998815053, 1.000000000000000000),
 ( 1.000000000000000000, 0.9392629463989758953, 1.000000000000000000),
 ( 1.000000000000000000, 0.9386756783045917540, 1.000000000000000000),
 ( 1.000000000000000000, 0.9384793862554625665, 1.000000000000000000),
 ( 1.000000000000000000, 0.9381841422087084936, 1.000000000000000000),
 ( 1.000000000000000000, 0.9380855931974712014, 1.000000000000000000),
 ( 1.000000000000000000, 0.9379375679425669965, 1.000000000000000000),
 ( 1.000000000000000000, 0.9378881925679130038, 1.000000000000000000),
 ( 1.000000000000000000, 0.9378140790407697436, 1.000000000000000000),
 ( 1.000000000000000000, 0.9377896949153108341, 1.000000000000000000),
 ( 1.000000000000000000, 0.9377409313169025040, 1.000000000000000000),
 ( 1.000000000000000000, 0.9377165729686793849, 1.000000000000000000),
 ( 1.000000000000000000, 0.9345773786259878868, 1.000000000000000000),
 ( 1.000000000000000000, 0.9318492984274234781, 1.000000000000000000),
 ( 1.000000000000000000, 0.9273872927429863688, 1.000000000000000000),
 ( 1.000000000000000000, 0.9256532593472229786, 1.000000000000000000),
 ( 1.000000000000000000, 0.9239357372750044428, 1.000000000000000000),
 ( 1.000000000000000000, 0.9235102113427005044, 1.000000000000000000),
 ( 1.000000000000000000, 0.9229728558029806074, 1.000000000000000000),
 ( 1.000000000000000000, 0.9228633126626633043, 1.000000000000000000),
 ( 1.000000000000000000, 0.9230139704736608497, 1.000000000000000000),
 ( 1.000000000000000000, 0.9237531682203802275, 1.000000000000000000),
 ( 1.000000000000000000, 0.9264156051930979574, 1.000000000000000000),
 ( 1.000000000000000000, 0.9283388455998493605, 1.000000000000000000),
 ( 1.000000000000000000, 0.9320050037531917297, 1.000000000000000000),
 ( 1.000000000000000000, 0.9333574575348343449, 1.000000000000000000),
 ( 1.000000000000000000, 0.9355411998009124375, 1.000000000000000000),
 ( 1.000000000000000000, 0.9362956009276801606, 1.000000000000000000),
 ( 1.000000000000000000, 0.9374637148015854127, 1.000000000000000000),
 ( 1.000000000000000000, 0.9378591705545192836, 1.000000000000000000),
 ( 1.000000000000000000, 0.9384610703419627997, 1.000000000000000000),
 ( 1.000000000000000000, 0.9386631562400347129, 1.000000000000000000),
 ( 1.000000000000000000, 0.9388793792114333847, 1.000000000000000000),
 ( 1.000000000000000000, 0.9388921037490437493, 1.000000000000000000),
 ( 1.000000000000000000, 0.9389175638858636708, 1.000000000000000000),
 ( 1.000000000000000000, 0.9389305010154682662, 1.000000000000000000),
 ( 1.000000000000000000, 0.9389691441647997072, 1.000000000000000000),
 ( 1.000000000000000000, 0.9389948969011567836, 1.000000000000000000),
 ( 1.000000000000000000, 0.9390721270299990930, 1.000000000000000000),
 ( 1.000000000000000000, 0.9391235763422390859, 1.000000000000000000),
 ( 1.000000000000000000, 0.9392778120326412683, 1.000000000000000000),
 ( 1.000000000000000000, 0.9393804861645803639, 1.000000000000000000),
 ( 1.000000000000000000, 0.9427638002345590795, 1.000000000000000000),
 ( 1.000000000000000000, 0.9458915987235437806, 1.000000000000000000),
 ( 1.000000000000000000, 0.9607963039197253696, 1.000000000000000000),
 ( 1.000000000000000000, 0.9703812854704935154, 1.000000000000000000),
 ( 1.000000000000000000, 0.9854660764538308859, 1.000000000000000000),
 ( 1.000000000000000000, 0.9909632567911316192, 1.000000000000000000),
 ( 1.000000000000000000, 0.9982308762617709830, 1.000000000000000000),
 ( 1.000000000000000000, 0.9999976772058264407, 1.000000000000000000),
 ( 1.000000000000000000, 1.000000000000000000, 1.000000000000000000) ) ) 
 REPRESENTATION_ITEM ( '' )  SURFACE ( )  );
#9600 = CARTESIAN_POINT ( 'NONE',  ( -626.3753644243258805, 28.28427124746188426, 34.99999999999999289 ) ) ;
#9601 = CARTESIAN_POINT ( 'NONE',  ( 130.8568914410475088, -24.07718906446864793, -32.49135343045505664 ) ) ;
#9602 = CARTESIAN_POINT ( 'NONE',  ( 98.29820294270304259, -18.47759065022024672, 7.653668647299475047 ) ) ;
#9603 = ORIENTED_EDGE ( 'NONE', *, *, #25512, .T. ) ;
#9604 = CARTESIAN_POINT ( 'NONE',  ( 146.6084372240433993, -3.357462877844280890E-13, 34.62501878078305850 ) ) ;
#9605 = CARTESIAN_POINT ( 'NONE',  ( 0.4311942631275967330, -24.25071831022400559, 44.08816696360413800 ) ) ;
#9606 = CARTESIAN_POINT ( 'NONE',  ( -24.88648382770552203, 19.35593139208421931, 36.77569126514013931 ) ) ;
#9607 = AXIS2_PLACEMENT_3D ( 'NONE', #3209, #5461, #3466 ) ;
#9608 = ORIENTED_EDGE ( 'NONE', *, *, #19074, .F. ) ;
#9609 = ORIENTED_EDGE ( 'NONE', *, *, #23617, .F. ) ;
#9610 = CARTESIAN_POINT ( 'NONE',  ( 170.2234770963711128, 15.44714144992819627, -40.00000000000002132 ) ) ;
#9611 = CARTESIAN_POINT ( 'NONE',  ( -192.1964066538934617, -48.17614796929171916, -14.00508515769209339 ) ) ;
#9612 = CARTESIAN_POINT ( 'NONE',  ( 151.7948205124836250, 1.807796684091926154E-15, 6.767089262349031742 ) ) ;
#9613 = CARTESIAN_POINT ( 'NONE',  ( 85.88526014319977264, 8.769885380239042405, -23.37195137963415092 ) ) ;
#9614 = EDGE_CURVE ( 'NONE', #17336, #25302, #14688, .T. ) ;
#9615 = LINE ( 'NONE', #15848, #11397 ) ;
#9616 = CARTESIAN_POINT ( 'NONE',  ( -238.4067589809705794, -3.369206980223063916E-14, -0.9644942799825824142 ) ) ;
#9617 = CARTESIAN_POINT ( 'NONE',  ( 170.2234770963711128, -39.99999999999991473, -24.55285855007201334 ) ) ;
#9618 = CARTESIAN_POINT ( 'NONE',  ( 199.9999999999999147, -10.43683117453143261, -15.88259547814976180 ) ) ;
#9619 = CARTESIAN_POINT ( 'NONE',  ( 0.2972598230769957217, -4.999556039334937811E-14, 14.33493731733933352 ) ) ;
#9620 = DIRECTION ( 'NONE',  ( 1.000000000000000000, 0.000000000000000000, 0.000000000000000000 ) ) ;
#9621 = CARTESIAN_POINT ( 'NONE',  ( -4.339409867971390611, -17.83714383556709748, -43.06267456182897035 ) ) ;
#9622 = EDGE_CURVE ( 'NONE', #19424, #961, #4338, .T. ) ;
#9623 = CARTESIAN_POINT ( 'NONE',  ( 170.2234770963711128, 17.36149277826980253, 17.36149277827007253 ) ) ;
#9624 = CARTESIAN_POINT ( 'NONE',  ( -210.0000000000000284, 0.000000000000000000, 0.000000000000000000 ) ) ;
#9625 = CARTESIAN_POINT ( 'NONE',  ( 19.06497207195981147, 1.521599808664285085E-13, -14.19242893257840521 ) ) ;
#9626 = DIRECTION ( 'NONE',  ( 1.303213150798907793E-16, -1.000000000000000000, 1.682156097916904081E-16 ) ) ;
#9627 = CARTESIAN_POINT ( 'NONE',  ( 192.4448373802101173, 20.00000000003945644, 40.00000000000002132 ) ) ;
#9628 = CARTESIAN_POINT ( 'NONE',  ( -280.0000000000000000, -20.00000000000006750, -2.449293598294708485E-15 ) ) ;
#9629 = EDGE_CURVE ( 'NONE', #14320, #567, #2996, .T. ) ;
#9630 = EDGE_CURVE ( 'NONE', #12216, #12388, #8156, .T. ) ;
#9631 = CARTESIAN_POINT ( 'NONE',  ( 0.2972598230769923355, 18.14793986248697166, 38.42060263243675422 ) ) ;
#9632 = CARTESIAN_POINT ( 'NONE',  ( -198.0356074513804572, -15.37879056873074290, -40.00000000000002132 ) ) ;
#9633 = DIRECTION ( 'NONE',  ( -0.000000000000000000, -0.000000000000000000, 1.000000000000000000 ) ) ;
#9634 = CARTESIAN_POINT ( 'NONE',  ( 14.38125909742180397, 67.30136555895953165, 10.73282306403583242 ) ) ;
#9635 = CARTESIAN_POINT ( 'NONE',  ( 130.8568914410475372, 5.949712681206715814, 2.449293598294708485E-15 ) ) ;
#9636 = ORIENTED_EDGE ( 'NONE', *, *, #2842, .F. ) ;
#9637 = CARTESIAN_POINT ( 'NONE',  ( 22.80622392652957231, -43.16567765897927700, 17.87980911537442807 ) ) ;
#9638 = CARTESIAN_POINT ( 'NONE',  ( 130.1167162091013836, 12.15076864148425528, 29.33455044752971119 ) ) ;
#9639 = VECTOR ( 'NONE', #4412, 1000.000000000000000 ) ;
#9640 = CARTESIAN_POINT ( 'NONE',  ( 200.0000000000000000, 42.42640687119288856, -14.14213562373094746 ) ) ;
#9641 = CARTESIAN_POINT ( 'NONE',  ( 57.59792236341147742, -1.230234673553095937E-13, 37.56421063658186199 ) ) ;
#9642 = CARTESIAN_POINT ( 'NONE',  ( -105.3755690713226585, 12.89780903124349720, 43.67073346367994446 ) ) ;
#9643 = VECTOR ( 'NONE', #24037, 1000.000000000000000 ) ;
#9644 = CARTESIAN_POINT ( 'NONE',  ( 192.4448373802101173, -20.00000000003938538, -40.00000000000002132 ) ) ;
#9645 = CARTESIAN_POINT ( 'NONE',  ( -109.1264249741459906, -13.72187187124011132, -33.12752917269217079 ) ) ;
#9646 = CARTESIAN_POINT ( 'NONE',  ( 199.9999999999999147, 0.6045081272180472531, 19.00173049909658474 ) ) ;
#9647 = CARTESIAN_POINT ( 'NONE',  ( 200.0000000000000000, -13.88319085540579678, 13.00159729487775451 ) ) ;
#9648 = CARTESIAN_POINT ( 'NONE',  ( -105.3755690713226585, 12.89780903124349720, 43.67073346367994446 ) ) ;
#9649 = CARTESIAN_POINT ( 'NONE',  ( -86.96347745069644475, -12.89780903124395195, -12.89780903124416511 ) ) ;
#9650 = CARTESIAN_POINT ( 'NONE',  ( -77.90255099906769942, -20.29001641120677846, -8.064892378658084837 ) ) ;
#9651 = CARTESIAN_POINT ( 'NONE',  ( -77.84504298474458039, 19.81984129313138965, -9.297284891551433006 ) ) ;
#9652 = CARTESIAN_POINT ( 'NONE',  ( 136.1360204305621266, 53.05693388239320285, -3.511608612530223716 ) ) ;
#9654 = CARTESIAN_POINT ( 'NONE',  ( 170.2234770963711128, -17.36149277826940462, -39.20704971665412586 ) ) ;
#9653 = CARTESIAN_POINT ( 'NONE',  ( -162.0762913951020892, -29.48230308784744125, -29.48230308784792442 ) ) ;
#9655 = CARTESIAN_POINT ( 'NONE',  ( -192.9588430854690273, -18.05360324515400094, -38.51493924976961836 ) ) ;
#9656 = ADVANCED_FACE ( 'NONE', ( #8710, #17342 ), #14692, .T. ) ;
#9657 = CARTESIAN_POINT ( 'NONE',  ( 170.2234770963711128, -24.55285855007183926, 0.000000000000000000 ) ) ;
#9658 = CARTESIAN_POINT ( 'NONE',  ( 116.7964245048409424, 27.98274000340266809, 0.000000000000000000 ) ) ;
#9660 = CARTESIAN_POINT ( 'NONE',  ( 19.06497207195982924, -40.00000000000021316, 54.19242893257830218 ) ) ;
#9659 = CARTESIAN_POINT ( 'NONE',  ( 163.1118516004056573, 9.006482792073693844, 47.56205970284970164 ) ) ;
#9661 = CARTESIAN_POINT ( 'NONE',  ( 192.4448373802100889, -14.14213562370313682, 14.14213562370301958 ) ) ;
#9662 = CARTESIAN_POINT ( 'NONE',  ( 146.6084372240433993, 24.48358557860307272, 24.48358557860347418 ) ) ;
#9663 = CARTESIAN_POINT ( 'NONE',  ( -259.2033419157646676, 30.48217210827734647, 40.00000000000002132 ) ) ;
#9664 = ORIENTED_EDGE ( 'NONE', *, *, #19395, .F. ) ;
#9665 = CARTESIAN_POINT ( 'NONE',  ( -135.8532207217289738, -6.472252184284190690, -6.472252184284188914 ) ) ;
#9666 = CARTESIAN_POINT ( 'NONE',  ( -4.585253294881784569, 42.10505998758514323, 17.44048689139054176 ) ) ;
#9667 = CARTESIAN_POINT ( 'NONE',  ( -65.65550967526353077, -9.107276986623745074, -24.89650881518310399 ) ) ;
#9668 = CARTESIAN_POINT ( 'NONE',  ( -30.26275506840324070, 1.694272468446254232, 0.000000000000000000 ) ) ;
#9669 = ORIENTED_EDGE ( 'NONE', *, *, #23316, .T. ) ;
#9670 = CARTESIAN_POINT ( 'NONE',  ( -190.0000000000000000, 71.50000000000009948, 66.50000000000005684 ) ) ;
#9671 = CARTESIAN_POINT ( 'NONE',  ( 200.0000000000000284, -14.89458464808834748, 11.81399803044240038 ) ) ;
#9672 = CARTESIAN_POINT ( 'NONE',  ( -3.921555385249984038, -23.47492146734913732, 43.03974577853593075 ) ) ;
#9673 = CARTESIAN_POINT ( 'NONE',  ( 21.45050411888145092, 18.02367319545977153, -43.51299627226218547 ) ) ;
#9674 = CARTESIAN_POINT ( 'NONE',  ( 199.0059208051008852, 8.690306674284110855, -18.00847358856242408 ) ) ;
#9675 = FACE_OUTER_BOUND ( 'NONE', #24373, .T. ) ;
#9676 = CARTESIAN_POINT ( 'NONE',  ( 163.1118516004056573, 40.00000000000000711, 12.73709011382489642 ) ) ;
#9677 = CARTESIAN_POINT ( 'NONE',  ( -82.23726319241515625, -1.261450157158256591, 20.19517362732507593 ) ) ;
#9678 = CARTESIAN_POINT ( 'NONE',  ( 151.7948205124836250, 4.785054706301759886, -4.785054706301612448 ) ) ;
#9679 = CARTESIAN_POINT ( 'NONE',  ( -238.4067589809705794, -0.9644942799826263791, 40.00000000000002132 ) ) ;
#9681 = CARTESIAN_POINT ( 'NONE',  ( -597.1859489463258797, 39.84828722673089629, -4.032642683987440968 ) ) ;
#9680 = CARTESIAN_POINT ( 'NONE',  ( -187.3037411062156821, 13.75782484034628439, -46.64555264106614629 ) ) ;
#9682 = FACE_OUTER_BOUND ( 'NONE', #19932, .T. ) ;
#9683 = CARTESIAN_POINT ( 'NONE',  ( -105.3755690713226585, 21.75974354311648185, -40.00000000000002132 ) ) ;
#9684 = CARTESIAN_POINT ( 'NONE',  ( -238.4067589809705794, 40.96449427990177128, 40.00000000000002132 ) ) ;
#9685 = CARTESIAN_POINT ( 'NONE',  ( 57.59792236341147742, 4.064940816252731242E-13, -37.56421063658186199 ) ) ;
#9686 = CARTESIAN_POINT ( 'NONE',  ( 160.9163046357249129, -135.7889608577475542, -49.61140153332242875 ) ) ;
#9687 = CARTESIAN_POINT ( 'NONE',  ( -162.0762913951021176, 27.08623940707639477, -29.48230308784743059 ) ) ;
#9688 = ORIENTED_EDGE ( 'NONE', *, *, #20024, .T. ) ;
#9689 = DIRECTION ( 'NONE',  ( -1.000000000000000000, -1.836970198721030181E-16, 0.000000000000000000 ) ) ;
#9690 = CARTESIAN_POINT ( 'NONE',  ( -200.0000000000000000, 66.50000000000009948, -66.50000000000005684 ) ) ;
#9691 = CARTESIAN_POINT ( 'NONE',  ( 91.82158438592158234, -12.16597498397778843, 12.16597498397750954 ) ) ;
#9692 = CARTESIAN_POINT ( 'NONE',  ( -210.0000000000000284, -66.50000000000001421, 66.50000000000005684 ) ) ;
#9693 = VERTEX_POINT ( 'NONE', #25725 ) ;
#9694 = ORIENTED_EDGE ( 'NONE', *, *, #14776, .T. ) ;
#9695 = CARTESIAN_POINT ( 'NONE',  ( -56.48582580120559982, -21.81201906317755501, -34.75652343174621706 ) ) ;
#9696 = CARTESIAN_POINT ( 'NONE',  ( 25.31597067610180929, -42.45761951829256020, -17.58652183052983276 ) ) ;
#9697 = EDGE_LOOP ( 'NONE', ( #19878, #15663, #21048, #17832 ) ) ;
#9698 = CARTESIAN_POINT ( 'NONE',  ( -105.3755690713226585, -21.75974354311652448, -40.00000000000002132 ) ) ;
#9699 = CARTESIAN_POINT ( 'NONE',  ( 190.0000000000000284, -82.49999999999990052, 52.49999999999977973 ) ) ;
#9700 = CIRCLE ( 'NONE', #10148, 5.000000000000011546 ) ;
#9701 = VERTEX_POINT ( 'NONE', #21466 ) ;
#9702 = CARTESIAN_POINT ( 'NONE',  ( 199.9999999999998863, -4.328516665792998097, 18.51095020188552809 ) ) ;
#9703 =( BOUNDED_SURFACE ( )  B_SPLINE_SURFACE ( 3, 2, ( 
 ( #21001, #21139, #25137 ),
 ( #4783, #3039, #19388 ),
 ( #12886, #25395, #17259 ),
 ( #9027, #1042, #9145 ),
 ( #15004, #651, #17131 ),
 ( #2654, #21393, #6758 ),
 ( #1174, #10759, #7146 ),
 ( #20871, #13271, #7014 ),
 ( #14870, #9276, #785 ),
 ( #23265, #10895, #23005 ),
 ( #8890, #15262, #13147 ),
 ( #5166, #8758, #15388 ),
 ( #12750, #3166, #5041 ),
 ( #4908, #23137, #17384 ),
 ( #915, #25523, #11269 ),
 ( #13019, #7271, #18871 ),
 ( #6888, #2914, #19132 ),
 ( #824, #25679, #15295 ),
 ( #25300, #13057, #9434 ),
 ( #13181, #3323, #15418 ),
 ( #25556, #21042, #2824 ),
 ( #25174, #25430, #1330 ),
 ( #23668, #17167, #10934 ),
 ( #7059, #6925, #21549 ),
 ( #21175, #17039, #23423 ),
 ( #2948, #3077, #15174 ),
 ( #11059, #3195, #17541 ),
 ( #19171, #7304, #23545 ),
 ( #17298, #19421, #1207 ),
 ( #19044, #5199, #15042 ),
 ( #7426, #8932, #12925 ),
 ( #23173, #13303, #5315 ),
 ( #21422, #11303, #9310 ),
 ( #23299, #19544, #15540 ) ),
 .UNSPECIFIED., .F., .F., .T. ) 
 B_SPLINE_SURFACE_WITH_KNOTS ( ( 4, 2, 2, 2, 2, 2, 2, 2, 2, 2, 2, 2, 2, 2, 2, 2, 4 ),
 ( 3, 3 ),
 ( 0.005135432767691730169, 0.02907015807668714841, 0.05300488338568256491, 0.07693960869467798835, 0.08292329002192683207, 0.08441921035373904647, 0.08446595786410818207, 0.08448933161929274294, 0.08451270537447730380, 0.08460620039521557501, 0.08479319043669208966, 0.08516717051964514673, 0.08591513068555126087, 0.08890697134917568967, 0.09189881201280011846, 0.09489065267642454726, 0.1008743340036734049 ),
 ( 0.000000000000000000, 1.000000000000000000 ),
 .UNSPECIFIED. ) 
 GEOMETRIC_REPRESENTATION_ITEM ( )  RATIONAL_B_SPLINE_SURFACE ( (
 ( 1.000000000000000000, 0.9997813423552075474, 1.000000000000000000),
 ( 1.000000000000000000, 0.9991063898506410412, 1.000000000000000000),
 ( 1.000000000000000000, 0.9968824705949623777, 1.000000000000000000),
 ( 1.000000000000000000, 0.9891556793369797873, 1.000000000000000000),
 ( 1.000000000000000000, 0.9836552277522164767, 1.000000000000000000),
 ( 1.000000000000000000, 0.9690805015303910475, 1.000000000000000000),
 ( 1.000000000000000000, 0.9600094330325482650, 1.000000000000000000),
 ( 1.000000000000000000, 0.9461485276691540269, 1.000000000000000000),
 ( 1.000000000000000000, 0.9432497373317602074, 1.000000000000000000),
 ( 1.000000000000000000, 0.9394620364518225797, 1.000000000000000000),
 ( 1.000000000000000000, 0.9386962831138920826, 1.000000000000000000),
 ( 1.000000000000000000, 0.9378980481303054173, 1.000000000000000000),
 ( 1.000000000000000000, 0.9378738510928928962, 1.000000000000000000),
 ( 1.000000000000000000, 0.9378375433852950138, 1.000000000000000000),
 ( 1.000000000000000000, 0.9378253334781229134, 1.000000000000000000),
 ( 1.000000000000000000, 0.9378014123365953081, 1.000000000000000000),
 ( 1.000000000000000000, 0.9377894572438933984, 1.000000000000000000),
 ( 1.000000000000000000, 0.9377297092068141993, 1.000000000000000000),
 ( 1.000000000000000000, 0.9376819985415375536, 1.000000000000000000),
 ( 1.000000000000000000, 0.9375391312191778681, 1.000000000000000000),
 ( 1.000000000000000000, 0.9374442392361990173, 1.000000000000000000),
 ( 1.000000000000000000, 0.9371606329892131493, 1.000000000000000000),
 ( 1.000000000000000000, 0.9369729884417210553, 1.000000000000000000),
 ( 1.000000000000000000, 0.9364144211479206170, 1.000000000000000000),
 ( 1.000000000000000000, 0.9360478649889876213, 1.000000000000000000),
 ( 1.000000000000000000, 0.9342453465011781866, 1.000000000000000000),
 ( 1.000000000000000000, 0.9329002455190741339, 1.000000000000000000),
 ( 1.000000000000000000, 0.9304321598238819435, 1.000000000000000000),
 ( 1.000000000000000000, 0.9293115443288706423, 1.000000000000000000),
 ( 1.000000000000000000, 0.9273348408774886309, 1.000000000000000000),
 ( 1.000000000000000000, 0.9264755133099957796, 1.000000000000000000),
 ( 1.000000000000000000, 0.9243017816395038277, 1.000000000000000000),
 ( 1.000000000000000000, 0.9233922826853561139, 1.000000000000000000),
 ( 1.000000000000000000, 0.9230541040372001182, 1.000000000000000000) ) ) 
 REPRESENTATION_ITEM ( '' )  SURFACE ( )  );
#9704 = CARTESIAN_POINT ( 'NONE',  ( -198.0012400611979047, 14.15884001207450460, 49.19397081476446942 ) ) ;
#9705 = CARTESIAN_POINT ( 'NONE',  ( 4.995406935893290878, 39.06748935135185263, 39.06748935135198764 ) ) ;
#9706 = CARTESIAN_POINT ( 'NONE',  ( -105.3841228958018092, -6.698390573547676752, -20.33918053570303641 ) ) ;
#9707 = CARTESIAN_POINT ( 'NONE',  ( 146.6084372240433993, 1.478241399363601114E-13, -34.62501878078305850 ) ) ;
#9708 = CARTESIAN_POINT ( 'NONE',  ( -162.0762913951021176, 1.694272876828294194, 40.00000000000002132 ) ) ;
#9709 = CARTESIAN_POINT ( 'NONE',  ( -198.0356074513804572, 39.15871834505956173, -39.15871834505865223 ) ) ;
#9710 = CARTESIAN_POINT ( 'NONE',  ( -295.0000000000000568, -4.857225732735059864E-14, 9.999999999999996447 ) ) ;
#9711 = EDGE_CURVE ( 'NONE', #17072, #5580, #7736, .T. ) ;
#9712 = CARTESIAN_POINT ( 'NONE',  ( -362.0709805440841365, -4.857225732735059864E-14, 0.000000000000000000 ) ) ;
#9713 = CARTESIAN_POINT ( 'NONE',  ( 0.2972598230769957217, 1.502051041545559470E-13, -14.33493731733933352 ) ) ;
#9714 = CARTESIAN_POINT ( 'NONE',  ( -198.0356074513804572, 1.247057299367198800E-13, -15.37879056873070560 ) ) ;
#9715 = CARTESIAN_POINT ( 'NONE',  ( -200.0000000000000000, -45.34857661735436807, -20.90527768611926263 ) ) ;
#9716 = CARTESIAN_POINT ( 'NONE',  ( 200.0000000000000000, -14.14213562373062949, -42.42640687119301646 ) ) ;
#9717 = CARTESIAN_POINT ( 'NONE',  ( -238.4067589809705794, -40.96449427990185654, -40.00000000000002132 ) ) ;
#9718 = ADVANCED_FACE ( 'NONE', ( #5242 ), #3630, .T. ) ;
#9719 = CARTESIAN_POINT ( 'NONE',  ( -238.4067589809705794, -28.96627169325313389, -27.60227080167074831 ) ) ;
#9720 = FACE_BOUND ( 'NONE', #22871, .T. ) ;
#9721 = VECTOR ( 'NONE', #13108, 1000.000000000000000 ) ;
#9722 = EDGE_CURVE ( 'NONE', #13093, #10307, #9615, .T. ) ;
#9723 = CARTESIAN_POINT ( 'NONE',  ( -77.84460141634585284, 19.81807444411913011, -9.302297467148907373 ) ) ;
#9724 = CARTESIAN_POINT ( 'NONE',  ( 130.8568914410475372, -3.326198072800416995E-13, 34.05028731879788495 ) ) ;
#9725 = CARTESIAN_POINT ( 'NONE',  ( 91.82158438592158234, 7.693928927950222250E-14, -17.20528682183300262 ) ) ;
#9726 = CARTESIAN_POINT ( 'NONE',  ( 200.0000000000000000, -42.42640687119293119, 14.14213562373082134 ) ) ;
#9727 = CARTESIAN_POINT ( 'NONE',  ( -208.1127848780265026, -10.60833733269537227, -10.60833733269551793 ) ) ;
#9728 = CARTESIAN_POINT ( 'NONE',  ( -197.4153392275570411, -14.14666332906662660, -49.11379398047656508 ) ) ;
#9729 = CARTESIAN_POINT ( 'NONE',  ( 14.38125909742181285, -10.73282306404727393, 10.73282306404716380 ) ) ;
#9730 = ORIENTED_EDGE ( 'NONE', *, *, #16772, .F. ) ;
#9731 = CARTESIAN_POINT ( 'NONE',  ( -198.0356074513804572, 10.87444709761036066, -67.44298959253325165 ) ) ;
#9732 = CARTESIAN_POINT ( 'NONE',  ( -91.56559293963836410, 16.03295912088714203, -16.03295912088699282 ) ) ;
#9733 = CARTESIAN_POINT ( 'NONE',  ( -100.7734535825088500, 22.67402823373189946, -40.00000000000002132 ) ) ;
#9734 = CARTESIAN_POINT ( 'NONE',  ( -105.4741150117367283, 19.77569912955882359, -7.943527260733686646 ) ) ;
#9735 = CARTESIAN_POINT ( 'NONE',  ( 14.38125909742181285, -17.55144818341421598, -39.01709431150935359 ) ) ;
#9736 = CARTESIAN_POINT ( 'NONE',  ( -199.9999999999999716, -49.28189405767602693, 14.17215463606940595 ) ) ;
#9737 = ORIENTED_EDGE ( 'NONE', *, *, #10945, .F. ) ;
#9738 = CARTESIAN_POINT ( 'NONE',  ( -30.26275506840324070, -40.00000000000001421, -1.694272468446678559 ) ) ;
#9739 = CARTESIAN_POINT ( 'NONE',  ( 14.33519843538167571, -24.71012982060716823, 44.71104701565639772 ) ) ;
#9740 = B_SPLINE_CURVE_WITH_KNOTS ( 'NONE', 3,
 ( #15353, #17857, #7744, #26008, #3509, #11879, #21862, #15856, #13482, #25734 ),
 .UNSPECIFIED., .F., .F.,
 ( 4, 2, 2, 2, 4 ),
 ( 0.7921542097164070428, 0.8508620842112317728, 0.8814014469398914198, 0.9119408096685510667, 0.9406682828396426554 ),
 .UNSPECIFIED. ) ;
#9741 = CARTESIAN_POINT ( 'NONE',  ( -4.201409602820307398, 13.81669219312490249, 46.93439176590543127 ) ) ;
#9742 = VERTEX_POINT ( 'NONE', #23715 ) ;
#9743 = ORIENTED_EDGE ( 'NONE', *, *, #21185, .F. ) ;
#9744 = PRODUCT_DEFINITION_SHAPE ( 'NONE', 'NONE',  #25182 ) ;
#9745 = CARTESIAN_POINT ( 'NONE',  ( 0.2972598230769930017, 54.33493731733938148, -40.00000000000002132 ) ) ;
#9746 = CARTESIAN_POINT ( 'NONE',  ( -194.4222169613592257, -48.65437996130108900, -14.07715596671970815 ) ) ;
#9747 = CARTESIAN_POINT ( 'NONE',  ( 19.06497207195980792, 39.99999999999983658, 54.19242893257857929 ) ) ;
#9748 = FILL_AREA_STYLE ('',( #19721 ) ) ;
#9749 = CARTESIAN_POINT ( 'NONE',  ( 200.0000000000000000, 7.347880794884121511E-14, 0.000000000000000000 ) ) ;
#9750 = VECTOR ( 'NONE', #11362, 1000.000000000000000 ) ;
#9751 = CARTESIAN_POINT ( 'NONE',  ( 163.1118516004056573, -2.556006622855449647E-13, 27.26290988616872824 ) ) ;
#9752 = DIRECTION ( 'NONE',  ( 0.01051738792036862290, -0.3995761383050656090, -0.9166396752533372272 ) ) ;
#9753 = CARTESIAN_POINT ( 'NONE',  ( -190.6136434985683934, 42.75828627302750107, 17.71106207812097111 ) ) ;
#9754 = CARTESIAN_POINT ( 'NONE',  ( 3.774039766387189854, -18.47898247163652741, -44.61221010187593805 ) ) ;
#9755 = CARTESIAN_POINT ( 'NONE',  ( 146.6084372240433709, -32.08495691632075619, 24.48358557860298035 ) ) ;
#9756 =( BOUNDED_SURFACE ( )  B_SPLINE_SURFACE ( 3, 3, ( 
 ( #20235, #5, #2141, #25969, #3598, #24362, #16095, #20101, #26101, #6000, #22236, #13966, #14106, #18092, #1743, #18361, #3875, #24226, #5860, #10252, #17821, #6126, #14234, #11706, #7709, #15820, #6257, #19959, #140, #9982 ),
 ( #4011, #10118, #21828, #22374, #26242, #11977, #16362, #18219, #8117, #8244, #4150, #23948, #24496, #5725, #7977, #3736, #13829, #21962, #12110, #7838, #2015, #16233, #11839, #15961, #24086, #19827, #9851, #22101, #12244, #20367 ),
 ( #17954, #1613, #9717, #808, #10918, #22890, #12772, #19029, #8512, #20764, #409, #18626, #4540, #8649, #2534, #14624, #16630, #8914, #20899, #6381, #22761, #22630, #2677, #20498, #17023, #12637, #24625, #24891, #25159, #673 ),
 ( #24760, #6646, #14760, #6513, #4670, #10651, #20626, #14370, #18761, #16757, #544, #2807, #10378, #16895, #6780, #4280, #18489, #270, #22502, #12499, #12370, #10783, #8378, #8782, #18894, #25027, #14892, #23032, #4807, #2401 ),
 ( #12909, #2270, #21025, #16500, #14499, #4405, #10512, #1063, #19660, #6910, #13414, #11291, #23157, #19411, #13042, #25543, #23412, #21412, #17530, #9547, #7042, #11410, #1195, #17152, #7414, #15159, #1316, #3185, #23657, #25668 ),
 ( #15528, #5437, #9300, #25286, #23285, #13538, #4932, #17404, #23533, #21664, #17655, #13291, #7294, #21160, #3313, #2934, #15408, #5061, #13167, #5304, #21287, #11043, #3061, #15282, #19280, #21538, #19532, #938, #9169, #11164 ),
 ( #17283, #25416, #7166, #15027, #5189, #9423, #3437, #11536, #1447, #19153, #9047, #24187, #22336, #19926, #5829, #11806, #3701, #15920, #20068, #13931, #26066, #1709, #20331, #5961, #17788, #7804, #7674, #14071, #5563, #4111 ) ),
 .UNSPECIFIED., .T., .F., .F. ) 
 B_SPLINE_SURFACE_WITH_KNOTS ( ( 4, 3, 4 ),
 ( 4, 2, 2, 2, 2, 2, 2, 2, 2, 2, 2, 2, 2, 2, 4 ),
 ( 0.000000000000000000, 0.5000000000000000000, 1.000000000000000000 ),
 ( 0.000000000000000000, 0.1357259735107005372, 0.1651108541090157700, 0.1944957347073310028, 0.3598804999793158710, 0.3867117631979620773, 0.4135430264166082281, 0.5789277916885930964, 0.6062785021374117456, 0.6336292125862302838, 0.8508620842112317728, 0.8814014469398914198, 0.9119408096685510667, 0.9559704048342755334, 1.000000000000000000 ),
 .UNSPECIFIED. ) 
 GEOMETRIC_REPRESENTATION_ITEM ( )  RATIONAL_B_SPLINE_SURFACE ( (
 ( 1.000000000000000000, 1.000000000000000000, 1.000000000000000000, 1.000000000000000000, 1.000000000000000000, 1.000000000000000000, 1.000000000000000000, 1.000000000000000000, 1.000000000000000000, 1.000000000000000000, 1.000000000000000000, 1.000000000000000000, 1.000000000000000000, 1.000000000000000000, 1.000000000000000000, 1.000000000000000000, 1.000000000000000000, 1.000000000000000000, 1.000000000000000000, 1.000000000000000000, 1.000000000000000000, 1.000000000000000000, 1.000000000000000000, 1.000000000000000000, 1.000000000000000000, 1.000000000000000000, 1.000000000000000000, 1.000000000000000000, 1.000000000000000000, 1.000000000000000000),
 ( 0.3333333333333333703, 0.3333333333333333703, 0.3333333333333333703, 0.3333333333333333703, 0.3333333333333333703, 0.3333333333333333703, 0.3333333333333333703, 0.3333333333333333703, 0.3333333333333333703, 0.3333333333333333703, 0.3333333333333333703, 0.3333333333333333703, 0.3333333333333333703, 0.3333333333333333703, 0.3333333333333333703, 0.3333333333333333703, 0.3333333333333333703, 0.3333333333333333703, 0.3333333333333333703, 0.3333333333333333703, 0.3333333333333333703, 0.3333333333333333703, 0.3333333333333333703, 0.3333333333333333703, 0.3333333333333333703, 0.3333333333333333703, 0.3333333333333333703, 0.3333333333333333703, 0.3333333333333333703, 0.3333333333333333703),
 ( 0.3333333333333333703, 0.3333333333333333703, 0.3333333333333333703, 0.3333333333333333703, 0.3333333333333333703, 0.3333333333333333703, 0.3333333333333333703, 0.3333333333333333703, 0.3333333333333333703, 0.3333333333333333703, 0.3333333333333333703, 0.3333333333333333703, 0.3333333333333333703, 0.3333333333333333703, 0.3333333333333333703, 0.3333333333333333703, 0.3333333333333333703, 0.3333333333333333703, 0.3333333333333333703, 0.3333333333333333703, 0.3333333333333333703, 0.3333333333333333703, 0.3333333333333333703, 0.3333333333333333703, 0.3333333333333333703, 0.3333333333333333703, 0.3333333333333333703, 0.3333333333333333703, 0.3333333333333333703, 0.3333333333333333703),
 ( 1.000000000000000000, 1.000000000000000000, 1.000000000000000000, 1.000000000000000000, 1.000000000000000000, 1.000000000000000000, 1.000000000000000000, 1.000000000000000000, 1.000000000000000000, 1.000000000000000000, 1.000000000000000000, 1.000000000000000000, 1.000000000000000000, 1.000000000000000000, 1.000000000000000000, 1.000000000000000000, 1.000000000000000000, 1.000000000000000000, 1.000000000000000000, 1.000000000000000000, 1.000000000000000000, 1.000000000000000000, 1.000000000000000000, 1.000000000000000000, 1.000000000000000000, 1.000000000000000000, 1.000000000000000000, 1.000000000000000000, 1.000000000000000000, 1.000000000000000000),
 ( 0.3333333333333333703, 0.3333333333333333703, 0.3333333333333333703, 0.3333333333333333703, 0.3333333333333333703, 0.3333333333333333703, 0.3333333333333333703, 0.3333333333333333703, 0.3333333333333333703, 0.3333333333333333703, 0.3333333333333333703, 0.3333333333333333703, 0.3333333333333333703, 0.3333333333333333703, 0.3333333333333333703, 0.3333333333333333703, 0.3333333333333333703, 0.3333333333333333703, 0.3333333333333333703, 0.3333333333333333703, 0.3333333333333333703, 0.3333333333333333703, 0.3333333333333333703, 0.3333333333333333703, 0.3333333333333333703, 0.3333333333333333703, 0.3333333333333333703, 0.3333333333333333703, 0.3333333333333333703, 0.3333333333333333703),
 ( 0.3333333333333333703, 0.3333333333333333703, 0.3333333333333333703, 0.3333333333333333703, 0.3333333333333333703, 0.3333333333333333703, 0.3333333333333333703, 0.3333333333333333703, 0.3333333333333333703, 0.3333333333333333703, 0.3333333333333333703, 0.3333333333333333703, 0.3333333333333333703, 0.3333333333333333703, 0.3333333333333333703, 0.3333333333333333703, 0.3333333333333333703, 0.3333333333333333703, 0.3333333333333333703, 0.3333333333333333703, 0.3333333333333333703, 0.3333333333333333703, 0.3333333333333333703, 0.3333333333333333703, 0.3333333333333333703, 0.3333333333333333703, 0.3333333333333333703, 0.3333333333333333703, 0.3333333333333333703, 0.3333333333333333703),
 ( 1.000000000000000000, 1.000000000000000000, 1.000000000000000000, 1.000000000000000000, 1.000000000000000000, 1.000000000000000000, 1.000000000000000000, 1.000000000000000000, 1.000000000000000000, 1.000000000000000000, 1.000000000000000000, 1.000000000000000000, 1.000000000000000000, 1.000000000000000000, 1.000000000000000000, 1.000000000000000000, 1.000000000000000000, 1.000000000000000000, 1.000000000000000000, 1.000000000000000000, 1.000000000000000000, 1.000000000000000000, 1.000000000000000000, 1.000000000000000000, 1.000000000000000000, 1.000000000000000000, 1.000000000000000000, 1.000000000000000000, 1.000000000000000000, 1.000000000000000000) ) ) 
 REPRESENTATION_ITEM ( '' )  SURFACE ( )  );
#9757 = CARTESIAN_POINT ( 'NONE',  ( -77.55640685876511498, -22.13135000837103661, -4.964495286674871776E-15 ) ) ;
#9758 = CARTESIAN_POINT ( 'NONE',  ( -162.0762913951020892, -29.48230308784785692, 29.48230308784751230 ) ) ;
#9759 = CARTESIAN_POINT ( 'NONE',  ( -198.0356074513804572, -39.99999999999990052, -15.37879056873112482 ) ) ;
#9760 = CARTESIAN_POINT ( 'NONE',  ( 170.0000000000000000, -24.95097643316997704, 0.000000000000000000 ) ) ;
#9761 = CARTESIAN_POINT ( 'NONE',  ( -135.8532207217289738, 6.472252184284096543, 6.472252184284234211 ) ) ;
#9762 = CARTESIAN_POINT ( 'NONE',  ( 0.2972598230770130412, -54.33493731733936016, -2.449293598294708485E-15 ) ) ;
#9763 = CARTESIAN_POINT ( 'NONE',  ( 91.82158438592159655, 12.16597498400028776, 44.40256751092339016 ) ) ;
#9764 = CARTESIAN_POINT ( 'NONE',  ( 14.38125909742182884, -55.17850393972636169, -2.449293598294708485E-15 ) ) ;
#9765 = CARTESIAN_POINT ( 'NONE',  ( 23.37394308801980713, -42.85717664514568526, -23.33966569535099822 ) ) ;
#9766 = CARTESIAN_POINT ( 'NONE',  ( -114.7799951756084482, 22.11694418166576526, 1.588013269880939271 ) ) ;
#9767 = CARTESIAN_POINT ( 'NONE',  ( 146.6084372240433709, -24.48358557860329299, 32.08495691632052882 ) ) ;
#9768 = CARTESIAN_POINT ( 'NONE',  ( -135.8532207217289738, -9.153146818113595984, -40.00000000000002132 ) ) ;
#9769 = ORIENTED_EDGE ( 'NONE', *, *, #19467, .T. ) ;
#9770 = EDGE_CURVE ( 'NONE', #15457, #18983, #23845, .T. ) ;
#9771 = CARTESIAN_POINT ( 'NONE',  ( 27.55177309529049268, -41.56868263114476747, 22.48880744267832199 ) ) ;
#9772 = CARTESIAN_POINT ( 'NONE',  ( 125.5832160019861021, 11.61997419108361385, 28.05309928654009610 ) ) ;
#9773 = CARTESIAN_POINT ( 'NONE',  ( 170.2234770963711128, 10.92277846919210660, -45.64576402573182889 ) ) ;
#9774 = CARTESIAN_POINT ( 'NONE',  ( 163.1118516004056573, -39.99999999999990052, -27.26290988616886679 ) ) ;
#9775 = CARTESIAN_POINT ( 'NONE',  ( 192.4448373802100889, -14.14213562375896061, 14.14213562375865330 ) ) ;
#9776 = EDGE_CURVE ( 'NONE', #8569, #17668, #6744, .T. ) ;
#9777 = CARTESIAN_POINT ( 'NONE',  ( 170.2234770963711128, -24.55285855007183926, 0.000000000000000000 ) ) ;
#9778 = CARTESIAN_POINT ( 'NONE',  ( 0.2972598230769930572, 14.33493731733933352, 0.000000000000000000 ) ) ;
#9779 = CARTESIAN_POINT ( 'NONE',  ( 200.0000000000001137, 18.84395317400427317, -2.458366139920278304 ) ) ;
#9780 = CARTESIAN_POINT ( 'NONE',  ( 199.9999999999999432, -11.82405030923947997, -14.88174658256811256 ) ) ;
#9781 = CARTESIAN_POINT ( 'NONE',  ( 170.2234770963711128, 39.20704971665372796, 17.36149277827039583 ) ) ;
#9782 = CARTESIAN_POINT ( 'NONE',  ( 57.59792236341147031, 30.00663442387720181, -26.56190807104661289 ) ) ;
#9783 = CARTESIAN_POINT ( 'NONE',  ( 14.38125909742181285, -10.73282306404727393, 10.73282306404716380 ) ) ;
#9784 = CARTESIAN_POINT ( 'NONE',  ( -192.9588430854689989, 1.161019517985663313E-13, -14.46834944099969533 ) ) ;
#9785 = CARTESIAN_POINT ( 'NONE',  ( -135.8532207217289738, -21.81201906317757633, -21.81201906317793515 ) ) ;
#9787 = CARTESIAN_POINT ( 'NONE',  ( 184.8905102610680444, -14.79361573936399665, 14.79361573936367158 ) ) ;
#9786 = CARTESIAN_POINT ( 'NONE',  ( 130.8568914410475088, 52.36146031193427319, -4.207082182989173802 ) ) ;
#9788 = CARTESIAN_POINT ( 'NONE',  ( -30.26275506840324070, -27.08623969584554558, -29.48230279907826912 ) ) ;
#9789 = CARTESIAN_POINT ( 'NONE',  ( -192.9588430854689989, -10.23066800230756890, 10.23066800230742501 ) ) ;
#9790 = CARTESIAN_POINT ( 'NONE',  ( 200.0000000000000000, -13.44239485489230290, 13.44239485489200803 ) ) ;
#9792 = CARTESIAN_POINT ( 'NONE',  ( -105.3755690713226585, -39.99999999999996447, -21.75974354311664527 ) ) ;
#9791 = CARTESIAN_POINT ( 'NONE',  ( 136.1360204305621551, 3.511608612530062512, 53.05693388239318864 ) ) ;
#9793 = CARTESIAN_POINT ( 'NONE',  ( 130.8568914410475372, -4.207082182992846420, 4.207082182992822439 ) ) ;
#9794 = CARTESIAN_POINT ( 'NONE',  ( 163.1118516004056573, -19.27778845538787422, 19.27778845538743724 ) ) ;
#9795 = CARTESIAN_POINT ( 'NONE',  ( -213.1075012329537230, 53.71589010953660193, 40.00000000000002132 ) ) ;
#9796 = EDGE_LOOP ( 'NONE', ( #6702, #20609, #2588, #6109, #20081, #18332, #1767, #2123 ) ) ;
#9797 = CARTESIAN_POINT ( 'NONE',  ( 163.1118516004056573, 9.006482792074356425, -47.56205970284957374 ) ) ;
#9798 = EDGE_CURVE ( 'NONE', #2419, #4199, #5949, .T. ) ;
#9799 = CYLINDRICAL_SURFACE ( 'NONE', #4863, 5.000000000000004441 ) ;
#9800 = DIRECTION ( 'NONE',  ( 1.000000000000000000, 0.000000000000000000, 0.000000000000000000 ) ) ;
#9801 = CARTESIAN_POINT ( 'NONE',  ( -100.7734535825088358, -22.67402823373193499, 0.000000000000000000 ) ) ;
#9802 = ORIENTED_EDGE ( 'NONE', *, *, #8633, .T. ) ;
#9803 = CARTESIAN_POINT ( 'NONE',  ( -195.1686598214593289, -44.46432177479800174, 24.52826087131761668 ) ) ;
#9804 = CARTESIAN_POINT ( 'NONE',  ( 199.9999999999998295, -18.94756416210704941, 1.560766781390804381 ) ) ;
#9805 = CARTESIAN_POINT ( 'NONE',  ( 9.349823541318809106, -18.59402391555502376, 44.88994471603710679 ) ) ;
#9806 = ADVANCED_FACE ( 'NONE', ( #9880 ), #21725, .F. ) ;
#9807 = EDGE_CURVE ( 'NONE', #21343, #15869, #4384, .T. ) ;
#9808 = B_SPLINE_CURVE_WITH_KNOTS ( 'NONE', 3,
 ( #10519, #10923, #14631, #22768, #22510, #12506 ),
 .UNSPECIFIED., .F., .F.,
 ( 4, 2, 4 ),
 ( -5.999999999808750012E-08, 0.04017169446089190188, 0.08034344892178379993 ),
 .UNSPECIFIED. ) ;
#9809 = CARTESIAN_POINT ( 'NONE',  ( 16.38602454699985955, 14.09104119328187821, -48.74566733939354179 ) ) ;
#9810 = CARTESIAN_POINT ( 'NONE',  ( 199.0054512189284424, 16.16316501604694622, -11.77153054567511425 ) ) ;
#9811 = DIRECTION ( 'NONE',  ( 0.000000000000000000, 0.000000000000000000, 1.000000000000000000 ) ) ;
#9812 = CARTESIAN_POINT ( 'NONE',  ( -114.4364955367301775, -8.064892380834896457, 20.29001642039033371 ) ) ;
#9813 = CARTESIAN_POINT ( 'NONE',  ( 184.8905102610680444, 13.49065550809826952, -13.49065550809790359 ) ) ;
#9814 = CARTESIAN_POINT ( 'NONE',  ( 163.1118516004056573, -12.73709011382472589, 40.00000000000002132 ) ) ;
#9815 = VECTOR ( 'NONE', #20521, 1000.000000000000000 ) ;
#9817 = CARTESIAN_POINT ( 'NONE',  ( -215.0000000000000284, 9.184850993605151889E-16, 0.000000000000000000 ) ) ;
#9816 = DIRECTION ( 'NONE',  ( 0.000000000000000000, -1.000000000000000000, 0.000000000000000000 ) ) ;
#9818 = CARTESIAN_POINT ( 'NONE',  ( 98.29820294273291381, -18.47759065023123526, -7.653668647304108674 ) ) ;
#9819 = CARTESIAN_POINT ( 'NONE',  ( 184.8905102610680444, 20.92133201514447549, 0.000000000000000000 ) ) ;
#9820 = CIRCLE ( 'NONE', #13233, 20.53474504356812247 ) ;
#9821 = CARTESIAN_POINT ( 'NONE',  ( -105.3755690713226727, -21.75974354311652093, 0.000000000000000000 ) ) ;
#9822 = CARTESIAN_POINT ( 'NONE',  ( -30.26275506840323359, 4.336144384597734078E-13, -41.69427246844629309 ) ) ;
#9823 = CARTESIAN_POINT ( 'NONE',  ( 192.4448373802101173, -40.00000000000019185, 20.00000000003900524 ) ) ;
#9824 = CARTESIAN_POINT ( 'NONE',  ( -208.1127848780264742, 17.67593391476678377, -38.89260858015718014 ) ) ;
#9825 = VERTEX_POINT ( 'NONE', #3367 ) ;
#9826 = DIRECTION ( 'NONE',  ( 0.000000000000000000, -1.000000000000000000, 0.000000000000000000 ) ) ;
#9827 = CARTESIAN_POINT ( 'NONE',  ( -30.26275506840324070, -1.694272468446265112, 0.000000000000000000 ) ) ;
#9828 = CARTESIAN_POINT ( 'NONE',  ( -315.0000000000000568, -4.857225732735059864E-14, 0.000000000000000000 ) ) ;
#9829 = ORIENTED_EDGE ( 'NONE', *, *, #3363, .T. ) ;
#9830 = ORIENTED_EDGE ( 'NONE', *, *, #3710, .T. ) ;
#9831 = CARTESIAN_POINT ( 'NONE',  ( 0.2972598230770153171, -66.70487387989861361, 10.13633138497438324 ) ) ;
#9832 = CARTESIAN_POINT ( 'NONE',  ( 23.13330272892113371, -43.07356808498585821, -17.84165608060053998 ) ) ;
#9833 = VERTEX_POINT ( 'NONE', #11468 ) ;
#9834 = CARTESIAN_POINT ( 'NONE',  ( -192.9588430854690273, 54.46834944098218756, -40.00000000000002132 ) ) ;
#9835 = DIRECTION ( 'NONE',  ( 1.836970198721030181E-16, -1.000000000000000000, 1.321694076934715579E-16 ) ) ;
#9836 = ORIENTED_EDGE ( 'NONE', *, *, #16711, .F. ) ;
#9837 = CARTESIAN_POINT ( 'NONE',  ( 200.0000000000000000, 18.87777001997802628, 2.191952217553565507 ) ) ;
#9838 = CIRCLE ( 'NONE', #14939, 5.000000000000004441 ) ;
#9839 = FACE_OUTER_BOUND ( 'NONE', #9033, .T. ) ;
#9840 = CARTESIAN_POINT ( 'NONE',  ( 199.9999999999999432, 14.14213562373090838, 14.14213562373092437 ) ) ;
#9841 = CARTESIAN_POINT ( 'NONE',  ( -188.4265466358331196, -47.03621809928752384, -13.83489705870362840 ) ) ;
#9842 = CARTESIAN_POINT ( 'NONE',  ( -86.96347745069643054, -40.00000000000009948, 18.24025645688337960 ) ) ;
#9843 = CARTESIAN_POINT ( 'NONE',  ( -213.1075012329537230, 13.71589010951907817, 40.00000000000002132 ) ) ;
#9844 = CARTESIAN_POINT ( 'NONE',  ( 4.995406935893290878, 39.06748935135239265, -39.06748935135144762 ) ) ;
#9845 = DIRECTION ( 'NONE',  ( -1.000000000000000000, 1.937599346585394162E-16, 0.000000000000000000 ) ) ;
#9846 = APPLICATION_CONTEXT ( 'automotive_design' ) ;
#9847 = CARTESIAN_POINT ( 'NONE',  ( 130.8568914410475372, 1.429239637432775288E-13, -34.05028731879788495 ) ) ;
#9848 = CARTESIAN_POINT ( 'NONE',  ( -259.2033419157646676, -40.00000000000017053, 9.517827891722212996 ) ) ;
#9849 = CARTESIAN_POINT ( 'NONE',  ( -110.1018001840479599, -14.72021915946409543, 13.84057942000516128 ) ) ;
#9850 = CARTESIAN_POINT ( 'NONE',  ( -213.1075012329537230, -9.698598906438496314, 66.26714140136188291 ) ) ;
#9851 = CARTESIAN_POINT ( 'NONE',  ( 170.2234770963711128, 24.55285855007190676, -40.00000000000002132 ) ) ;
#9852 = CARTESIAN_POINT ( 'NONE',  ( -56.48582580120558561, -50.09629031063963112, -6.472252184284449150 ) ) ;
#9853 = LINE ( 'NONE', #16236, #13439 ) ;
#9854 = CARTESIAN_POINT ( 'NONE',  ( 22.40986519363269025, -47.15972762675173868, 13.85314893102521161 ) ) ;
#9855 = CARTESIAN_POINT ( 'NONE',  ( -135.8532207217289738, 39.99999999999990763, 9.153146818113990335 ) ) ;
#9856 = CARTESIAN_POINT ( 'NONE',  ( 19.06497207195981858, -40.00000000000007105, 14.19242893257826665 ) ) ;
#9857 = CARTESIAN_POINT ( 'NONE',  ( 14.38125909742180397, 67.30136555895953165, 10.73282306403583242 ) ) ;
#9858 = CIRCLE ( 'NONE', #21348, 5.000000000000004441 ) ;
#9859 = CARTESIAN_POINT ( 'NONE',  ( 192.4448373802101173, -14.14213562370342281, 42.42640687122062104 ) ) ;
#9860 = CARTESIAN_POINT ( 'NONE',  ( -190.7346372395638241, -23.92885340725213439, -43.65255821760446509 ) ) ;
#9861 = CARTESIAN_POINT ( 'NONE',  ( -213.1075012329537230, -9.698598906450557777, 9.698598906450415669 ) ) ;
#9862 = ORIENTED_EDGE ( 'NONE', *, *, #16291, .T. ) ;
#9863 = CARTESIAN_POINT ( 'NONE',  ( -91.56559293963834989, -16.03295912088728414, 16.03295912088688269 ) ) ;
#9864 = CARTESIAN_POINT ( 'NONE',  ( -192.9588430854689989, -10.23066800230756890, 10.23066800230742501 ) ) ;
#9865 = CARTESIAN_POINT ( 'NONE',  ( -213.1075012329537230, -13.71589010951915810, 0.000000000000000000 ) ) ;
#9866 = PLANE ( 'NONE',  #23792 ) ;
#9867 = CARTESIAN_POINT ( 'NONE',  ( -280.0000000000000568, -42.42640687119276066, -14.14213562373147148 ) ) ;
#9868 = CARTESIAN_POINT ( 'NONE',  ( -82.30220482034381746, 7.441767004347251024, 18.74474319041271997 ) ) ;
#9869 = EDGE_LOOP ( 'NONE', ( #14516, #18953, #16851, #21083 ) ) ;
#9870 = CARTESIAN_POINT ( 'NONE',  ( 199.9999999999999147, 16.69452638465319083, -9.073307399871135104 ) ) ;
#9871 = CARTESIAN_POINT ( 'NONE',  ( 85.88498484994616433, -8.769905298562015616, -23.37206192994392140 ) ) ;
#9872 = CARTESIAN_POINT ( 'NONE',  ( -8.720657192110643052, 13.49580954686805079, 45.36528685023045426 ) ) ;
#9873 = VERTEX_POINT ( 'NONE', #1382 ) ;
#9874 = ORIENTED_EDGE ( 'NONE', *, *, #12981, .T. ) ;
#9875 = CARTESIAN_POINT ( 'NONE',  ( 4.995406935893289102, 10.78321810388998081, 10.78321810389001811 ) ) ;
#9876 = CARTESIAN_POINT ( 'NONE',  ( 199.0097900131551114, -3.258944298918965199, -19.73026277452668609 ) ) ;
#9877 = CARTESIAN_POINT ( 'NONE',  ( -362.0709805440841365, -4.857225732735059864E-14, 0.000000000000000000 ) ) ;
#9878 = CARTESIAN_POINT ( 'NONE',  ( -88.37877758186448318, -19.92653024483028190, -8.575405934408012243 ) ) ;
#9879 = EDGE_CURVE ( 'NONE', #21371, #10429, #18203, .T. ) ;
#9880 = FACE_OUTER_BOUND ( 'NONE', #3964, .T. ) ;
#9881 = CARTESIAN_POINT ( 'NONE',  ( 19.06497207195981147, 1.521599808664285085E-13, -14.19242893257840521 ) ) ;
#9882 = FACE_OUTER_BOUND ( 'NONE', #6622, .T. ) ;
#9883 = CARTESIAN_POINT ( 'NONE',  ( -629.5673161569764034, 26.57848330823986771, -29.89298347762988328 ) ) ;
#9884 = DIRECTION ( 'NONE',  ( 0.000000000000000000, 1.000000000000000000, 0.000000000000000000 ) ) ;
#9885 = CARTESIAN_POINT ( 'NONE',  ( 199.0157948715101668, 14.36126147255820484, 13.92041998760680066 ) ) ;
#9886 = CARTESIAN_POINT ( 'NONE',  ( -151.7004365449059264, 13.46261988209483640, 32.50163950446889061 ) ) ;
#9887 = CARTESIAN_POINT ( 'NONE',  ( 6.615221834219322083, -14.16446777330033768, -49.23097633541950557 ) ) ;
#9888 = CARTESIAN_POINT ( 'NONE',  ( 151.7948205124836534, 23.49921654116056047, -33.06932595376338213 ) ) ;
#9889 = CARTESIAN_POINT ( 'NONE',  ( -200.0000000000000284, -82.49999999999990052, 52.49999999999977973 ) ) ;
#9890 = CARTESIAN_POINT ( 'NONE',  ( -91.56559293963834989, -40.53558337403669753, -16.03295912088728770 ) ) ;
#9891 = CARTESIAN_POINT ( 'NONE',  ( -86.96347745069644475, -2.438961472018186339E-13, 21.75974354311649961 ) ) ;
#9892 = CARTESIAN_POINT ( 'NONE',  ( -238.4067589809705794, 0.6820004457912851592, -0.6820004457913123597 ) ) ;
#9893 = CARTESIAN_POINT ( 'NONE',  ( -208.1127848780264742, 17.67593391476678377, -38.89260858015718014 ) ) ;
#9894 = CARTESIAN_POINT ( 'NONE',  ( 57.59792236341148453, -37.56421063658185489, -2.449293598294708485E-15 ) ) ;
#9895 = FACE_OUTER_BOUND ( 'NONE', #20949, .T. ) ;
#9896 = CARTESIAN_POINT ( 'NONE',  ( -213.1075012329537230, -53.71589010950170717, 40.00000000000002132 ) ) ;
#9897 = CARTESIAN_POINT ( 'NONE',  ( -102.4068193528148072, 20.44188272012841878, -8.088405365069068154 ) ) ;
#9898 = CARTESIAN_POINT ( 'NONE',  ( 0.2972598230769883387, 40.00000000000017053, -14.33493731733891607 ) ) ;
#9899 = CARTESIAN_POINT ( 'NONE',  ( -56.48582580120559982, 21.81201906317778594, -34.75652343174606074 ) ) ;
#9900 = CARTESIAN_POINT ( 'NONE',  ( 0.2972598230769930572, 14.33493731733933352, 0.000000000000000000 ) ) ;
#9901 = ORIENTED_EDGE ( 'NONE', *, *, #16818, .T. ) ;
#9902 = CARTESIAN_POINT ( 'NONE',  ( 27.55177309528321317, -45.29548561697026088, 13.49150912998325325 ) ) ;
#9903 = DIRECTION ( 'NONE',  ( 0.000000000000000000, -1.000000000000000000, 0.000000000000000000 ) ) ;
#9904 = CARTESIAN_POINT ( 'NONE',  ( -259.2033419157646676, 21.55415060305839958, -35.01439189186541512 ) ) ;
#9905 = CARTESIAN_POINT ( 'NONE',  ( -208.1127848780264742, -40.00000000000025580, 55.00245453014408525 ) ) ;
#9906 = CARTESIAN_POINT ( 'NONE',  ( 0.2972598230769886718, 38.42060263243643448, 18.14793986248763957 ) ) ;
#9907 = DIRECTION ( 'NONE',  ( 0.000000000000000000, -1.000000000000000000, 0.000000000000000000 ) ) ;
#9908 = CARTESIAN_POINT ( 'NONE',  ( 57.59792236341147031, 37.56421063658187620, -40.00000000000002132 ) ) ;
#9909 = DIRECTION ( 'NONE',  ( 0.000000000000000000, 0.000000000000000000, 1.000000000000000000 ) ) ;
#9910 = CARTESIAN_POINT ( 'NONE',  ( 199.9999999999996874, 18.57765777299087873, -3.990914148134230288 ) ) ;
#9911 = CARTESIAN_POINT ( 'NONE',  ( 199.9999999999998863, -15.63633292130449703, 10.81305911573160472 ) ) ;
#9912 = CARTESIAN_POINT ( 'NONE',  ( 4.995406935893286438, 67.35176059880245703, -10.78321810387767066 ) ) ;
#9913 = CARTESIAN_POINT ( 'NONE',  ( -198.0356074513804572, -67.44298959253333692, -10.87444709761016348 ) ) ;
#9914 = CARTESIAN_POINT ( 'NONE',  ( -188.2995950289364941, -46.99046209955528042, 13.82811170417144453 ) ) ;
#9915 = CARTESIAN_POINT ( 'NONE',  ( -77.67315633212002979, 18.60060890640625075, -11.80559230994880515 ) ) ;
#9916 = CARTESIAN_POINT ( 'NONE',  ( 151.7948205124836250, -4.785054706301600902, -4.785054706301715477 ) ) ;
#9918 = FACE_OUTER_BOUND ( 'NONE', #13584, .T. ) ;
#9917 = CARTESIAN_POINT ( 'NONE',  ( 57.59792236341148453, -26.56190807104663421, -26.56190807104710672 ) ) ;
#9919 = CARTESIAN_POINT ( 'NONE',  ( 57.59792236341147031, -30.00663442387662627, -26.56190807104723461 ) ) ;
#9920 = CARTESIAN_POINT ( 'NONE',  ( -280.0000000000000000, 14.14213562373098299, -14.14213562373088706 ) ) ;
#9921 = CARTESIAN_POINT ( 'NONE',  ( 199.0263117993877131, -12.25726513653892447, 15.86500832304671427 ) ) ;
#9923 = CARTESIAN_POINT ( 'NONE',  ( 91.82158438592159655, -39.99999999999994316, -17.20528682183314118 ) ) ;
#9922 = CARTESIAN_POINT ( 'NONE',  ( -91.56559293963834989, -16.03295912088659492, -40.53558337403696044 ) ) ;
#9924 = CARTESIAN_POINT ( 'NONE',  ( 184.8905102610680444, 43.07788698682572459, 13.49065550809829439 ) ) ;
#9925 = CARTESIAN_POINT ( 'NONE',  ( -208.1127848780265026, -10.60833733269537227, -10.60833733269551793 ) ) ;
#9926 = CARTESIAN_POINT ( 'NONE',  ( 9.006212071484325676, 49.32687279761466215, -14.17897189021863902 ) ) ;
#9927 = CARTESIAN_POINT ( 'NONE',  ( 184.8905102610680444, -20.92133201514440799, 40.00000000000002132 ) ) ;
#9928 = ORIENTED_EDGE ( 'NONE', *, *, #20307, .F. ) ;
#9929 = CARTESIAN_POINT ( 'NONE',  ( -210.0000000000000284, 57.47694228411666728, -64.52066607436458412 ) ) ;
#9930 = CARTESIAN_POINT ( 'NONE',  ( -5.983078567328675490, 41.77006127201591568, 17.30172588002420753 ) ) ;
#9931 = CARTESIAN_POINT ( 'NONE',  ( -716.9846540392142060, -52.49999999999991473, 82.49999999999998579 ) ) ;
#9932 = CARTESIAN_POINT ( 'NONE',  ( 200.0000000000000000, 66.50000000000009948, 66.50000000000005684 ) ) ;
#9933 = ORIENTED_EDGE ( 'NONE', *, *, #21432, .T. ) ;
#9934 = CARTESIAN_POINT ( 'NONE',  ( -189.0540043421004270, -43.34487664254536554, 17.95403576473164264 ) ) ;
#9935 = CARTESIAN_POINT ( 'NONE',  ( 199.9999999999994031, -18.37269623729978107, -4.912321869774860517 ) ) ;
#9936 = CARTESIAN_POINT ( 'NONE',  ( 16.03312633940209153, -18.43342098164813336, 44.50221493480265877 ) ) ;
#9937 = CARTESIAN_POINT ( 'NONE',  ( 22.75882399337413986, 17.88527043150909890, -43.17886244245817551 ) ) ;
#9938 = CARTESIAN_POINT ( 'NONE',  ( 199.0186803405091780, -17.32754287553631301, -9.995805879000721816 ) ) ;
#9939 = LINE ( 'NONE', #22061, #13436 ) ;
#9940 = LINE ( 'NONE', #22197, #10568 ) ;
#9941 = EDGE_CURVE ( 'NONE', #21338, #21343, #19902, .T. ) ;
#9942 = CARTESIAN_POINT ( 'NONE',  ( -105.3755690713226585, 41.18208027870575449, 15.38646221621837107 ) ) ;
#9943 = CARTESIAN_POINT ( 'NONE',  ( 130.8568914410475088, -5.949712681206671405, 40.00000000000002132 ) ) ;
#9945 = CARTESIAN_POINT ( 'NONE',  ( -30.26275506840325136, 29.48230279907760121, 27.08623969584625613 ) ) ;
#9944 = CARTESIAN_POINT ( 'NONE',  ( -188.9001659262682722, 17.93767091109533496, -43.30536839095024959 ) ) ;
#9946 = ADVANCED_FACE ( 'NONE', ( #14135, #13998 ), #22129, .T. ) ;
#9947 = CARTESIAN_POINT ( 'NONE',  ( -348.0000000000001137, -4.857225732735059864E-14, 0.000000000000000000 ) ) ;
#9948 = CARTESIAN_POINT ( 'NONE',  ( -30.26275506840324425, -1.694272468446265334, -40.00000000000002132 ) ) ;
#9949 = CARTESIAN_POINT ( 'NONE',  ( 199.9999999999999432, -20.00000000000006750, 0.000000000000000000 ) ) ;
#9950 = CARTESIAN_POINT ( 'NONE',  ( 163.1118516004056573, 1.658263919738574066E-13, -12.73709011382475254 ) ) ;
#9951 = CARTESIAN_POINT ( 'NONE',  ( 136.1360204305621266, 3.511608612530704665, 3.511608612530695339 ) ) ;
#9952 = CARTESIAN_POINT ( 'NONE',  ( -91.56559293963834989, -2.543181659092656077E-13, 22.67402823373191723 ) ) ;
#9953 = CARTESIAN_POINT ( 'NONE',  ( 91.82158438592158234, 12.16597498397756993, 12.16597498397776356 ) ) ;
#9954 = EDGE_CURVE ( 'NONE', #15005, #6531, #8809, .T. ) ;
#9955 = EDGE_CURVE ( 'NONE', #22348, #3897, #18694, .T. ) ;
#9956 = ORIENTED_EDGE ( 'NONE', *, *, #10708, .F. ) ;
#9957 = CARTESIAN_POINT ( 'NONE',  ( -238.4067589809705794, -27.60227080167069147, 28.96627169325319429 ) ) ;
#9958 = CARTESIAN_POINT ( 'NONE',  ( 57.59792236341147031, 2.435789363418171760, 0.000000000000000000 ) ) ;
#9959 = CARTESIAN_POINT ( 'NONE',  ( -88.38011429763034243, -8.298859915572245782, 20.03522015847540061 ) ) ;
#9960 = SHAPE_DEFINITION_REPRESENTATION ( #2559, #15720 ) ;
#9961 = ORIENTED_EDGE ( 'NONE', *, *, #23375, .T. ) ;
#9962 = VERTEX_POINT ( 'NONE', #3909 ) ;
#9963 = B_SPLINE_CURVE_WITH_KNOTS ( 'NONE', 3,
 ( #754, #13490, #13980, #6269, #17603, #1397 ),
 .UNSPECIFIED., .F., .F.,
 ( 4, 2, 4 ),
 ( 2.453269466693398698E-18, 0.004090000753319153470, 0.008180001506638303471 ),
 .UNSPECIFIED. ) ;
#9964 = CARTESIAN_POINT ( 'NONE',  ( -238.4067589809705794, -57.25054294065807881, 0.6820004457338858517 ) ) ;
#9965 = CARTESIAN_POINT ( 'NONE',  ( 22.89002945277386303, -43.14209108112270741, -17.87003923493590207 ) ) ;
#9966 = EDGE_LOOP ( 'NONE', ( #16815, #5514, #23671, #8331 ) ) ;
#9967 = CARTESIAN_POINT ( 'NONE',  ( 4.995406935893289102, 55.24977328856464709, -40.00000000000002132 ) ) ;
#9968 = CARTESIAN_POINT ( 'NONE',  ( 210.0000000000000284, 57.47694228411675255, -64.52066607436459833 ) ) ;
#9969 = VERTEX_POINT ( 'NONE', #12402 ) ;
#9970 = CARTESIAN_POINT ( 'NONE',  ( 200.0000000000000284, 12.51656570147539327, 14.30544205704861760 ) ) ;
#9971 = DIRECTION ( 'NONE',  ( 0.000000000000000000, -1.000000000000000000, 0.000000000000000000 ) ) ;
#9972 = CARTESIAN_POINT ( 'NONE',  ( -135.8532207217289738, -6.472252184284190690, -6.472252184284188914 ) ) ;
#9973 = CARTESIAN_POINT ( 'NONE',  ( -188.2507053403089969, -46.97353740712736681, -13.82466505297411352 ) ) ;
#9974 = CARTESIAN_POINT ( 'NONE',  ( -198.0356074513804572, -2.321818583541004323E-13, 55.37879056873073580 ) ) ;
#9975 = CARTESIAN_POINT ( 'NONE',  ( 151.7948205124836534, -33.23291073765550863, 40.00000000000002132 ) ) ;
#9976 = CARTESIAN_POINT ( 'NONE',  ( 151.7948205124836250, 4.785054706301759886, -4.785054706301612448 ) ) ;
#9977 = CARTESIAN_POINT ( 'NONE',  ( 199.0232347278000873, 0.3099713519423794028, 20.00382596759649800 ) ) ;
#9978 = CARTESIAN_POINT ( 'NONE',  ( -238.4067589809705794, -40.00000000000007105, 0.9644942799824426372 ) ) ;
#9979 = CARTESIAN_POINT ( 'NONE',  ( 163.1118516004056573, -39.99999999999986500, -12.73709011382517353 ) ) ;
#9980 = CARTESIAN_POINT ( 'NONE',  ( -105.2276882640349811, -13.16704209471193643, 17.02247659824342563 ) ) ;
#9981 = CARTESIAN_POINT ( 'NONE',  ( 91.82158438592159655, -44.40256751092324095, -12.16597498400075139 ) ) ;
#9982 = CARTESIAN_POINT ( 'NONE',  ( 199.9999999999999432, 20.00000000000013856, 0.000000000000000000 ) ) ;
#9983 = CARTESIAN_POINT ( 'NONE',  ( 130.8568914410475088, -4.207082182989324792, -52.36146031193423056 ) ) ;
#9984 = CARTESIAN_POINT ( 'NONE',  ( -362.0709805440841365, 10.00000000000000000, 0.000000000000000000 ) ) ;
#9985 = LINE ( 'NONE', #21029, #20451 ) ;
#9986 = CARTESIAN_POINT ( 'NONE',  ( 184.8905102610680444, -1.851754852062639767E-13, 20.92133201514444352 ) ) ;
#9987 = CARTESIAN_POINT ( 'NONE',  ( 4.995406935893290878, -5.232665749138292703E-14, 15.24977328854832592 ) ) ;
#9988 = AXIS2_PLACEMENT_3D ( 'NONE', #3324, #25809, #15175 ) ;
#9989 = CARTESIAN_POINT ( 'NONE',  ( 0.2972598230769886718, 38.42060263243669027, -18.14793986248710667 ) ) ;
#9990 = CARTESIAN_POINT ( 'NONE',  ( 130.8568914410475088, -4.207082182990058428, 52.36146031193416661 ) ) ;
#9991 = CARTESIAN_POINT ( 'NONE',  ( -188.4702232936801920, -13.83721295434097698, -47.05182887786487100 ) ) ;
#9992 = CARTESIAN_POINT ( 'NONE',  ( 160.7895100360958622, -2.688594056682756800E-13, 28.48799984206441138 ) ) ;
#9993 = ORIENTED_EDGE ( 'NONE', *, *, #11249, .F. ) ;
#9994 = CARTESIAN_POINT ( 'NONE',  ( -238.4067589809705794, 0.6820004457912851592, -0.6820004457913123597 ) ) ;
#9995 = DIRECTION ( 'NONE',  ( -0.000000000000000000, -1.000000000000000000, -0.000000000000000000 ) ) ;
#9996 = CARTESIAN_POINT ( 'NONE',  ( 57.59792236341147031, 1.722363176415065089, -1.722363176415036445 ) ) ;
#9997 = CARTESIAN_POINT ( 'NONE',  ( -135.8532207217289738, 9.153146818113546246, -0.000000000000000000 ) ) ;
#9998 = CARTESIAN_POINT ( 'NONE',  ( 35.93739780938212647, 20.78453051354052761, 38.99308239399191933 ) ) ;
#9999 = CARTESIAN_POINT ( 'NONE',  ( 91.82158438592158234, -40.45024623143936537, -16.11829626348475131 ) ) ;
#10000 = DIRECTION ( 'NONE',  ( 0.9352143328345786655, 0.1355013631633526505, 0.3271292286568833751 ) ) ;
#10001 = ORIENTED_EDGE ( 'NONE', *, *, #25827, .F. ) ;
#10002 = AXIS2_PLACEMENT_3D ( 'NONE', #2880, #749, #12977 ) ;
#10003 = CARTESIAN_POINT ( 'NONE',  ( 199.9999999999999432, 18.40126832602490481, -4.753217589480088989 ) ) ;
#10004 = CARTESIAN_POINT ( 'NONE',  ( -105.2110227778625955, -16.13864963246017226, 14.20565731140640153 ) ) ;
#10005 = CARTESIAN_POINT ( 'NONE',  ( -7.769366557096160975, 13.56374645827035330, 45.69637362128187164 ) ) ;
#10006 = ORIENTED_EDGE ( 'NONE', *, *, #2171, .F. ) ;
#10007 = EDGE_LOOP ( 'NONE', ( #11646, #19085, #9688, #24519 ) ) ;
#10008 = CARTESIAN_POINT ( 'NONE',  ( 192.4448373802100889, -20.00000000003938538, 0.000000000000000000 ) ) ;
#10009 = CARTESIAN_POINT ( 'NONE',  ( 199.0099327931564233, -3.581876008808642098, -19.67427284064525139 ) ) ;
#10010 = CARTESIAN_POINT ( 'NONE',  ( -105.3178975793838532, 5.416379678185476720, 20.76461410732419921 ) ) ;
#10011 = CARTESIAN_POINT ( 'NONE',  ( -213.1075012329537230, 9.698598906450410340, 9.698598906450483170 ) ) ;
#10012 = CARTESIAN_POINT ( 'NONE',  ( -96.94475454972024409, -9.001119816611835134, -20.58449551011104361 ) ) ;
#10013 = CARTESIAN_POINT ( 'NONE',  ( 146.6084372240433993, -3.357462877844280890E-13, 34.62501878078305850 ) ) ;
#10014 = CARTESIAN_POINT ( 'NONE',  ( 199.9999999999998863, -16.91159699891635171, 8.687942971654136315 ) ) ;
#10015 = VECTOR ( 'NONE', #2873, 1000.000000000000000 ) ;
#10016 = CIRCLE ( 'NONE', #13010, 69.99999999999998579 ) ;
#10017 = CARTESIAN_POINT ( 'NONE',  ( 199.0225339954500328, 2.108197227390415929, 19.89250884296043864 ) ) ;
#10018 = DIRECTION ( 'NONE',  ( 1.000000000000000000, 1.836970198721030427E-16, -0.000000000000000000 ) ) ;
#10019 = CARTESIAN_POINT ( 'NONE',  ( -4.082462733454481629, -23.44093842354198287, -42.99255347688251305 ) ) ;
#10020 = CARTESIAN_POINT ( 'NONE',  ( -135.8532207217289738, -50.09629031063973770, 6.472252184283735943 ) ) ;
#10021 = CARTESIAN_POINT ( 'NONE',  ( -114.5520604218033327, -9.956332160911816942, -19.58753817072744496 ) ) ;
#10022 = CARTESIAN_POINT ( 'NONE',  ( 184.8905102610680444, -13.49065550809780412, -43.07788698682583828 ) ) ;
#10023 = CARTESIAN_POINT ( 'NONE',  ( -192.9588430854689989, 1.161019517985663313E-13, -14.46834944099969533 ) ) ;
#10024 = CARTESIAN_POINT ( 'NONE',  ( 0.2972598230769976091, -10.13633138497465147, -10.13633138497482733 ) ) ;
#10025 = CARTESIAN_POINT ( 'NONE',  ( -192.9588430854690273, -54.46834944098226572, 40.00000000000002132 ) ) ;
#10026 = AXIS2_PLACEMENT_3D ( 'NONE', #22793, #20795, #8947 ) ;
#10027 = CARTESIAN_POINT ( 'NONE',  ( -215.0000000000000284, 63.70262460423102624, -57.69613583541415380 ) ) ;
#10028 = CARTESIAN_POINT ( 'NONE',  ( -100.7734535825088358, -17.32597176626813251, -2.449293598294708485E-15 ) ) ;
#10029 = CARTESIAN_POINT ( 'NONE',  ( -105.2800168526293874, 11.81670533840901349, 17.89480874142644495 ) ) ;
#10030 = ADVANCED_FACE ( 'NONE', ( #16260 ), #7723, .T. ) ;
#10031 = CARTESIAN_POINT ( 'NONE',  ( 192.4448373802101173, 40.00000000000026290, -19.99999999996018474 ) ) ;
#10032 = CARTESIAN_POINT ( 'NONE',  ( 130.8568914410475372, -24.07718906447222551, -24.07718906447233209 ) ) ;
#10033 = CARTESIAN_POINT ( 'NONE',  ( 4.995406935893288214, 15.24977328854832770, 0.000000000000000000 ) ) ;
#10034 = ORIENTED_EDGE ( 'NONE', *, *, #25821, .F. ) ;
#10035 = EDGE_LOOP ( 'NONE', ( #23584, #3200, #25176, #4982 ) ) ;
#10036 = CARTESIAN_POINT ( 'NONE',  ( -238.4067589809705794, 0.9644942799825386714, 0.000000000000000000 ) ) ;
#10037 = CLOSED_SHELL ( 'NONE', ( #1344, #18404, #14041, #4705, #5818, #4310, #8981, #1351, #1128, #23456, #24175, #6061, #11417, #9245, #3052, #23613, #15293, #19712, #3765, #22893, #2491, #16398, #18431, #10865, #22490, #17987, #5713, #1831, #20641, #4210, #21821, #9656, #3290, #14663, #22308, #20697, #13615, #5175, #9151, #3932, #2156, #10634, #6467, #22266, #19239, #5120, #4121, #14673, #19798, #22652, #14743, #5087, #22686, #17750, #18579, #7327, #16550, #359, #2490, #14428, #13938, #881, #639, #9140, #7053, #2080, #199, #14007, #21123, #1016, #25260, #4455, #10977, #11347, #12807, #356, #11728, #20968, #10784, #23090, #6719, #8294, #22159, #14531, #6197, #6953, #8247, #18916, #6568, #7658, #23762, #20128, #4450, #17907, #10782, #20189, #4691, #15568, #26326, #11416, #10030, #14285, #17751, #23445, #16723, #8681, #13472, #20535, #7575, #12885, #198, #6527, #7273, #16966, #23487, #17203, #1827, #25507 ) ) ;
#10038 = CARTESIAN_POINT ( 'NONE',  ( 128.5824617753800965, 11.99766463964378360, 28.96492468983284851 ) ) ;
#10039 = CARTESIAN_POINT ( 'NONE',  ( -162.0762913951020892, -1.777970010055771463E-13, 41.69427287682835015 ) ) ;
#10040 = CARTESIAN_POINT ( 'NONE',  ( 170.2234770963711128, 10.92277846919147066, 45.64576402573197811 ) ) ;
#10041 = CARTESIAN_POINT ( 'NONE',  ( -210.0000000000000284, -66.50000000000001421, 66.50000000000005684 ) ) ;
#10042 = EDGE_CURVE ( 'NONE', #25804, #16337, #15286, .T. ) ;
#10043 = CIRCLE ( 'NONE', #21634, 21.53474504356810115 ) ;
#10044 = VECTOR ( 'NONE', #8246, 1000.000000000000000 ) ;
#10045 = CARTESIAN_POINT ( 'NONE',  ( -163.5815439468644854, -12.03526835479589430, -38.33196286469318181 ) ) ;
#10046 = CARTESIAN_POINT ( 'NONE',  ( -109.1264249741457633, 13.72187187126429997, 33.12752917268171871 ) ) ;
#10047 = CARTESIAN_POINT ( 'NONE',  ( 199.9999999999997442, 15.07190321012488887, 11.58049570127731798 ) ) ;
#10048 = CARTESIAN_POINT ( 'NONE',  ( 199.9999999999999716, -17.84994651634582397, 6.552042691338741953 ) ) ;
#10049 = CARTESIAN_POINT ( 'NONE',  ( -259.2033419157646676, 49.83842185052017015, 6.730120644404137487 ) ) ;
#10050 = CARTESIAN_POINT ( 'NONE',  ( 199.9999999999999432, -14.14213562373073607, -14.14213562373102206 ) ) ;
#10051 = CARTESIAN_POINT ( 'NONE',  ( -114.6112526615690115, 21.20804461678012132, 5.819739293988868134 ) ) ;
#10052 = CARTESIAN_POINT ( 'NONE',  ( -77.79459117305557925, 19.55393134992732129, -9.938707241617530386 ) ) ;
#10053 = CARTESIAN_POINT ( 'NONE',  ( -105.3755690713226585, -12.89780903124444578, 43.67073346367968156 ) ) ;
#10054 = CARTESIAN_POINT ( 'NONE',  ( -87.10563802237744824, 13.14174799572376706, -16.99650074894995910 ) ) ;
#10055 = CARTESIAN_POINT ( 'NONE',  ( -213.1075012329537230, 9.698598906450543566, -9.698598906450348167 ) ) ;
#10056 = CARTESIAN_POINT ( 'NONE',  ( 170.2234770963711128, 17.36149277827004411, -17.36149277826983095 ) ) ;
#10057 = CARTESIAN_POINT ( 'NONE',  ( 199.0197853254965707, 8.008002382618863990, 18.32953931431698535 ) ) ;
#10058 = EDGE_CURVE ( 'NONE', #13429, #23676, #8599, .T. ) ;
#10060 = CARTESIAN_POINT ( 'NONE',  ( 170.2234770963711128, 1.169953928977015745E-13, -24.55285855007187124 ) ) ;
#10059 = CARTESIAN_POINT ( 'NONE',  ( 14.38125909742180397, 67.30136555898270956, -10.73282306405792319 ) ) ;
#10061 = CARTESIAN_POINT ( 'NONE',  ( 0.2972598230769976091, -10.13633138497465147, -10.13633138497482733 ) ) ;
#10062 = CARTESIAN_POINT ( 'NONE',  ( 21.25019396254074167, 43.56030393975865422, -18.04326867293220360 ) ) ;
#10063 = CARTESIAN_POINT ( 'NONE',  ( -213.1075012329537230, 53.71589010950162191, -40.00000000000002132 ) ) ;
#10064 = ORIENTED_EDGE ( 'NONE', *, *, #4931, .T. ) ;
#10065 = CARTESIAN_POINT ( 'NONE',  ( -238.4067589809705794, 0.9644942799825386714, 0.000000000000000000 ) ) ;
#10066 = AXIS2_PLACEMENT_3D ( 'NONE', #11472, #1001, #23222 ) ;
#10067 = CARTESIAN_POINT ( 'NONE',  ( -4.201409602816648992, -46.93439176590693052, 13.81669219312499486 ) ) ;
#10068 = CARTESIAN_POINT ( 'NONE',  ( -208.1127848780264742, 15.00245453012665742, 40.00000000000002132 ) ) ;
#10069 = VERTEX_POINT ( 'NONE', #18928 ) ;
#10070 = CARTESIAN_POINT ( 'NONE',  ( -188.6013476421594817, -43.09288642756992971, 23.51433506917121008 ) ) ;
#10071 = CIRCLE ( 'NONE', #21142, 14.99999999999999467 ) ;
#10072 = CARTESIAN_POINT ( 'NONE',  ( 200.0000000000003411, -18.28334586770733594, 5.214203034309022655 ) ) ;
#10073 = CARTESIAN_POINT ( 'NONE',  ( -3.696864809816500230, -23.52297716615279555, 43.10456217110754551 ) ) ;
#10074 = CARTESIAN_POINT ( 'NONE',  ( 23.54890483848213378, 13.78807129923295527, -46.74501720879577960 ) ) ;
#10075 = CARTESIAN_POINT ( 'NONE',  ( 199.0080442515877905, 1.130919702028742257, -19.96471691786700120 ) ) ;
#10076 = CARTESIAN_POINT ( 'NONE',  ( 190.0000000000000000, 52.49999999999987210, 82.49999999999998579 ) ) ;
#10077 = CARTESIAN_POINT ( 'NONE',  ( -187.7699188115033735, -13.79076593538429130, 46.80708926513559476 ) ) ;
#10078 = CARTESIAN_POINT ( 'NONE',  ( 151.7948205124836534, 33.06932595376333239, 23.49921654116065284 ) ) ;
#10079 = CARTESIAN_POINT ( 'NONE',  ( -135.8532207217289738, 9.153146818113546246, -0.000000000000000000 ) ) ;
#10081 = CARTESIAN_POINT ( 'NONE',  ( -162.0762913951021176, 29.48230308784730980, 27.08623940707652622 ) ) ;
#10080 = CARTESIAN_POINT ( 'NONE',  ( -190.0144721489061794, 23.79987203025343234, -43.47822244622717136 ) ) ;
#10082 = CARTESIAN_POINT ( 'NONE',  ( -210.0000000000000284, 63.70262460423102624, -57.69613583541415380 ) ) ;
#10083 = CARTESIAN_POINT ( 'NONE',  ( -208.1127848780264742, -55.00245453014425578, -40.00000000000002132 ) ) ;
#10084 = CARTESIAN_POINT ( 'NONE',  ( -135.8532207217289738, 30.84685318188643066, 2.449293598294708485E-15 ) ) ;
#10085 = CARTESIAN_POINT ( 'NONE',  ( -105.3755690713226585, -39.99999999999985079, -18.24025645688394448 ) ) ;
#10086 = CARTESIAN_POINT ( 'NONE',  ( -135.8532207217289738, 50.09629031063965243, -6.472252184284084109 ) ) ;
#10087 = CARTESIAN_POINT ( 'NONE',  ( 14.38125909742181108, 1.616281842095393922E-13, -15.17850393972633682 ) ) ;
#10088 = CARTESIAN_POINT ( 'NONE',  ( 98.29820294273291381, -18.47759065023123526, -7.653668647304108674 ) ) ;
#10089 = EDGE_LOOP ( 'NONE', ( #9993, #24065, #21429, #22083 ) ) ;
#10090 = CARTESIAN_POINT ( 'NONE',  ( 192.4448373802101173, -42.42640687122073473, 14.14213562370301780 ) ) ;
#10091 = B_SPLINE_CURVE_WITH_KNOTS ( 'NONE', 3,
 ( #22691, #2330, #20559, #6311, #336, #20294 ),
 .UNSPECIFIED., .F., .F.,
 ( 4, 2, 4 ),
 ( 1.142150420466554580E-15, 0.03937685942888059787, 0.07875371885776004388 ),
 .UNSPECIFIED. ) ;
#10092 = CARTESIAN_POINT ( 'NONE',  ( -99.31267923333879821, -8.544756979511673123, 20.62886818714596160 ) ) ;
#10093 = APPLICATION_PROTOCOL_DEFINITION ( 'draft international standard', 'automotive_design', 1998, #16389 ) ;
#10094 = VERTEX_POINT ( 'NONE', #7075 ) ;
#10095 = ORIENTED_EDGE ( 'NONE', *, *, #737, .T. ) ;
#10096 = CARTESIAN_POINT ( 'NONE',  ( 200.0000000000000000, -42.42640687119269671, -14.14213562373124766 ) ) ;
#10097 = CARTESIAN_POINT ( 'NONE',  ( 23.35928221536255833, -46.81377789283288848, -13.80178577956144181 ) ) ;
#10098 = VERTEX_POINT ( 'NONE', #17181 ) ;
#10099 = CARTESIAN_POINT ( 'NONE',  ( -259.2033419157646676, -9.517827891722680178, 0.000000000000000000 ) ) ;
#10100 = CARTESIAN_POINT ( 'NONE',  ( -86.86493150571114086, -8.366608963953822808, -19.60045294882766598 ) ) ;
#10101 = EDGE_CURVE ( 'NONE', #3856, #4168, #24793, .T. ) ;
#10102 = ORIENTED_EDGE ( 'NONE', *, *, #3703, .T. ) ;
#10103 = CARTESIAN_POINT ( 'NONE',  ( 199.9999999999998295, 8.812783067309094776, 16.84096882534935702 ) ) ;
#10104 = CARTESIAN_POINT ( 'NONE',  ( -190.0000000000000000, 66.50000000000009948, 66.50000000000005684 ) ) ;
#10105 = CARTESIAN_POINT ( 'NONE',  ( -100.7734535825088358, -16.03295912088706743, -16.03295912088710296 ) ) ;
#10106 = EDGE_CURVE ( 'NONE', #25810, #1453, #8009, .T. ) ;
#10107 = CARTESIAN_POINT ( 'NONE',  ( -129.2920262391662050, -25.26067940890114372, -10.46331600579726739 ) ) ;
#10108 = CARTESIAN_POINT ( 'NONE',  ( -105.3755690713226585, -39.99999999999996447, -21.75974354311664527 ) ) ;
#10109 = CARTESIAN_POINT ( 'NONE',  ( -30.26275506840324070, 1.694272468446254232, 0.000000000000000000 ) ) ;
#10110 = CARTESIAN_POINT ( 'NONE',  ( -192.9588430854690273, 10.23066800229588758, -66.79921049721882298 ) ) ;
#10111 = CARTESIAN_POINT ( 'NONE',  ( 199.0263771359574889, -13.68429728450633753, 14.60718570525551563 ) ) ;
#10112 = EDGE_CURVE ( 'NONE', #5117, #26151, #439, .T. ) ;
#10113 = CARTESIAN_POINT ( 'NONE',  ( -30.26275506840324070, -40.00000000000003553, 1.694272468446120117 ) ) ;
#10114 = CARTESIAN_POINT ( 'NONE',  ( 184.8905102610680444, -39.99999999999991473, -20.92133201514458207 ) ) ;
#10115 = CARTESIAN_POINT ( 'NONE',  ( 136.1360204305621551, -40.00000000000036238, 35.03383547441254109 ) ) ;
#10116 = CARTESIAN_POINT ( 'NONE',  ( -213.1075012329537230, -8.703598725189323045E-14, 13.71589010951911902 ) ) ;
#10117 = CARTESIAN_POINT ( 'NONE',  ( -30.26275506840322294, -57.76657404653985139, 1.198031551615709844 ) ) ;
#10118 = CARTESIAN_POINT ( 'NONE',  ( -259.2033419157646676, 9.517827891722582478, -40.00000000000002132 ) ) ;
#10119 = CARTESIAN_POINT ( 'NONE',  ( -280.0000000000000568, -42.42640687119285303, -14.14213562373118371 ) ) ;
#10120 = CARTESIAN_POINT ( 'NONE',  ( -215.0000000000000284, 60.27431767988564104, -73.32453023895048716 ) ) ;
#10121 = FACE_OUTER_BOUND ( 'NONE', #3045, .T. ) ;
#10122 = CARTESIAN_POINT ( 'NONE',  ( -86.96347745069644475, -2.438961472018186339E-13, 21.75974354311649961 ) ) ;
#10123 = CARTESIAN_POINT ( 'NONE',  ( -30.26275506840323359, -40.00000000000017053, 41.69427246844613677 ) ) ;
#10124 = CARTESIAN_POINT ( 'NONE',  ( -208.1127848780264742, 67.17687982760683951, 10.60833733268317403 ) ) ;
#10125 = CARTESIAN_POINT ( 'NONE',  ( -114.5468827412802710, 9.969911493407927594, 19.54080463289418290 ) ) ;
#10126 = CARTESIAN_POINT ( 'NONE',  ( -189.1816166312681560, -17.96744819724773734, -43.37725711903312487 ) ) ;
#10127 = CARTESIAN_POINT ( 'NONE',  ( 184.8905102610680444, 14.79361573936396113, -14.79361573936377461 ) ) ;
#10128 = VERTEX_POINT ( 'NONE', #6678 ) ;
#10129 = CARTESIAN_POINT ( 'NONE',  ( -86.96347745069644475, -43.67073346367964604, -12.89780903124457545 ) ) ;
#10130 = LINE ( 'NONE', #18374, #9750 ) ;
#10131 = CARTESIAN_POINT ( 'NONE',  ( -208.1127848780264742, -15.00245453012673202, -40.00000000000002132 ) ) ;
#10132 = CARTESIAN_POINT ( 'NONE',  ( -575.0231298121466352, 75.00000000000000000, -25.00000000000201794 ) ) ;
#10133 = CARTESIAN_POINT ( 'NONE',  ( 192.4448373802101173, -14.14213562375826605, -42.42640687116518450 ) ) ;
#10134 = CARTESIAN_POINT ( 'NONE',  ( -77.62874474886946530, 3.805079090663308516, 21.73921449504242531 ) ) ;
#10135 = VERTEX_POINT ( 'NONE', #17058 ) ;
#10136 = CARTESIAN_POINT ( 'NONE',  ( 199.9999999999999432, 17.05889967449044775, -8.389830104632190810 ) ) ;
#10137 = CARTESIAN_POINT ( 'NONE',  ( 12.01361959687196190, -24.84115733209533516, 44.88892880200814517 ) ) ;
#10138 = CARTESIAN_POINT ( 'NONE',  ( -2.557884977174613716, 23.77085849409060003, 43.43882039325016109 ) ) ;
#10139 = ORIENTED_EDGE ( 'NONE', *, *, #1162, .T. ) ;
#10140 = PRODUCT_DEFINITION ( 'UNKNOWN', '', #20659, #19251 ) ;
#10141 = ORIENTED_EDGE ( 'NONE', *, *, #22568, .F. ) ;
#10142 = CARTESIAN_POINT ( 'NONE',  ( 151.7948205124836250, -33.23291073765550863, 0.000000000000000000 ) ) ;
#10143 = CARTESIAN_POINT ( 'NONE',  ( 199.0120775374408311, -7.960707704260069129, -18.34818886981279462 ) ) ;
#10144 = DIRECTION ( 'NONE',  ( 0.000000000000000000, -1.000000000000000000, 0.000000000000000000 ) ) ;
#10145 = CARTESIAN_POINT ( 'NONE',  ( -100.7734535825088358, -16.03295912088706743, -16.03295912088710296 ) ) ;
#10146 = EDGE_CURVE ( 'NONE', #23489, #1760, #2962, .T. ) ;
#10147 = B_SPLINE_CURVE_WITH_KNOTS ( 'NONE', 3,
 ( #19823, #17817, #25829, #1609, #20324, #8205 ),
 .UNSPECIFIED., .F., .F.,
 ( 4, 2, 4 ),
 ( 0.3689590070116581799, 0.3867117631979620773, 0.4044645193949216733 ),
 .UNSPECIFIED. ) ;
#10148 = AXIS2_PLACEMENT_3D ( 'NONE', #7572, #25444, #5721 ) ;
#10149 = CARTESIAN_POINT ( 'NONE',  ( -99.31364972215654063, -8.933506367378383217, -20.48028939132497328 ) ) ;
#10150 =( BOUNDED_CURVE ( )  B_SPLINE_CURVE ( 3, ( #21951, #7441, #17429, #17681, #17553, #21817, #19304 ),
 .UNSPECIFIED., .F., .F. ) 
 B_SPLINE_CURVE_WITH_KNOTS ( ( 4, 3, 4 ),
 ( 0.007486030685209696563, 0.02316748376737270271, 0.03884893684953900223 ),
 .UNSPECIFIED. ) 
 CURVE ( )  GEOMETRIC_REPRESENTATION_ITEM ( )  RATIONAL_B_SPLINE_CURVE ( ( 0.5852718452494432011, 0.6660804010233991601, 0.8043231192735847968, 1.000000000000000000, 0.8043231192735437185, 0.6660804010233410954, 0.5852718452493922419 ) ) 
 REPRESENTATION_ITEM ( '' )  );
#10151 = CARTESIAN_POINT ( 'NONE',  ( 0.2972598230769883387, 40.00000000000017053, -14.33493731733891607 ) ) ;
#10152 = CARTESIAN_POINT ( 'NONE',  ( 98.29820294267473457, 1.310413973322231751, -20.00000000000522959 ) ) ;
#10153 = CARTESIAN_POINT ( 'NONE',  ( -639.5940242462432934, 29.29751003713100133, -27.23829469497263034 ) ) ;
#10154 = CARTESIAN_POINT ( 'NONE',  ( -200.0000000000000284, 82.50000000000008527, 52.49999999999980105 ) ) ;
#10155 = CARTESIAN_POINT ( 'NONE',  ( 199.0228608363770206, 1.289830063590766907, 19.96444201077071057 ) ) ;
#10156 = CARTESIAN_POINT ( 'NONE',  ( -186.5449016017332440, 41.81559155949143758, 17.32058514259380289 ) ) ;
#10157 = CARTESIAN_POINT ( 'NONE',  ( 9.006212071498026717, -24.85331907610667912, -44.90541342374617528 ) ) ;
#10158 = CARTESIAN_POINT ( 'NONE',  ( 192.4448373802100889, -14.14213562370293431, -14.14213562370322030 ) ) ;
#10159 = CARTESIAN_POINT ( 'NONE',  ( -105.2054292635175585, 5.571723593410010660E-14, -21.49321519473983955 ) ) ;
#10160 = CARTESIAN_POINT ( 'NONE',  ( 0.2972598230770153171, -66.70487387989861361, 10.13633138497438324 ) ) ;
#10161 = DIRECTION ( 'NONE',  ( 0.000000000000000000, 1.000000000000000000, 0.000000000000000000 ) ) ;
#10162 = CARTESIAN_POINT ( 'NONE',  ( -198.0356074513804572, -10.87444709759714634, -10.87444709759729911 ) ) ;
#10163 = CARTESIAN_POINT ( 'NONE',  ( -238.4067589809705794, -0.9644942799826263791, 40.00000000000002132 ) ) ;
#10164 = CARTESIAN_POINT ( 'NONE',  ( -198.0356074513804572, 10.87444709759730088, -10.87444709759707173 ) ) ;
#10165 = CARTESIAN_POINT ( 'NONE',  ( 200.0000000000000000, -19.99999999999988631, -40.00000000000002132 ) ) ;
#10166 = CARTESIAN_POINT ( 'NONE',  ( -114.4364955367320107, 8.644468109212716911, 20.04994829327460337 ) ) ;
#10167 = CARTESIAN_POINT ( 'NONE',  ( 170.2234770963711128, 39.99999999999980105, 24.55285855007229401 ) ) ;
#10168 = CARTESIAN_POINT ( 'NONE',  ( 130.8568914410475088, 4.207082182989741348, -52.36146031193420924 ) ) ;
#10169 = CARTESIAN_POINT ( 'NONE',  ( -208.1127848780264742, 15.00245453012665742, -40.00000000000002132 ) ) ;
#10170 = ORIENTED_EDGE ( 'NONE', *, *, #26073, .T. ) ;
#10171 = ORIENTED_EDGE ( 'NONE', *, *, #11409, .T. ) ;
#10172 = CARTESIAN_POINT ( 'NONE',  ( -280.0000000000000000, -20.00000000000006750, 0.000000000000000000 ) ) ;
#10173 = CIRCLE ( 'NONE', #20378, 20.53474504356812247 ) ;
#10174 = CARTESIAN_POINT ( 'NONE',  ( -97.72675010090193837, -8.185591577777252326, -20.89622088363372399 ) ) ;
#10175 = CARTESIAN_POINT ( 'NONE',  ( -259.2033419157646676, -1.564921101325656229E-13, 30.48217210827739621 ) ) ;
#10176 = CARTESIAN_POINT ( 'NONE',  ( -105.3755690713226727, 12.89780903124418998, -12.89780903124389155 ) ) ;
#10177 = CARTESIAN_POINT ( 'NONE',  ( -213.1075012329537230, 13.71589010951907994, 0.000000000000000000 ) ) ;
#10178 = CARTESIAN_POINT ( 'NONE',  ( 184.8905102610680444, -20.92133201514440799, 0.000000000000000000 ) ) ;
#10179 = DIRECTION ( 'NONE',  ( -1.000000000000000000, 1.018913292508929218E-14, 0.000000000000000000 ) ) ;
#10180 = CARTESIAN_POINT ( 'NONE',  ( 199.9999999999998579, 17.78360892267977178, 6.705045715290576247 ) ) ;
#10181 = CARTESIAN_POINT ( 'NONE',  ( 199.9999999999999716, -17.44173617362904949, 7.567414129180135340 ) ) ;
#10182 = CARTESIAN_POINT ( 'NONE',  ( 0.2972598230769907257, 66.70487387989869887, -10.13633138497392494 ) ) ;
#10183 = CARTESIAN_POINT ( 'NONE',  ( -162.0762913951021176, -29.48230308784793152, 27.08623940707591515 ) ) ;
#10184 = DIRECTION ( 'NONE',  ( 1.000000000000000000, 1.836970198721030427E-16, -0.000000000000000000 ) ) ;
#10185 = CARTESIAN_POINT ( 'NONE',  ( -86.96347745069644475, -2.438961472018186339E-13, 21.75974354311649961 ) ) ;
#10186 = CARTESIAN_POINT ( 'NONE',  ( -198.0356074513804572, -39.15871834505931304, 17.40982414986437377 ) ) ;
#10187 = CARTESIAN_POINT ( 'NONE',  ( 19.06497207195980792, 10.03556273973447155, -10.03556273973422286 ) ) ;
#10188 = CARTESIAN_POINT ( 'NONE',  ( 136.1360204305621266, -24.77266263493151044, 24.77266263493093135 ) ) ;
#10189 = CARTESIAN_POINT ( 'NONE',  ( -105.3755690713226585, -12.89780903124383471, -43.67073346367985920 ) ) ;
#10190 = CARTESIAN_POINT ( 'NONE',  ( 199.0199705922642295, 7.656373194246554270, 18.47861116135505100 ) ) ;
#10191 = AXIS2_PLACEMENT_3D ( 'NONE', #21611, #24239, #1890 ) ;
#10193 = CARTESIAN_POINT ( 'NONE',  ( 14.38125909742181818, -1.924622159709266762E-13, 55.17850393972636880 ) ) ;
#10192 = CARTESIAN_POINT ( 'NONE',  ( -86.96347745069644475, 12.89780903124419353, -12.89780903124389333 ) ) ;
#10194 = CARTESIAN_POINT ( 'NONE',  ( 14.38125909742180397, 67.30136555898270956, -10.73282306405792319 ) ) ;
#10195 = CARTESIAN_POINT ( 'NONE',  ( 22.57783252600447454, 43.22748647439907899, -17.90541116499352015 ) ) ;
#10196 = CARTESIAN_POINT ( 'NONE',  ( 192.4448373802101173, 19.99999999996065014, -40.00000000000002132 ) ) ;
#10197 = ORIENTED_EDGE ( 'NONE', *, *, #6969, .F. ) ;
#10198 = CARTESIAN_POINT ( 'NONE',  ( -56.48582580120559271, -6.472252184284187138, -6.472252184284199572 ) ) ;
#10199 = B_SPLINE_CURVE_WITH_KNOTS ( 'NONE', 3,
 ( #1583, #24057, #17926, #21933, #5693, #13798, #20202, #18061 ),
 .UNSPECIFIED., .F., .F.,
 ( 4, 2, 2, 4 ),
 ( -5.298247996646543873E-05, 0.001923793760049340336, 0.003900570000065146144, 0.007854122480096750389 ),
 .UNSPECIFIED. ) ;
#10200 = CARTESIAN_POINT ( 'NONE',  ( -5.152948516943984814, -42.67688069069014745, 23.23217004669189123 ) ) ;
#10201 = APPLICATION_CONTEXT ( 'automotive_design' ) ;
#10202 = CARTESIAN_POINT ( 'NONE',  ( -238.4067589809705794, 40.96449427998256709, 2.449293598294708485E-15 ) ) ;
#10203 = ORIENTED_EDGE ( 'NONE', *, *, #388, .F. ) ;
#10204 = CARTESIAN_POINT ( 'NONE',  ( 160.9163046357249129, -125.7889608577475400, 55.61140153332248559 ) ) ;
#10205 = CARTESIAN_POINT ( 'NONE',  ( 199.9999999999998863, -18.99932777274695539, 0.6272729670678898195 ) ) ;
#10206 = CARTESIAN_POINT ( 'NONE',  ( 22.37977766478752883, -13.85469381972563241, 47.17011059970548104 ) ) ;
#10207 = EDGE_CURVE ( 'NONE', #19805, #4513, #13528, .T. ) ;
#10208 = CARTESIAN_POINT ( 'NONE',  ( -3.838270362648607659, 17.89317813950102831, -43.19795333834863982 ) ) ;
#10209 = CARTESIAN_POINT ( 'NONE',  ( 199.0127284201194300, -9.139505923766694906, -17.79079187713806220 ) ) ;
#10210 = DIRECTION ( 'NONE',  ( -1.000000000000000000, -1.836970198721030181E-16, -0.000000000000000000 ) ) ;
#10211 = DIRECTION ( 'NONE',  ( 0.000000000000000000, 1.000000000000000000, 0.000000000000000000 ) ) ;
#10212 = CARTESIAN_POINT ( 'NONE',  ( 19.06497207195981147, -4.605042221739098431E-14, 14.19242893257840521 ) ) ;
#10213 = CARTESIAN_POINT ( 'NONE',  ( -30.26275506840323715, 29.48230279907829754, -29.48230279907758344 ) ) ;
#10214 = CARTESIAN_POINT ( 'NONE',  ( -678.9461782662789346, 75.00000000000000000, -24.99999999999826628 ) ) ;
#10216 = CARTESIAN_POINT ( 'NONE',  ( -280.0000000000000568, 14.14213562373038968, 42.42640687119305198 ) ) ;
#10215 = CARTESIAN_POINT ( 'NONE',  ( -188.3120606736016214, 23.45204117844427572, -43.00889065702882874 ) ) ;
#10217 = DIRECTION ( 'NONE',  ( 0.000000000000000000, 0.000000000000000000, 1.000000000000000000 ) ) ;
#10218 = CARTESIAN_POINT ( 'NONE',  ( -105.3755690713226727, -18.24025645688354302, -2.449293598294708485E-15 ) ) ;
#10219 = CARTESIAN_POINT ( 'NONE',  ( -238.4067589809705794, 40.96449428006337001, -40.00000000000002132 ) ) ;
#10220 = CARTESIAN_POINT ( 'NONE',  ( 184.8905102610680444, -39.99999999999978684, -19.07866798485600768 ) ) ;
#10221 = CARTESIAN_POINT ( 'NONE',  ( -56.48582580120559982, -6.472252184284282173, 50.09629031063965243 ) ) ;
#10222 = DIRECTION ( 'NONE',  ( 1.000000000000000000, 0.000000000000000000, -0.000000000000000000 ) ) ;
#10223 = CARTESIAN_POINT ( 'NONE',  ( -56.48582580120558561, 6.472252184284607246, -50.09629031063960269 ) ) ;
#10224 = EDGE_LOOP ( 'NONE', ( #15900, #15458, #19615, #7345, #13183, #125, #7996 ) ) ;
#10225 = CARTESIAN_POINT ( 'NONE',  ( -56.48582580120559271, -6.472252184284187138, -6.472252184284199572 ) ) ;
#10226 = CARTESIAN_POINT ( 'NONE',  ( -103.9663809734695405, 8.026122151187262688, 20.15238534352856803 ) ) ;
#10227 = EDGE_LOOP ( 'NONE', ( #23795, #14393, #15586, #21944, #11309 ) ) ;
#10228 = VERTEX_POINT ( 'NONE', #15057 ) ;
#10229 = CARTESIAN_POINT ( 'NONE',  ( -238.4067589809705794, -28.96627169325313389, -27.60227080167074831 ) ) ;
#10230 = CARTESIAN_POINT ( 'NONE',  ( 21.80484139881942696, -43.42703366220392525, -17.98806631651325816 ) ) ;
#10231 = VERTEX_POINT ( 'NONE', #8683 ) ;
#10232 = CARTESIAN_POINT ( 'NONE',  ( -105.3755690713226727, -21.75974354311652093, 0.000000000000000000 ) ) ;
#10233 = CARTESIAN_POINT ( 'NONE',  ( -86.95456283525173546, -9.640367918722454021, -19.12038226852981992 ) ) ;
#10234 = ORIENTED_EDGE ( 'NONE', *, *, #8006, .F. ) ;
#10235 = B_SPLINE_CURVE_WITH_KNOTS ( 'NONE', 3,
 ( #17555, #15683, #21436, #21562, #11191, #23808, #11563, #13195, #17683, #15309, #25825, #21690 ),
 .UNSPECIFIED., .F., .F.,
 ( 4, 2, 2, 2, 2, 4 ),
 ( -5.998499568646490758E-08, 0.003531500499830293825, 0.007063060984656273529, 0.01412618195430823814, 0.02118930292396020362, 0.02825242389361216910 ),
 .UNSPECIFIED. ) ;
#10236 = CARTESIAN_POINT ( 'NONE',  ( 200.0000000000000284, 17.23849352212496910, 7.999418879479941680 ) ) ;
#10237 = DIRECTION ( 'NONE',  ( 0.000000000000000000, -1.000000000000000000, 0.000000000000000000 ) ) ;
#10238 = CARTESIAN_POINT ( 'NONE',  ( -91.56559293963834989, 12.25131212657490209, -44.31723036834897300 ) ) ;
#10239 = CARTESIAN_POINT ( 'NONE',  ( -144.0562696875023789, -31.27040355047325093, -10.50947022297233246 ) ) ;
#10240 = CARTESIAN_POINT ( 'NONE',  ( 200.0000000000000000, -39.99999999999991473, -20.00000000000024514 ) ) ;
#10241 = CARTESIAN_POINT ( 'NONE',  ( 170.2234770963711128, -24.55285855007183926, 0.000000000000000000 ) ) ;
#10242 = CARTESIAN_POINT ( 'NONE',  ( -280.0000000000000568, -14.14213562373049449, -42.42640687119305198 ) ) ;
#10243 = DIRECTION ( 'NONE',  ( 0.000000000000000000, -1.000000000000000000, 0.000000000000000000 ) ) ;
#10244 = VECTOR ( 'NONE', #24109, 1000.000000000000000 ) ;
#10245 = CIRCLE ( 'NONE', #16183, 29.99999999999999645 ) ;
#10246 = CARTESIAN_POINT ( 'NONE',  ( -135.8532207217289738, -40.00000000000001421, -9.153146818113709671 ) ) ;
#10247 = CARTESIAN_POINT ( 'NONE',  ( -198.0356074513804572, -2.321818583541004323E-13, 55.37879056873073580 ) ) ;
#10248 = VECTOR ( 'NONE', #25961, 1000.000000000000000 ) ;
#10249 = CARTESIAN_POINT ( 'NONE',  ( -86.96347745069645896, 40.00000000000008527, -21.75974354311636461 ) ) ;
#10250 = CARTESIAN_POINT ( 'NONE',  ( 0.2972598230769983307, -14.33493731733933352, 0.000000000000000000 ) ) ;
#10251 = CARTESIAN_POINT ( 'NONE',  ( 184.8905102610680444, -41.77492675555986779, -14.79361573936407304 ) ) ;
#10252 = CARTESIAN_POINT ( 'NONE',  ( 57.59792236341147031, 2.435789363418171760, 0.000000000000000000 ) ) ;
#10253 = CARTESIAN_POINT ( 'NONE',  ( -91.56559293963834989, 16.03295912088683650, 40.53558337403684675 ) ) ;
#10254 = FACE_BOUND ( 'NONE', #13840, .T. ) ;
#10255 = CARTESIAN_POINT ( 'NONE',  ( 14.32711937312301487, -49.08922911798406830, 14.14294248749828498 ) ) ;
#10256 = CARTESIAN_POINT ( 'NONE',  ( -105.3755690713226727, 1.741486606973311632E-13, -18.24025645688352881 ) ) ;
#10257 = CARTESIAN_POINT ( 'NONE',  ( 146.6084372240433993, 5.715592784339989804E-15, 5.374981219216972583 ) ) ;
#10258 = CARTESIAN_POINT ( 'NONE',  ( 163.1118516004056573, 37.29075403953160617, -19.27778845539222985 ) ) ;
#10259 = CARTESIAN_POINT ( 'NONE',  ( 170.2234770963711128, -10.92277846919235529, 45.64576402573175073 ) ) ;
#10260 = CARTESIAN_POINT ( 'NONE',  ( -188.9266751785335146, -17.94050871568824235, -43.31221945728833589 ) ) ;
#10261 = CARTESIAN_POINT ( 'NONE',  ( 0.2972598230770027716, -38.42060263243656237, -18.14793986248737667 ) ) ;
#10262 = ORIENTED_EDGE ( 'NONE', *, *, #3297, .T. ) ;
#10263 = CARTESIAN_POINT ( 'NONE',  ( -259.2033419157646676, -35.01439189186523748, -21.55415060305881170 ) ) ;
#10264 = CARTESIAN_POINT ( 'NONE',  ( -266.9101291198153376, 0.000000000000000000, 0.000000000000000000 ) ) ;
#10265 = CARTESIAN_POINT ( 'NONE',  ( 91.82158438592158234, 17.20528682183301683, 0.000000000000000000 ) ) ;
#10266 = CARTESIAN_POINT ( 'NONE',  ( 73.43374839994166337, 12.96823619005579964, 26.88865971589134318 ) ) ;
#10267 = CARTESIAN_POINT ( 'NONE',  ( 184.8905102610680444, -14.79361573936399665, 14.79361573936367158 ) ) ;
#10268 =( LENGTH_UNIT ( ) NAMED_UNIT ( * ) SI_UNIT ( .MILLI., .METRE. ) );
#10269 = ORIENTED_EDGE ( 'NONE', *, *, #18324, .F. ) ;
#10270 = ORIENTED_EDGE ( 'NONE', *, *, #1025, .T. ) ;
#10271 = VECTOR ( 'NONE', #7566, 1000.000000000000000 ) ;
#10272 = CARTESIAN_POINT ( 'NONE',  ( 199.9999999999999432, 9.226325135675029543, 16.62006860685476184 ) ) ;
#10273 = CARTESIAN_POINT ( 'NONE',  ( 21.98945382326331810, -23.63684424402667261, 43.25809532770878008 ) ) ;
#10274 = CARTESIAN_POINT ( 'NONE',  ( 5.823571940223595256, 24.75780943189298355, 44.77584346942381188 ) ) ;
#10275 = ORIENTED_EDGE ( 'NONE', *, *, #18243, .T. ) ;
#10276 = ORIENTED_EDGE ( 'NONE', *, *, #13214, .F. ) ;
#10277 = LINE ( 'NONE', #24114, #9815 ) ;
#10278 = CARTESIAN_POINT ( 'NONE',  ( 199.0073291892102247, 3.255542347464756681, -19.72957075196997323 ) ) ;
#10279 = CARTESIAN_POINT ( 'NONE',  ( -348.0000000000001137, -4.504554366608264653E-14, -28.79780246617542616 ) ) ;
#10280 = CARTESIAN_POINT ( 'NONE',  ( 4.995406935893289102, 10.78321810388998081, 10.78321810389001811 ) ) ;
#10281 = CARTESIAN_POINT ( 'NONE',  ( 23.37394308801976806, 42.85717664514618264, -23.33966569535049373 ) ) ;
#10282 = CARTESIAN_POINT ( 'NONE',  ( 192.4448373802101173, 40.00000000000026290, -19.99999999996018474 ) ) ;
#10283 = DIRECTION ( 'NONE',  ( -5.098616525425841937E-32, 2.775557561562890858E-16, 1.000000000000000000 ) ) ;
#10284 = CARTESIAN_POINT ( 'NONE',  ( -138.9613198120178765, 29.42718893709621142, -10.11110880661601996 ) ) ;
#10285 = VECTOR ( 'NONE', #732, 1000.000000000000000 ) ;
#10286 = DIRECTION ( 'NONE',  ( 1.000000000000000000, 1.836970198721030181E-16, 0.000000000000000000 ) ) ;
#10287 = CARTESIAN_POINT ( 'NONE',  ( 199.0210534451952924, 5.480999013853959489, 19.23967134089702569 ) ) ;
#10288 = CARTESIAN_POINT ( 'NONE',  ( -121.8425418803964817, 9.420907392434369143, 22.74408238734170595 ) ) ;
#10289 = CARTESIAN_POINT ( 'NONE',  ( 16.10036699873721489, -24.53427828609593675, -44.47262139758191779 ) ) ;
#10290 = CARTESIAN_POINT ( 'NONE',  ( -135.8532207217289738, -21.81201906317757633, -21.81201906317793515 ) ) ;
#10291 = ADVANCED_FACE ( 'NONE', ( #441, #5092, #23186, #20931, #25316, #11072 ), #10543, .F. ) ;
#10292 = CARTESIAN_POINT ( 'NONE',  ( -105.2054292634647936, 1.359558446572939561, -21.49321519475378750 ) ) ;
#10293 = CARTESIAN_POINT ( 'NONE',  ( -192.9588430854690273, -66.79921049724377724, 10.23066800231950069 ) ) ;
#10294 = CARTESIAN_POINT ( 'NONE',  ( -575.0231298121445889, 75.00000000000000000, 29.99999999999825206 ) ) ;
#10295 = CARTESIAN_POINT ( 'NONE',  ( 170.2234770963711128, 24.55285855007190321, 0.000000000000000000 ) ) ;
#10296 = CARTESIAN_POINT ( 'NONE',  ( 136.1360204305621551, -4.966164525587043244, 40.00000000000002132 ) ) ;
#10297 = EDGE_CURVE ( 'NONE', #12655, #7180, #7222, .T. ) ;
#10298 = CARTESIAN_POINT ( 'NONE',  ( -678.9461782662789346, 90.00000000000000000, -34.99999999999845812 ) ) ;
#10299 = CARTESIAN_POINT ( 'NONE',  ( 0.2972598230770130412, -54.33493731733936016, -2.449293598294708485E-15 ) ) ;
#10300 = CARTESIAN_POINT ( 'NONE',  ( -105.3366978519447059, 10.59928388867598237, 18.59727947899841993 ) ) ;
#10301 = CARTESIAN_POINT ( 'NONE',  ( -198.0356074513804572, 40.00000000000056843, -55.37879056871282302 ) ) ;
#10302 = EDGE_CURVE ( 'NONE', #11184, #14253, #2566, .T. ) ;
#10303 = CARTESIAN_POINT ( 'NONE',  ( -135.8532207217289738, 21.81201906317777883, -34.75652343174605363 ) ) ;
#10304 = ADVANCED_FACE ( 'NONE', ( #12669 ), #20797, .T. ) ;
#10305 = CARTESIAN_POINT ( 'NONE',  ( -56.48582580120559271, -9.153146818113595984, 0.000000000000000000 ) ) ;
#10306 = ORIENTED_EDGE ( 'NONE', *, *, #18007, .F. ) ;
#10307 = VERTEX_POINT ( 'NONE', #18795 ) ;
#10308 = CARTESIAN_POINT ( 'NONE',  ( -162.0762913951021176, 1.694272876828294194, 40.00000000000002132 ) ) ;
#10309 = AXIS2_PLACEMENT_3D ( 'NONE', #9598, #7092, #1370 ) ;
#10310 = CARTESIAN_POINT ( 'NONE',  ( 170.0000000000000000, -21.59613885783082665, -12.70659020859102739 ) ) ;
#10311 = CARTESIAN_POINT ( 'NONE',  ( -162.0762913951021176, 57.76657433523994456, -1.198031840315424867 ) ) ;
#10312 = CARTESIAN_POINT ( 'NONE',  ( 199.9999999999999432, -20.00000000000006750, 0.000000000000000000 ) ) ;
#10313 = CARTESIAN_POINT ( 'NONE',  ( 170.2234770963711128, -24.55285855007183926, 0.000000000000000000 ) ) ;
#10314 = CARTESIAN_POINT ( 'NONE',  ( -200.0000000000000000, 71.50000000000009948, 66.50000000000005684 ) ) ;
#10315 = CARTESIAN_POINT ( 'NONE',  ( 200.0000000000001137, 18.27430636540404407, -5.205727087885991367 ) ) ;
#10316 = CARTESIAN_POINT ( 'NONE',  ( 199.9999999999999716, -16.47313602895343365, 9.508414938895898061 ) ) ;
#10317 = CARTESIAN_POINT ( 'NONE',  ( 14.38125909742181108, 39.01709431150961649, -39.01709431150867147 ) ) ;
#10318 = CARTESIAN_POINT ( 'NONE',  ( 192.4448373802101173, -42.42640687116510634, 14.14213562375845257 ) ) ;
#10319 = DIRECTION ( 'NONE',  ( -1.000000000000000000, -1.836970198721030181E-16, -1.232595164407830946E-32 ) ) ;
#10320 = CARTESIAN_POINT ( 'NONE',  ( -208.1127848780264742, 40.00000000000014211, -15.00245453012627728 ) ) ;
#10321 = CARTESIAN_POINT ( 'NONE',  ( 200.0000000000000000, -42.42640687119290988, 14.14213562373064903 ) ) ;
#10322 = CARTESIAN_POINT ( 'NONE',  ( -87.13361725327074225, 15.19799821270847850, -15.19799821270833284 ) ) ;
#10323 = CARTESIAN_POINT ( 'NONE',  ( 146.6084372240433993, -24.48358557860319706, -24.48358557860330720 ) ) ;
#10324 = CARTESIAN_POINT ( 'NONE',  ( 4.995406935893297984, -39.06748935135182421, -17.50105314357212549 ) ) ;
#10325 = CARTESIAN_POINT ( 'NONE',  ( 199.0254843815459651, -7.164921656906469316, 18.67865466993989898 ) ) ;
#10327 = CARTESIAN_POINT ( 'NONE',  ( -208.1127848780264742, 39.99999999999979394, 55.00245453010936103 ) ) ;
#10326 = CARTESIAN_POINT ( 'NONE',  ( -162.0762913951020892, 29.48230308784799902, -29.48230308784730980 ) ) ;
#10328 = CARTESIAN_POINT ( 'NONE',  ( -280.0000000000000568, 42.42640687119265408, 14.14213562373147504 ) ) ;
#10329 = CARTESIAN_POINT ( 'NONE',  ( 23.26364522860089323, 46.84987168986916117, -13.80713620122723917 ) ) ;
#10330 = CARTESIAN_POINT ( 'NONE',  ( -192.9588430854690273, 14.46834944099966336, -40.00000000000002132 ) ) ;
#10331 = CARTESIAN_POINT ( 'NONE',  ( 98.29820294267527458, 2.689882573189819553E-13, -20.00000000000500222 ) ) ;
#10332 = CARTESIAN_POINT ( 'NONE',  ( -3.494657986427672114, -43.29048295385651812, 17.93150516116827120 ) ) ;
#10333 = CARTESIAN_POINT ( 'NONE',  ( -259.2033419157646676, 30.48217210827734647, 2.449293598294708485E-15 ) ) ;
#10334 = ORIENTED_EDGE ( 'NONE', *, *, #23713, .T. ) ;
#10335 = CARTESIAN_POINT ( 'NONE',  ( -626.9846540392142060, 75.00000000000000000, -60.00000000000000000 ) ) ;
#10336 = CARTESIAN_POINT ( 'NONE',  ( -77.55640685876518603, 15.64922766773203122, 15.64922766773211471 ) ) ;
#10337 = CARTESIAN_POINT ( 'NONE',  ( -4.660840668352994598, -13.78427145221255934, 46.77528141313064225 ) ) ;
#10338 = CARTESIAN_POINT ( 'NONE',  ( 2.332272417556594313, 24.49123061636224463, -44.41409500754982531 ) ) ;
#10339 = CARTESIAN_POINT ( 'NONE',  ( 199.0095093599360894, -2.612260778589423182, -19.82812366214328748 ) ) ;
#10340 = CARTESIAN_POINT ( 'NONE',  ( -259.2033419157646676, -1.473088368616265084E-13, 9.517827891722632216 ) ) ;
#10341 = CARTESIAN_POINT ( 'NONE',  ( 190.0000000000000000, -66.50000000000001421, -66.50000000000005684 ) ) ;
#10342 = CARTESIAN_POINT ( 'NONE',  ( -187.3037411061906425, -23.25513534570069041, 42.71163782367113271 ) ) ;
#10343 = CARTESIAN_POINT ( 'NONE',  ( -238.4067589809705794, -27.60227080167029001, -28.96627169325357798 ) ) ;
#10344 = CARTESIAN_POINT ( 'NONE',  ( 136.1360204305621266, 35.03383547441298873, 0.000000000000000000 ) ) ;
#10346 = CARTESIAN_POINT ( 'NONE',  ( 136.1360204305621551, 3.511608612530062512, 53.05693388239318864 ) ) ;
#10345 = CARTESIAN_POINT ( 'NONE',  ( -194.4222169613859421, 14.07715596672279545, -48.65437996130461329 ) ) ;
#10347 = CARTESIAN_POINT ( 'NONE',  ( 163.1118516004056573, 9.006482792073693844, 47.56205970284970164 ) ) ;
#10348 = CARTESIAN_POINT ( 'NONE',  ( -192.9588430854690273, -54.46834944098226572, 40.00000000000002132 ) ) ;
#10349 = CARTESIAN_POINT ( 'NONE',  ( -135.8532207217289738, 30.84685318188643421, 40.00000000000002132 ) ) ;
#10350 = CARTESIAN_POINT ( 'NONE',  ( 192.4448373802101173, -40.00000000000019185, 20.00000000003900524 ) ) ;
#10351 = CARTESIAN_POINT ( 'NONE',  ( 146.6084372240433993, 3.800685668858676980, 3.800685668858667210 ) ) ;
#10352 = CARTESIAN_POINT ( 'NONE',  ( -97.73806390045244541, 20.71810467719082283, -8.581719943944259299 ) ) ;
#10353 = CARTESIAN_POINT ( 'NONE',  ( 4.995406935893305977, -39.06748935135157552, -39.06748935135225764 ) ) ;
#10354 = ORIENTED_EDGE ( 'NONE', *, *, #15991, .F. ) ;
#10355 = CARTESIAN_POINT ( 'NONE',  ( 14.38125909742180752, 10.73282306404720465, 10.73282306404724018 ) ) ;
#10356 = LINE ( 'NONE', #2117, #20571 ) ;
#10357 = CONTEXT_DEPENDENT_SHAPE_REPRESENTATION ( #3923, #6573 ) ;
#10358 = ADVANCED_FACE ( 'NONE', ( #576 ), #22924, .T. ) ;
#10359 = CARTESIAN_POINT ( 'NONE',  ( 14.38125909742181996, -10.73282306403606157, 67.30136555895948902 ) ) ;
#10360 = CARTESIAN_POINT ( 'NONE',  ( 6.202588567996038194, -49.19971320597203146, -14.15973318135109871 ) ) ;
#10361 = ORIENTED_EDGE ( 'NONE', *, *, #13860, .F. ) ;
#10362 = CARTESIAN_POINT ( 'NONE',  ( 4.990270234119186021, -49.14367003637712372, -14.15117691407198741 ) ) ;
#10363 = DIRECTION ( 'NONE',  ( 1.000000000000000000, 1.836970198721030181E-16, 0.000000000000000000 ) ) ;
#10364 = ORIENTED_EDGE ( 'NONE', *, *, #4933, .F. ) ;
#10365 = CARTESIAN_POINT ( 'NONE',  ( 200.0000000000002842, 4.912815075579886503, -18.35721014059308942 ) ) ;
#10366 = DIRECTION ( 'NONE',  ( 0.3301743741175477975, 0.9439199556509468847, 0.000000000000000000 ) ) ;
#10367 = CARTESIAN_POINT ( 'NONE',  ( 163.1118516004056573, 9.006482792074356425, -47.56205970284957374 ) ) ;
#10368 = CARTESIAN_POINT ( 'NONE',  ( -189.1816166312713960, -43.37725711903439674, -17.96744819724840880 ) ) ;
#10369 = B_SPLINE_CURVE_WITH_KNOTS ( 'NONE', 3,
 ( #7626, #17872, #26023, #13750, #3935, #17610 ),
 .UNSPECIFIED., .F., .F.,
 ( 4, 2, 4 ),
 ( -5.998621906354538341E-08, 0.03938016914544736902, 0.07876039827711379948 ),
 .UNSPECIFIED. ) ;
#10370 = CARTESIAN_POINT ( 'NONE',  ( 163.1118516004056573, -40.00000000000003553, 12.73709011382460687 ) ) ;
#10371 = CARTESIAN_POINT ( 'NONE',  ( 192.4448373802100889, 19.99999999996064304, 2.449293598294708485E-15 ) ) ;
#10372 = CARTESIAN_POINT ( 'NONE',  ( 192.4448373802101173, -42.42640687122053578, -14.14213562370360577 ) ) ;
#10373 = CARTESIAN_POINT ( 'NONE',  ( 199.0258313909553749, -8.851116586292111066, 17.94317422212728630 ) ) ;
#10374 = CARTESIAN_POINT ( 'NONE',  ( -208.1127848780264742, -40.00000000000011369, 15.00245453012655439 ) ) ;
#10375 = CARTESIAN_POINT ( 'NONE',  ( -259.2033419157646676, 39.99999999999987210, 30.48217210827754542 ) ) ;
#10376 = CARTESIAN_POINT ( 'NONE',  ( -192.9588430854690273, 39.99999999999992895, 14.46834944099983922 ) ) ;
#10377 = CARTESIAN_POINT ( 'NONE',  ( 19.06497207195981503, -14.19242893257840166, 0.000000000000000000 ) ) ;
#10378 = CARTESIAN_POINT ( 'NONE',  ( -86.96347745069644475, -18.24025645688354302, -2.449293598294708485E-15 ) ) ;
#10379 = EDGE_CURVE ( 'NONE', #4560, #7864, #4662, .T. ) ;
#10380 = CARTESIAN_POINT ( 'NONE',  ( 199.9999999999999432, -14.14213562373093680, 14.14213562373082311 ) ) ;
#10381 = CARTESIAN_POINT ( 'NONE',  ( 159.7744820660625180, -10.75261058663746816, -25.95909830917691608 ) ) ;
#10382 = CARTESIAN_POINT ( 'NONE',  ( 23.37394308801977871, -46.80823611210205115, 13.80096434448272724 ) ) ;
#10383 = CARTESIAN_POINT ( 'NONE',  ( 91.82158438592156813, 40.00000000000027711, -22.79471317813428044 ) ) ;
#10384 = CARTESIAN_POINT ( 'NONE',  ( -30.26275506840323359, -1.535832457777009877E-13, 41.69427246844629309 ) ) ;
#10385 = CARTESIAN_POINT ( 'NONE',  ( -259.2033419157646676, 49.83842185052027673, -6.730120644403441155 ) ) ;
#10386 = CARTESIAN_POINT ( 'NONE',  ( -200.0000000000000000, 69.99999999999995737, 8.572527594031465104E-15 ) ) ;
#10387 = DIRECTION ( 'NONE',  ( 0.000000000000000000, -0.3028247695821862928, 0.9530462522498558409 ) ) ;
#10388 = CARTESIAN_POINT ( 'NONE',  ( 151.7948205124836534, -33.06932595376343897, -23.49921654116042902 ) ) ;
#10389 = EDGE_LOOP ( 'NONE', ( #561, #12002, #19449, #4233 ) ) ;
#10390 = CARTESIAN_POINT ( 'NONE',  ( -192.9588430854689989, 10.23066800230756712, -10.23066800230735396 ) ) ;
#10391 = CARTESIAN_POINT ( 'NONE',  ( 141.7948666911895259, 30.38861427224637879, -12.58737617328896086 ) ) ;
#10392 = CARTESIAN_POINT ( 'NONE',  ( -162.0762913951020892, -41.69427287672991866, -40.00000000000002132 ) ) ;
#10393 = CARTESIAN_POINT ( 'NONE',  ( -114.7756899093962062, 16.59394837944376988, -14.65087933325889225 ) ) ;
#10394 = EDGE_LOOP ( 'NONE', ( #13153, #19009, #23266, #5263 ) ) ;
#10395 = ORIENTED_EDGE ( 'NONE', *, *, #20727, .F. ) ;
#10396 = CARTESIAN_POINT ( 'NONE',  ( 199.9999999999999432, 14.88226939975712604, 11.82339673543941494 ) ) ;
#10397 = CARTESIAN_POINT ( 'NONE',  ( -83.21262154144254453, 33.12752917118434226, -13.72187187061452107 ) ) ;
#10398 = CARTESIAN_POINT ( 'NONE',  ( 9.028290303185817933, 18.59346688787791635, 44.88859993222893507 ) ) ;
#10399 = EDGE_LOOP ( 'NONE', ( #17360, #16816, #26219, #13058 ) ) ;
#10400 = ORIENTED_EDGE ( 'NONE', *, *, #3611, .T. ) ;
#10401 = PRODUCT ( 'Stator', 'Stator', '', ( #20079 ) ) ;
#10402 = CARTESIAN_POINT ( 'NONE',  ( 170.2234770963711128, -24.55285855007184281, -40.00000000000002132 ) ) ;
#10403 = CARTESIAN_POINT ( 'NONE',  ( 199.0117582043400830, -7.359043231587310885, -18.59750019459799120 ) ) ;
#10404 = CARTESIAN_POINT ( 'NONE',  ( -105.4741150117389594, 7.943527260764311926, 19.77569912954495024 ) ) ;
#10405 = CARTESIAN_POINT ( 'NONE',  ( -135.8532207217289738, 50.09629031063965243, -6.472252184284084109 ) ) ;
#10406 = DIRECTION ( 'NONE',  ( -1.000000000000000000, 0.000000000000000000, 0.000000000000000000 ) ) ;
#10407 = CARTESIAN_POINT ( 'NONE',  ( -103.9650464693342826, -8.298274097555776052, -20.03380587592332773 ) ) ;
#10408 = CARTESIAN_POINT ( 'NONE',  ( 146.6084372240433993, 8.568076647504290689E-14, -5.374981219216972583 ) ) ;
#10409 = CARTESIAN_POINT ( 'NONE',  ( -198.0356074513804572, 40.00000000000014921, -15.37879056873028816 ) ) ;
#10410 = CARTESIAN_POINT ( 'NONE',  ( -656.8721355146591350, 39.91566430679986865, -2.646366307133875218 ) ) ;
#10411 = SPHERICAL_SURFACE ( 'NONE', #25140, 15.00000000000000000 ) ;
#10412 = CARTESIAN_POINT ( 'NONE',  ( 199.0056892241198625, 17.33029760820262410, -9.978133259584877734 ) ) ;
#10413 = CARTESIAN_POINT ( 'NONE',  ( -189.1815713358150788, 17.96744347545610410, 43.37724571961807385 ) ) ;
#10414 = CARTESIAN_POINT ( 'NONE',  ( -100.7734535825088500, -12.25131212657524316, 44.31723036834888774 ) ) ;
#10415 = CARTESIAN_POINT ( 'NONE',  ( -114.4364955367314991, -8.644468109207263495, -20.04994829327655737 ) ) ;
#10416 = CARTESIAN_POINT ( 'NONE',  ( 4.995406935893287326, 17.50105314357170627, 39.06748935135200895 ) ) ;
#10417 = CARTESIAN_POINT ( 'NONE',  ( -77.78697283798739193, 6.810146944752746734, 20.89074004980727395 ) ) ;
#10418 = VECTOR ( 'NONE', #23747, 1000.000000000000000 ) ;
#10419 = CARTESIAN_POINT ( 'NONE',  ( 192.4448373802101173, 42.42640687122089815, -14.14213562370272470 ) ) ;
#10420 = CARTESIAN_POINT ( 'NONE',  ( -631.7966154096428681, 28.60212811815375034, 34.74874185832601370 ) ) ;
#10421 = CARTESIAN_POINT ( 'NONE',  ( 14.38125909742181285, -15.17850393972633505, 40.00000000000002132 ) ) ;
#10422 = CARTESIAN_POINT ( 'NONE',  ( -91.56559293963834989, -16.03295912088728414, 16.03295912088688269 ) ) ;
#10423 = CARTESIAN_POINT ( 'NONE',  ( -198.0356074513804572, -15.37879056873074290, 40.00000000000002132 ) ) ;
#10424 = CARTESIAN_POINT ( 'NONE',  ( -110.0947816603262908, 15.91249765680895045, 12.43490089449757185 ) ) ;
#10425 = CARTESIAN_POINT ( 'NONE',  ( -280.0000000000000568, 40.00000000000017764, -19.99999999999959144 ) ) ;
#10426 = CARTESIAN_POINT ( 'NONE',  ( -208.1127848780264742, 38.89260858015732936, -17.67593391476642140 ) ) ;
#10427 = CARTESIAN_POINT ( 'NONE',  ( 135.5356265174576436, -12.51227922893921196, 30.20731421070332345 ) ) ;
#10428 = B_SPLINE_CURVE_WITH_KNOTS ( 'NONE', 3,
 ( #663, #16886, #4798, #21653, #17395, #25534 ),
 .UNSPECIFIED., .F., .F.,
 ( 4, 2, 4 ),
 ( 0.000000000000000000, 0.004519108751124900972, 0.009038217502249801943 ),
 .UNSPECIFIED. ) ;
#10429 = VERTEX_POINT ( 'NONE', #9200 ) ;
#10430 = ORIENTED_EDGE ( 'NONE', *, *, #16051, .T. ) ;
#10431 = ORIENTED_EDGE ( 'NONE', *, *, #20307, .T. ) ;
#10432 = CARTESIAN_POINT ( 'NONE',  ( -198.0356074513804572, 15.37879056873066830, 40.00000000000002132 ) ) ;
#10433 = CIRCLE ( 'NONE', #21889, 39.99999999999997158 ) ;
#10434 = ADVANCED_FACE ( 'NONE', ( #19685 ), #10630, .F. ) ;
#10435 = CIRCLE ( 'NONE', #9161, 39.99999999999991473 ) ;
#10436 = CARTESIAN_POINT ( 'NONE',  ( 136.1360204305621551, 31.79587985999232558, 24.77266263493161702 ) ) ;
#10437 = CARTESIAN_POINT ( 'NONE',  ( -105.2958943010001605, -20.90688085069862723, -4.721182065470063804 ) ) ;
#10438 = EDGE_CURVE ( 'NONE', #21905, #25993, #25964, .T. ) ;
#10439 = CARTESIAN_POINT ( 'NONE',  ( -200.0000000000000000, -55.16984130227027094, 4.865628651907646152 ) ) ;
#10440 = CARTESIAN_POINT ( 'NONE',  ( -86.86493150571111244, 7.943527260496201947, -19.77569912839169319 ) ) ;
#10441 = CARTESIAN_POINT ( 'NONE',  ( 200.0000000000000568, 2.630809070280605511, -18.81871160794394982 ) ) ;
#10442 = EDGE_CURVE ( 'NONE', #5421, #14022, #21823, .T. ) ;
#10443 = EDGE_CURVE ( 'NONE', #24345, #3139, #7319, .T. ) ;
#10444 = VECTOR ( 'NONE', #7904, 1000.000000000000000 ) ;
#10445 = CARTESIAN_POINT ( 'NONE',  ( 199.9999999999999147, 11.06273067492490547, -15.45041022988906931 ) ) ;
#10446 = VECTOR ( 'NONE', #15432, 1000.000000000000227 ) ;
#10447 = CARTESIAN_POINT ( 'NONE',  ( -198.0356074513804572, 10.87444709759730088, -10.87444709759707173 ) ) ;
#10448 = CARTESIAN_POINT ( 'NONE',  ( 19.06497207195981858, -38.31983398719641087, 18.24870850772724040 ) ) ;
#10449 = CARTESIAN_POINT ( 'NONE',  ( -370.0000000000001137, 20.53474504356807273, 0.000000000000000000 ) ) ;
#10450 = CARTESIAN_POINT ( 'NONE',  ( 199.9999999999999432, -1.727494763561684666E-13, 20.00000000000010303 ) ) ;
#10451 = CARTESIAN_POINT ( 'NONE',  ( -162.0762913951020607, -57.76657433537922515, -1.198031840455874963 ) ) ;
#10452 = CARTESIAN_POINT ( 'NONE',  ( 1.564252679174723770, 14.06374044400962120, 48.56509332159242831 ) ) ;
#10453 = CARTESIAN_POINT ( 'NONE',  ( 130.8568914410475372, -24.07718906447255947, 24.07718906447199458 ) ) ;
#10454 = CARTESIAN_POINT ( 'NONE',  ( -86.96347745069643054, -41.18208027870589660, -15.38646221621809040 ) ) ;
#10455 = DIRECTION ( 'NONE',  ( 0.000000000000000000, 1.000000000000000000, 0.000000000000000000 ) ) ;
#10457 = CARTESIAN_POINT ( 'NONE',  ( -86.96347745069645896, 39.99999999999994316, 18.24025645688366737 ) ) ;
#10456 = CARTESIAN_POINT ( 'NONE',  ( 151.7948205124836534, 33.06932595376333239, 23.49921654116065284 ) ) ;
#10458 = CARTESIAN_POINT ( 'NONE',  ( -86.96347745069644475, 12.89780903124349898, 43.67073346367994446 ) ) ;
#10459 = VECTOR ( 'NONE', #1994, 1000.000000000000000 ) ;
#10460 = CARTESIAN_POINT ( 'NONE',  ( 25.62979979002535202, 45.99287499161375337, -13.63460241473574897 ) ) ;
#10461 = CARTESIAN_POINT ( 'NONE',  ( 199.9999999999999432, 19.99999999999996092, 2.449293598294708485E-15 ) ) ;
#10462 = CARTESIAN_POINT ( 'NONE',  ( -213.1075012329537230, 9.698598906450410340, 9.698598906450483170 ) ) ;
#10463 = CARTESIAN_POINT ( 'NONE',  ( -4.039451493210483690, -23.44932283416618191, -43.00522595894033628 ) ) ;
#10464 =( BOUNDED_CURVE ( )  B_SPLINE_CURVE ( 3, ( #5463, #25828, #1221, #9325 ),
 .UNSPECIFIED., .F., .F. ) 
 B_SPLINE_CURVE_WITH_KNOTS ( ( 4, 4 ),
 ( 0.007858036080414859334, 0.01577215542394082640 ),
 .UNSPECIFIED. ) 
 CURVE ( )  GEOMETRIC_REPRESENTATION_ITEM ( )  RATIONAL_B_SPLINE_CURVE ( ( 0.5857864376268567819, 0.5560595459730498513, 0.5340584217468483663, 0.5197830649482524379 ) ) 
 REPRESENTATION_ITEM ( '' )  );
#10465 = CARTESIAN_POINT ( 'NONE',  ( -3.615356597027800767, -43.25798660799100759, 17.91804473398356023 ) ) ;
#10466 = CARTESIAN_POINT ( 'NONE',  ( 146.6084372240433709, -34.62501878078303008, 40.00000000000002132 ) ) ;
#10467 = CONICAL_SURFACE ( 'NONE', #9607, 20.53474504356812247, 0.7853981633974447263 ) ;
#10468 = ORIENTED_EDGE ( 'NONE', *, *, #25887, .F. ) ;
#10469 = CARTESIAN_POINT ( 'NONE',  ( 14.33519843538172189, 24.71012982060745955, -44.71104701565624140 ) ) ;
#10470 = CARTESIAN_POINT ( 'NONE',  ( 14.38125909742180752, 10.73282306404720465, 10.73282306404724018 ) ) ;
#10471 = CARTESIAN_POINT ( 'NONE',  ( -7.726389047727614034, -17.45517700520998972, 42.14052505957891981 ) ) ;
#10472 = CARTESIAN_POINT ( 'NONE',  ( -0.6848998192527971929, 24.09453515735949480, -43.87669161505412774 ) ) ;
#10473 = CARTESIAN_POINT ( 'NONE',  ( 199.0099327931564233, -3.581876008808642098, -19.67427284064525139 ) ) ;
#10474 = CIRCLE ( 'NONE', #13836, 5.000000000000004441 ) ;
#10475 = EDGE_CURVE ( 'NONE', #15838, #18515, #11700, .T. ) ;
#10476 = DIRECTION ( 'NONE',  ( -1.000000000000000000, -1.836970198721030181E-16, 0.000000000000000000 ) ) ;
#10477 = CARTESIAN_POINT ( 'NONE',  ( -189.6939645179850515, -18.01965094556746649, 43.50328570201445189 ) ) ;
#10478 = CARTESIAN_POINT ( 'NONE',  ( -192.9588430854690273, -18.05360324515400094, -38.51493924976961836 ) ) ;
#10479 = CARTESIAN_POINT ( 'NONE',  ( -87.13361725327072804, -21.49321519333431141, -3.542586001259484843E-15 ) ) ;
#10481 = CARTESIAN_POINT ( 'NONE',  ( 170.2234770963711128, 10.92277846919147066, 45.64576402573197811 ) ) ;
#10480 = CARTESIAN_POINT ( 'NONE',  ( -197.4153392276936358, 24.72549520225541286, -44.73189834455630631 ) ) ;
#10482 = CARTESIAN_POINT ( 'NONE',  ( 91.82158438592158234, -12.16597498397778843, 12.16597498397750954 ) ) ;
#10483 = CARTESIAN_POINT ( 'NONE',  ( 0.2972598230770129857, -54.33493731733936016, -40.00000000000002132 ) ) ;
#10484 = CARTESIAN_POINT ( 'NONE',  ( 19.06497207195980792, 54.19242893257843718, 2.449293598294708485E-15 ) ) ;
#10485 = CARTESIAN_POINT ( 'NONE',  ( 57.59792236341147031, -1.493297263419786540E-14, 2.435789363418160658 ) ) ;
#10486 = CARTESIAN_POINT ( 'NONE',  ( -86.96347745069644475, 12.89780903124401057, 12.89780903124407629 ) ) ;
#10487 = AXIS2_PLACEMENT_3D ( 'NONE', #13158, #3049, #25659 ) ;
#10488 = CARTESIAN_POINT ( 'NONE',  ( -88.37877758187934774, 19.92653024472395273, -8.575405934686655129 ) ) ;
#10489 = CARTESIAN_POINT ( 'NONE',  ( -208.1127848780264742, -10.60833733270725787, -67.17687982763172272 ) ) ;
#10490 = CARTESIAN_POINT ( 'NONE',  ( 19.06497207195980792, 18.24870850772737185, 38.31983398719634692 ) ) ;
#10491 = ORIENTED_EDGE ( 'NONE', *, *, #10586, .T. ) ;
#10492 = CARTESIAN_POINT ( 'NONE',  ( -192.9588430854689989, 10.23066800230742679, 10.23066800230749607 ) ) ;
#10493 = CARTESIAN_POINT ( 'NONE',  ( -86.86493150570990451, 8.366608963953497735, 19.60045294882744216 ) ) ;
#10494 = CARTESIAN_POINT ( 'NONE',  ( 163.1118516004056573, 19.27778845539212327, 37.29075403953164169 ) ) ;
#10495 = CARTESIAN_POINT ( 'NONE',  ( 20.16956056503174466, -47.86583268169049177, -13.95858718338156734 ) ) ;
#10496 = VERTEX_POINT ( 'NONE', #1608 ) ;
#10497 = DIRECTION ( 'NONE',  ( 1.000000000000000000, 0.000000000000000000, 0.000000000000000000 ) ) ;
#10498 = FACE_OUTER_BOUND ( 'NONE', #24249, .T. ) ;
#10499 = ORIENTED_EDGE ( 'NONE', *, *, #17902, .F. ) ;
#10500 = CARTESIAN_POINT ( 'NONE',  ( 199.9999999999997726, 3.400090818600995934, -18.69490476363523612 ) ) ;
#10501 = DIRECTION ( 'NONE',  ( -1.000000000000000000, -0.000000000000000000, -0.000000000000000000 ) ) ;
#10502 = CARTESIAN_POINT ( 'NONE',  ( -188.9524938556191955, -47.22059665006131013, -13.86227398173359759 ) ) ;
#10503 = VECTOR ( 'NONE', #2601, 1000.000000000000000 ) ;
#10504 = CARTESIAN_POINT ( 'NONE',  ( -30.26275506840323359, -1.535832457777009877E-13, 41.69427246844629309 ) ) ;
#10505 = CARTESIAN_POINT ( 'NONE',  ( -30.26275506840324425, 41.69427246844628598, -40.00000000000002132 ) ) ;
#10506 = CARTESIAN_POINT ( 'NONE',  ( -100.7734535825088358, -16.03295912088728770, 16.03295912088687913 ) ) ;
#10507 = CARTESIAN_POINT ( 'NONE',  ( 199.0246859915949642, -4.071254240408448410, 19.58630271169732140 ) ) ;
#10508 = CARTESIAN_POINT ( 'NONE',  ( -213.1075012329537230, -2.291445344039133686E-13, 53.71589010951915100 ) ) ;
#10509 = CARTESIAN_POINT ( 'NONE',  ( 0.2972598230769956662, 39.99999999999983658, 54.33493731733950938 ) ) ;
#10510 = LINE ( 'NONE', #24623, #14254 ) ;
#10511 = CARTESIAN_POINT ( 'NONE',  ( -30.26275506840324070, -1.694272468446265112, 0.000000000000000000 ) ) ;
#10512 = CARTESIAN_POINT ( 'NONE',  ( -192.9588430854690273, -54.46834944098226572, 40.00000000000002132 ) ) ;
#10513 = CARTESIAN_POINT ( 'NONE',  ( -30.26275506840323359, -1.198031551616339341, 57.76657404653985139 ) ) ;
#10514 = CARTESIAN_POINT ( 'NONE',  ( 169.9999999999999716, -9.369682556672181306, -22.62041470344887273 ) ) ;
#10515 = DIRECTION ( 'NONE',  ( 0.000000000000000000, 0.000000000000000000, 1.000000000000000000 ) ) ;
#10516 = CARTESIAN_POINT ( 'NONE',  ( 130.8568914410475088, 40.00000000000011369, -5.949712681206269949 ) ) ;
#10517 = CARTESIAN_POINT ( 'NONE',  ( -192.9588430854690273, 39.99999999999980105, 54.46834944098235809 ) ) ;
#10518 = CARTESIAN_POINT ( 'NONE',  ( 199.0260893535204048, -10.43036187021208860, 17.07141274968551059 ) ) ;
#10519 = CARTESIAN_POINT ( 'NONE',  ( 23.37394308801977871, -23.33966569535098046, 42.85717664514577763 ) ) ;
#10520 = CARTESIAN_POINT ( 'NONE',  ( 23.37394308801977161, 13.80096434448334186, -46.80823611210181667 ) ) ;
#10521 = CARTESIAN_POINT ( 'NONE',  ( -198.0356074513804288, -39.15871834505936278, 39.15871834505892224 ) ) ;
#10522 = EDGE_LOOP ( 'NONE', ( #11062, #12001, #18006, #14214 ) ) ;
#10523 = CARTESIAN_POINT ( 'NONE',  ( -5.152948516936860734, 46.60473671797380746, -13.74948675458147740 ) ) ;
#10524 = CARTESIAN_POINT ( 'NONE',  ( 110.0479209278586126, 22.74092928740055441, -9.419601331808626909 ) ) ;
#10525 = CARTESIAN_POINT ( 'NONE',  ( -208.1127848780264742, -55.00245453014425578, -40.00000000000002132 ) ) ;
#10526 = CARTESIAN_POINT ( 'NONE',  ( 169.9999999999999716, -9.369682556672181306, -22.62041470344887273 ) ) ;
#10527 = FACE_OUTER_BOUND ( 'NONE', #3085, .T. ) ;
#10528 =( NAMED_UNIT ( * ) PLANE_ANGLE_UNIT ( ) SI_UNIT ( $, .RADIAN. ) );
#10529 = ORIENTED_EDGE ( 'NONE', *, *, #12384, .F. ) ;
#10530 = ORIENTED_EDGE ( 'NONE', *, *, #8145, .F. ) ;
#10531 = CARTESIAN_POINT ( 'NONE',  ( 199.9999999999999147, -10.44179787682348781, 15.88662230291588706 ) ) ;
#10532 = CARTESIAN_POINT ( 'NONE',  ( -103.9650464692780218, 8.298274099701076878, -20.03380587474480379 ) ) ;
#10533 = CARTESIAN_POINT ( 'NONE',  ( 16.10036699856469156, 24.53427828609990513, 44.47262139759975241 ) ) ;
#10534 = B_SPLINE_CURVE_WITH_KNOTS ( 'NONE', 3,
 ( #12761, #14487, #20886, #10906, #22880, #8502, #22749, #14881, #6368, #4917, #24749, #16489 ),
 .UNSPECIFIED., .F., .F.,
 ( 4, 2, 2, 2, 2, 4 ),
 ( -5.998499568707339487E-08, 0.003531500499830289921, 0.007063060984656267458, 0.01412618195430823294, 0.02118930292396019321, 0.02825242389361215523 ),
 .UNSPECIFIED. ) ;
#10535 = ORIENTED_EDGE ( 'NONE', *, *, #12719, .F. ) ;
#10536 = ORIENTED_EDGE ( 'NONE', *, *, #21363, .F. ) ;
#10537 = CARTESIAN_POINT ( 'NONE',  ( -198.0356074513804572, 10.87444709758468875, 67.44298959250869530 ) ) ;
#10538 = CARTESIAN_POINT ( 'NONE',  ( 199.0166470710653925, -15.03895783737594805, -13.18902814565699266 ) ) ;
#10539 = DIRECTION ( 'NONE',  ( -1.000000000000000000, 0.000000000000000000, 0.000000000000000000 ) ) ;
#10540 = CARTESIAN_POINT ( 'NONE',  ( -208.1127848780265026, 10.60833733269537049, 10.60833733269544510 ) ) ;
#10541 = CARTESIAN_POINT ( 'NONE',  ( 163.1118516004056573, 37.29075403953160617, -19.27778845539222985 ) ) ;
#10542 = LINE ( 'NONE', #25058, #26192 ) ;
#10543 = PLANE ( 'NONE',  #16951 ) ;
#10544 = EDGE_CURVE ( 'NONE', #1596, #17045, #17408, .T. ) ;
#10545 = CARTESIAN_POINT ( 'NONE',  ( 19.06497207195980792, 40.00000000000059686, -54.19242893257802507 ) ) ;
#10546 = CARTESIAN_POINT ( 'NONE',  ( -280.0000000000000568, 40.00000000000017764, -19.99999999999959144 ) ) ;
#10547 = CARTESIAN_POINT ( 'NONE',  ( -636.9543983739517898, 28.22693517060480772, 28.36072991200662941 ) ) ;
#10548 = CARTESIAN_POINT ( 'NONE',  ( 180.0000000000000000, 6.980486755139914804E-14, 0.000000000000000000 ) ) ;
#10549 = CARTESIAN_POINT ( 'NONE',  ( 199.0070393743141892, 19.55016766319115007, -4.199986046643529924 ) ) ;
#10550 = CARTESIAN_POINT ( 'NONE',  ( -188.2506440019886327, 23.43978047293197164, 42.99080317017340747 ) ) ;
#10551 = CARTESIAN_POINT ( 'NONE',  ( -135.8532207217289738, 6.472252184284096543, 6.472252184284234211 ) ) ;
#10552 = CARTESIAN_POINT ( 'NONE',  ( -105.3844635032202461, 6.703103239450354245, -20.33704783843148434 ) ) ;
#10553 = CARTESIAN_POINT ( 'NONE',  ( -213.1075012329537230, -9.698598906438496314, 66.26714140136188291 ) ) ;
#10554 = CARTESIAN_POINT ( 'NONE',  ( -77.55640685876510076, 0.6996548653659642181, 22.13135000837105082 ) ) ;
#10555 = CARTESIAN_POINT ( 'NONE',  ( -91.56559293963836410, 44.31723036834908669, -12.25131212657445801 ) ) ;
#10556 = CARTESIAN_POINT ( 'NONE',  ( -200.0000000000000568, 46.38610861938607144, -18.14877749763654080 ) ) ;
#10557 = CARTESIAN_POINT ( 'NONE',  ( 136.1360204305621266, 35.03383547441298873, 0.000000000000000000 ) ) ;
#10558 = CARTESIAN_POINT ( 'NONE',  ( 200.0000000000000000, 14.14213562373041455, 42.42640687119311593 ) ) ;
#10559 = CARTESIAN_POINT ( 'NONE',  ( -192.9588430854689989, -14.46834944099973086, 0.000000000000000000 ) ) ;
#10560 = CARTESIAN_POINT ( 'NONE',  ( -594.0003854396136376, 43.45006682348635252, -11.76540767128717846 ) ) ;
#10561 = CARTESIAN_POINT ( 'NONE',  ( -30.26275506840323359, 4.336144384597734078E-13, -41.69427246844629309 ) ) ;
#10562 = CARTESIAN_POINT ( 'NONE',  ( 199.0142503478488720, -11.66167433960233168, -16.26558534365442910 ) ) ;
#10563 = CARTESIAN_POINT ( 'NONE',  ( 167.0466155511619775, -9.710058186602013919, 23.44215416552578901 ) ) ;
#10564 = EDGE_LOOP ( 'NONE', ( #13065, #4415, #10662, #21240 ) ) ;
#10565 = ORIENTED_EDGE ( 'NONE', *, *, #1189, .F. ) ;
#10566 = CARTESIAN_POINT ( 'NONE',  ( 163.1118516004056573, -27.26290988616869626, 0.000000000000000000 ) ) ;
#10567 = DIRECTION ( 'NONE',  ( 0.000000000000000000, 1.000000000000000000, 0.000000000000000000 ) ) ;
#10568 = VECTOR ( 'NONE', #18182, 1000.000000000000000 ) ;
#10569 =( BOUNDED_SURFACE ( )  B_SPLINE_SURFACE ( 3, 3, ( 
 ( #9920, #1552, #21513, #3285, #23631, #17761, #9789, #15892, #24020, #11917, #20167, #8450, #18163, #16033, #12441, #14308, #24158, #16569, #2215, #14570, #1949, #22700, #4083, #12577, #18432, #6071, #10056, #24566, #16169, #6195 ),
 ( #14042, #20569, #5935, #18293, #4475, #22176, #4220, #20707, #18699, #10189, #79, #2342, #12184, #20305, #6321, #22442, #10324, #14442, #22306, #24700, #14173, #8189, #12047, #2473, #7915, #208, #3950, #12310, #8317, #18567 ),
 ( #10583, #24304, #16305, #26309, #8052, #346, #2082, #24429, #20437, #16440, #22571, #4349, #10454, #6455, #18836, #14705, #882, #4613, #23357, #8992, #25228, #20969, #12709, #615, #14833, #23229, #11234, #15226, #13239, #18971 ),
 ( #20837, #22838, #6852, #2612, #24832, #17222, #10725, #1008, #8721, #8589, #5007, #14969, #16700, #9111, #21102, #7115, #16839, #5134, #22965, #21364, #10990, #24972, #6721, #17096, #4745, #3131, #2749, #6981, #12851, #6585 ),
 ( #751, #10853, #16967, #483, #25103, #8855, #23104, #4876, #12979, #19099, #2882, #15096, #13112, #21233, #3006, #11114, #19228, #25361, #17352, #5256, #9763, #11614, #7751, #17476, #26014, #25488, #11751, #19736, #15862, #23991 ),
 ( #17600, #5771, #7237, #9246, #23482, #11480, #15358, #13879, #19872, #13358, #22012, #5382, #19608, #1523, #1141, #9631, #23603, #21480, #1654, #13742, #1262, #3255, #17732, #17863, #3645, #1394, #25873, #15732, #11359, #13487 ),
 ( #3783, #19352, #7617, #7364, #23858, #19476, #9495, #21608, #9366, #15602, #3382, #25618, #15476, #25741, #13610, #7491, #23727, #5508, #21738, #3514, #5635, #21868, #12023, #2189, #321, #4193, #20143, #6297, #24541, #5906 ) ),
 .UNSPECIFIED., .T., .F., .F. ) 
 B_SPLINE_SURFACE_WITH_KNOTS ( ( 4, 3, 4 ),
 ( 4, 2, 2, 2, 2, 2, 2, 2, 2, 2, 2, 2, 2, 2, 4 ),
 ( 0.000000000000000000, 0.5000000000000000000, 1.000000000000000000 ),
 ( 0.000000000000000000, 0.1357259735107005372, 0.1651108541090157700, 0.1944957347073310028, 0.3598804999793158710, 0.3867117631979620773, 0.4135430264166082281, 0.5789277916885930964, 0.6062785021374117456, 0.6336292125862302838, 0.8508620842112317728, 0.8814014469398914198, 0.9119408096685510667, 0.9559704048342755334, 1.000000000000000000 ),
 .UNSPECIFIED. ) 
 GEOMETRIC_REPRESENTATION_ITEM ( )  RATIONAL_B_SPLINE_SURFACE ( (
 ( 1.000000000000000000, 1.000000000000000000, 1.000000000000000000, 1.000000000000000000, 1.000000000000000000, 1.000000000000000000, 1.000000000000000000, 1.000000000000000000, 1.000000000000000000, 1.000000000000000000, 1.000000000000000000, 1.000000000000000000, 1.000000000000000000, 1.000000000000000000, 1.000000000000000000, 1.000000000000000000, 1.000000000000000000, 1.000000000000000000, 1.000000000000000000, 1.000000000000000000, 1.000000000000000000, 1.000000000000000000, 1.000000000000000000, 1.000000000000000000, 1.000000000000000000, 1.000000000000000000, 1.000000000000000000, 1.000000000000000000, 1.000000000000000000, 1.000000000000000000),
 ( 0.3333333333333333703, 0.3333333333333333703, 0.3333333333333333703, 0.3333333333333333703, 0.3333333333333333703, 0.3333333333333333703, 0.3333333333333333703, 0.3333333333333333703, 0.3333333333333333703, 0.3333333333333333703, 0.3333333333333333703, 0.3333333333333333703, 0.3333333333333333703, 0.3333333333333333703, 0.3333333333333333703, 0.3333333333333333703, 0.3333333333333333703, 0.3333333333333333703, 0.3333333333333333703, 0.3333333333333333703, 0.3333333333333333703, 0.3333333333333333703, 0.3333333333333333703, 0.3333333333333333703, 0.3333333333333333703, 0.3333333333333333703, 0.3333333333333333703, 0.3333333333333333703, 0.3333333333333333703, 0.3333333333333333703),
 ( 0.3333333333333333703, 0.3333333333333333703, 0.3333333333333333703, 0.3333333333333333703, 0.3333333333333333703, 0.3333333333333333703, 0.3333333333333333703, 0.3333333333333333703, 0.3333333333333333703, 0.3333333333333333703, 0.3333333333333333703, 0.3333333333333333703, 0.3333333333333333703, 0.3333333333333333703, 0.3333333333333333703, 0.3333333333333333703, 0.3333333333333333703, 0.3333333333333333703, 0.3333333333333333703, 0.3333333333333333703, 0.3333333333333333703, 0.3333333333333333703, 0.3333333333333333703, 0.3333333333333333703, 0.3333333333333333703, 0.3333333333333333703, 0.3333333333333333703, 0.3333333333333333703, 0.3333333333333333703, 0.3333333333333333703),
 ( 1.000000000000000000, 1.000000000000000000, 1.000000000000000000, 1.000000000000000000, 1.000000000000000000, 1.000000000000000000, 1.000000000000000000, 1.000000000000000000, 1.000000000000000000, 1.000000000000000000, 1.000000000000000000, 1.000000000000000000, 1.000000000000000000, 1.000000000000000000, 1.000000000000000000, 1.000000000000000000, 1.000000000000000000, 1.000000000000000000, 1.000000000000000000, 1.000000000000000000, 1.000000000000000000, 1.000000000000000000, 1.000000000000000000, 1.000000000000000000, 1.000000000000000000, 1.000000000000000000, 1.000000000000000000, 1.000000000000000000, 1.000000000000000000, 1.000000000000000000),
 ( 0.3333333333333333703, 0.3333333333333333703, 0.3333333333333333703, 0.3333333333333333703, 0.3333333333333333703, 0.3333333333333333703, 0.3333333333333333703, 0.3333333333333333703, 0.3333333333333333703, 0.3333333333333333703, 0.3333333333333333703, 0.3333333333333333703, 0.3333333333333333703, 0.3333333333333333703, 0.3333333333333333703, 0.3333333333333333703, 0.3333333333333333703, 0.3333333333333333703, 0.3333333333333333703, 0.3333333333333333703, 0.3333333333333333703, 0.3333333333333333703, 0.3333333333333333703, 0.3333333333333333703, 0.3333333333333333703, 0.3333333333333333703, 0.3333333333333333703, 0.3333333333333333703, 0.3333333333333333703, 0.3333333333333333703),
 ( 0.3333333333333333703, 0.3333333333333333703, 0.3333333333333333703, 0.3333333333333333703, 0.3333333333333333703, 0.3333333333333333703, 0.3333333333333333703, 0.3333333333333333703, 0.3333333333333333703, 0.3333333333333333703, 0.3333333333333333703, 0.3333333333333333703, 0.3333333333333333703, 0.3333333333333333703, 0.3333333333333333703, 0.3333333333333333703, 0.3333333333333333703, 0.3333333333333333703, 0.3333333333333333703, 0.3333333333333333703, 0.3333333333333333703, 0.3333333333333333703, 0.3333333333333333703, 0.3333333333333333703, 0.3333333333333333703, 0.3333333333333333703, 0.3333333333333333703, 0.3333333333333333703, 0.3333333333333333703, 0.3333333333333333703),
 ( 1.000000000000000000, 1.000000000000000000, 1.000000000000000000, 1.000000000000000000, 1.000000000000000000, 1.000000000000000000, 1.000000000000000000, 1.000000000000000000, 1.000000000000000000, 1.000000000000000000, 1.000000000000000000, 1.000000000000000000, 1.000000000000000000, 1.000000000000000000, 1.000000000000000000, 1.000000000000000000, 1.000000000000000000, 1.000000000000000000, 1.000000000000000000, 1.000000000000000000, 1.000000000000000000, 1.000000000000000000, 1.000000000000000000, 1.000000000000000000, 1.000000000000000000, 1.000000000000000000, 1.000000000000000000, 1.000000000000000000, 1.000000000000000000, 1.000000000000000000) ) ) 
 REPRESENTATION_ITEM ( '' )  SURFACE ( )  );
#10570 = CARTESIAN_POINT ( 'NONE',  ( 91.82158438592158234, 16.11829626346161604, -16.11829626346121103 ) ) ;
#10571 = CARTESIAN_POINT ( 'NONE',  ( -110.1017491837608446, -20.19444236859277098, -1.278135197240527043 ) ) ;
#10572 = CARTESIAN_POINT ( 'NONE',  ( -199.9999999999999147, -53.44529986889379103, 10.02640517461957614 ) ) ;
#10573 = LINE ( 'NONE', #8304, #5770 ) ;
#10574 = CARTESIAN_POINT ( 'NONE',  ( 199.9999999999998295, 14.29413690760092592, -12.53266873553815053 ) ) ;
#10575 = CARTESIAN_POINT ( 'NONE',  ( 199.9999999999999147, -1.558418107136771757, -18.94039843610738671 ) ) ;
#10576 = CARTESIAN_POINT ( 'NONE',  ( -91.56559293963834989, -44.31723036834885932, -12.25131212657538171 ) ) ;
#10577 = CARTESIAN_POINT ( 'NONE',  ( -208.1127848780265026, -10.60833733269537227, -10.60833733269551793 ) ) ;
#10578 = CARTESIAN_POINT ( 'NONE',  ( -114.7792487060331865, 22.11287803872790647, 1.644740498667294881 ) ) ;
#10579 = CARTESIAN_POINT ( 'NONE',  ( 146.6084372240433709, 40.00000000000010658, -5.374981219216549810 ) ) ;
#10580 = CARTESIAN_POINT ( 'NONE',  ( -94.58366989427227622, -8.190486896679354700, 20.91926462023902999 ) ) ;
#10581 = CARTESIAN_POINT ( 'NONE',  ( 170.2234770963711128, 24.55285855007190321, 0.000000000000000000 ) ) ;
#10582 = CARTESIAN_POINT ( 'NONE',  ( -56.48582580120559271, -6.472252184284187138, -6.472252184284199572 ) ) ;
#10583 = CARTESIAN_POINT ( 'NONE',  ( -280.0000000000000568, -42.42640687119285303, -14.14213562373118371 ) ) ;
#10584 = CARTESIAN_POINT ( 'NONE',  ( -100.7734535825088500, 22.67402823373189591, -0.000000000000000000 ) ) ;
#10585 = CIRCLE ( 'NONE', #19088, 15.00000000000000000 ) ;
#10586 = EDGE_CURVE ( 'NONE', #9969, #11726, #10464, .T. ) ;
#10588 = CARTESIAN_POINT ( 'NONE',  ( -30.26275506840324425, 39.99999999999987210, 41.69427246844643520 ) ) ;
#10587 = CARTESIAN_POINT ( 'NONE',  ( -105.3755690713226585, -43.67073346367964604, -12.89780903124457545 ) ) ;
#10589 = CARTESIAN_POINT ( 'NONE',  ( -135.8532207217289738, 50.09629031063956006, 6.472252184284782217 ) ) ;
#10590 = CARTESIAN_POINT ( 'NONE',  ( 22.76403192593601688, 43.17745271018617359, -17.88468650128181991 ) ) ;
#10591 = CARTESIAN_POINT ( 'NONE',  ( -100.7734535825088500, -22.67402823373193499, -40.00000000000002132 ) ) ;
#10592 = CARTESIAN_POINT ( 'NONE',  ( -105.3755690713226585, -43.67073346367983788, 12.89780903124397149 ) ) ;
#10593 = CARTESIAN_POINT ( 'NONE',  ( -100.7734535825088500, 17.32597176626808988, 40.00000000000002132 ) ) ;
#10594 = AXIS2_PLACEMENT_3D ( 'NONE', #23196, #15199, #17190 ) ;
#10595 = EDGE_CURVE ( 'NONE', #19296, #13991, #9700, .T. ) ;
#10596 = CARTESIAN_POINT ( 'NONE',  ( -4.558244102846490620, -42.85231560262746342, 23.34817229226001345 ) ) ;
#10597 = CARTESIAN_POINT ( 'NONE',  ( 170.2234770963711128, 15.44714144992818738, 40.00000000000002132 ) ) ;
#10598 = ADVANCED_FACE ( 'NONE', ( #5213 ), #15816, .T. ) ;
#10599 = ORIENTED_EDGE ( 'NONE', *, *, #1126, .F. ) ;
#10600 = CARTESIAN_POINT ( 'NONE',  ( -190.1760961843813789, -47.67020129257696937, -13.92889018389476874 ) ) ;
#10601 = CARTESIAN_POINT ( 'NONE',  ( -100.7734535825088358, -16.03295912088706743, -16.03295912088710296 ) ) ;
#10602 = CARTESIAN_POINT ( 'NONE',  ( -5.379830816902669177, -13.73345071524718897, 46.52611083736134390 ) ) ;
#10603 = CARTESIAN_POINT ( 'NONE',  ( -4.660840668352909333, 23.32816686155626584, -42.82207049670912369 ) ) ;
#10604 = CARTESIAN_POINT ( 'NONE',  ( 200.0000000000003411, -11.08347333911627963, 15.44584840147742355 ) ) ;
#10605 = CARTESIAN_POINT ( 'NONE',  ( -30.26275506840324070, 1.198031551616030033, -1.198031551616006496 ) ) ;
#10606 = CARTESIAN_POINT ( 'NONE',  ( -82.30220482034327745, 7.441767004318980305, -18.74474319042418458 ) ) ;
#10607 = CARTESIAN_POINT ( 'NONE',  ( -65.65555754753494000, -24.04429191298299884, -11.16466304451123825 ) ) ;
#10608 = CARTESIAN_POINT ( 'NONE',  ( -190.0144721487978643, -23.79987203025130071, 43.47822244619790411 ) ) ;
#10609 = FACE_OUTER_BOUND ( 'NONE', #16517, .T. ) ;
#10610 = AXIS2_PLACEMENT_3D ( 'NONE', #783, #7268, #11020 ) ;
#10611 = CARTESIAN_POINT ( 'NONE',  ( 163.1118516004056573, -19.27778845539181063, -37.29075403953176959 ) ) ;
#10612 = CARTESIAN_POINT ( 'NONE',  ( -200.0000000000000000, -66.50000000000001421, 66.50000000000005684 ) ) ;
#10614 = CARTESIAN_POINT ( 'NONE',  ( 170.2234770963711128, 10.92277846919216522, -10.92277846919186501 ) ) ;
#10613 = CARTESIAN_POINT ( 'NONE',  ( -199.0730705747853051, 18.57195860668882048, -44.83667434815284736 ) ) ;
#10615 = CARTESIAN_POINT ( 'NONE',  ( 130.8568914410475372, -24.07718906447255947, 24.07718906447199458 ) ) ;
#10616 = CARTESIAN_POINT ( 'NONE',  ( -198.0356074513804288, -55.37879056873077133, -2.449293598294708485E-15 ) ) ;
#10617 = CARTESIAN_POINT ( 'NONE',  ( 170.2234770963711128, 15.44714144992819094, 2.449293598294708485E-15 ) ) ;
#10618 = CARTESIAN_POINT ( 'NONE',  ( -280.0000000000000568, -40.00000000000028422, 19.99999999999959499 ) ) ;
#10619 = CARTESIAN_POINT ( 'NONE',  ( -135.8532207217289738, 21.81201906317777883, -34.75652343174605363 ) ) ;
#10620 = ADVANCED_FACE ( 'NONE', ( #5335 ), #21437, .F. ) ;
#10621 =( BOUNDED_SURFACE ( )  B_SPLINE_SURFACE ( 3, 3, ( 
 ( #5027, #25249, #23252, #15689, #13702, #9329, #21323, #11442, #19690, #1225, #5596, #15564, #5467, #11198, #23689, #7577, #13321, #23320, #15437, #17316, #3096, #13570, #7450, #17561, #23564, #25699, #17439, #21696, #21568, #21441 ),
 ( #9584, #23814, #7080, #3341, #3216, #21827, #25448, #3597, #19438, #19826, #25577, #7323, #11705, #19564, #5096, #5339, #13449, #1356, #9455, #7200, #1612, #3472, #1478, #11571, #17689, #19312, #13201, #11322, #25832, #9716 ),
 ( #1095, #9205, #15315, #25321, #15193, #23441, #5217, #4279, #17820, #24361, #22235, #7708, #4010, #23946, #10117, #7976, #5999, #24495, #2140, #8116, #9981, #11976, #16094, #18090, #1742, #12109, #25968, #10251, #18360, #139 ),
 ( #7836, #12369, #18218, #8243, #16361, #26241, #16232, #14233, #5724, #3874, #3735, #22373, #4149, #24225, #11838, #6256, #15960, #14105, #13828, #14369, #20497, #15819, #21961, #22500, #2640, #4, #6125, #24085, #20100, #20234 ),
 ( #1878, #2013, #19958, #9850, #17953, #12242, #20366, #26100, #5859, #13965, #22100, #21129, #13260, #9266, #18859, #21256, #14859, #13380, #15123, #21383, #23381, #10748, #904, #24994, #6875, #22993, #17247, #25513, #17374, #3155 ),
 ( #19252, #3028, #9016, #11136, #2904, #1032, #7003, #14991, #15251, #9132, #7260, #25384, #11257, #5275, #7136, #19375, #640, #4769, #12874, #23501, #1163, #16990, #17121, #2772, #6747, #21507, #11012, #25252, #5155, #10882 ),
 ( #15378, #19122, #8744, #16862, #23254, #20990, #18996, #8879, #5030, #773, #25125, #23126, #4898, #13007, #13137, #5930, #21890, #9783, #1414, #15623, #1545, #3666, #7384, #26169, #11775, #25765, #23746, #11911, #17885, #7910 ) ),
 .UNSPECIFIED., .T., .F., .F. ) 
 B_SPLINE_SURFACE_WITH_KNOTS ( ( 4, 3, 4 ),
 ( 4, 2, 2, 2, 2, 2, 2, 2, 2, 2, 2, 2, 2, 2, 4 ),
 ( 0.000000000000000000, 0.5000000000000000000, 1.000000000000000000 ),
 ( 0.000000000000000000, 0.1357259735107005372, 0.1651108541090157700, 0.1944957347073310028, 0.3598804999793158710, 0.3867117631979620773, 0.4135430264166082281, 0.5789277916885930964, 0.6062785021374117456, 0.6336292125862302838, 0.8508620842112317728, 0.8814014469398914198, 0.9119408096685510667, 0.9559704048342755334, 1.000000000000000000 ),
 .UNSPECIFIED. ) 
 GEOMETRIC_REPRESENTATION_ITEM ( )  RATIONAL_B_SPLINE_SURFACE ( (
 ( 1.000000000000000000, 1.000000000000000000, 1.000000000000000000, 1.000000000000000000, 1.000000000000000000, 1.000000000000000000, 1.000000000000000000, 1.000000000000000000, 1.000000000000000000, 1.000000000000000000, 1.000000000000000000, 1.000000000000000000, 1.000000000000000000, 1.000000000000000000, 1.000000000000000000, 1.000000000000000000, 1.000000000000000000, 1.000000000000000000, 1.000000000000000000, 1.000000000000000000, 1.000000000000000000, 1.000000000000000000, 1.000000000000000000, 1.000000000000000000, 1.000000000000000000, 1.000000000000000000, 1.000000000000000000, 1.000000000000000000, 1.000000000000000000, 1.000000000000000000),
 ( 0.3333333333333333703, 0.3333333333333333703, 0.3333333333333333703, 0.3333333333333333703, 0.3333333333333333703, 0.3333333333333333703, 0.3333333333333333703, 0.3333333333333333703, 0.3333333333333333703, 0.3333333333333333703, 0.3333333333333333703, 0.3333333333333333703, 0.3333333333333333703, 0.3333333333333333703, 0.3333333333333333703, 0.3333333333333333703, 0.3333333333333333703, 0.3333333333333333703, 0.3333333333333333703, 0.3333333333333333703, 0.3333333333333333703, 0.3333333333333333703, 0.3333333333333333703, 0.3333333333333333703, 0.3333333333333333703, 0.3333333333333333703, 0.3333333333333333703, 0.3333333333333333703, 0.3333333333333333703, 0.3333333333333333703),
 ( 0.3333333333333333703, 0.3333333333333333703, 0.3333333333333333703, 0.3333333333333333703, 0.3333333333333333703, 0.3333333333333333703, 0.3333333333333333703, 0.3333333333333333703, 0.3333333333333333703, 0.3333333333333333703, 0.3333333333333333703, 0.3333333333333333703, 0.3333333333333333703, 0.3333333333333333703, 0.3333333333333333703, 0.3333333333333333703, 0.3333333333333333703, 0.3333333333333333703, 0.3333333333333333703, 0.3333333333333333703, 0.3333333333333333703, 0.3333333333333333703, 0.3333333333333333703, 0.3333333333333333703, 0.3333333333333333703, 0.3333333333333333703, 0.3333333333333333703, 0.3333333333333333703, 0.3333333333333333703, 0.3333333333333333703),
 ( 1.000000000000000000, 1.000000000000000000, 1.000000000000000000, 1.000000000000000000, 1.000000000000000000, 1.000000000000000000, 1.000000000000000000, 1.000000000000000000, 1.000000000000000000, 1.000000000000000000, 1.000000000000000000, 1.000000000000000000, 1.000000000000000000, 1.000000000000000000, 1.000000000000000000, 1.000000000000000000, 1.000000000000000000, 1.000000000000000000, 1.000000000000000000, 1.000000000000000000, 1.000000000000000000, 1.000000000000000000, 1.000000000000000000, 1.000000000000000000, 1.000000000000000000, 1.000000000000000000, 1.000000000000000000, 1.000000000000000000, 1.000000000000000000, 1.000000000000000000),
 ( 0.3333333333333333703, 0.3333333333333333703, 0.3333333333333333703, 0.3333333333333333703, 0.3333333333333333703, 0.3333333333333333703, 0.3333333333333333703, 0.3333333333333333703, 0.3333333333333333703, 0.3333333333333333703, 0.3333333333333333703, 0.3333333333333333703, 0.3333333333333333703, 0.3333333333333333703, 0.3333333333333333703, 0.3333333333333333703, 0.3333333333333333703, 0.3333333333333333703, 0.3333333333333333703, 0.3333333333333333703, 0.3333333333333333703, 0.3333333333333333703, 0.3333333333333333703, 0.3333333333333333703, 0.3333333333333333703, 0.3333333333333333703, 0.3333333333333333703, 0.3333333333333333703, 0.3333333333333333703, 0.3333333333333333703),
 ( 0.3333333333333333703, 0.3333333333333333703, 0.3333333333333333703, 0.3333333333333333703, 0.3333333333333333703, 0.3333333333333333703, 0.3333333333333333703, 0.3333333333333333703, 0.3333333333333333703, 0.3333333333333333703, 0.3333333333333333703, 0.3333333333333333703, 0.3333333333333333703, 0.3333333333333333703, 0.3333333333333333703, 0.3333333333333333703, 0.3333333333333333703, 0.3333333333333333703, 0.3333333333333333703, 0.3333333333333333703, 0.3333333333333333703, 0.3333333333333333703, 0.3333333333333333703, 0.3333333333333333703, 0.3333333333333333703, 0.3333333333333333703, 0.3333333333333333703, 0.3333333333333333703, 0.3333333333333333703, 0.3333333333333333703),
 ( 1.000000000000000000, 1.000000000000000000, 1.000000000000000000, 1.000000000000000000, 1.000000000000000000, 1.000000000000000000, 1.000000000000000000, 1.000000000000000000, 1.000000000000000000, 1.000000000000000000, 1.000000000000000000, 1.000000000000000000, 1.000000000000000000, 1.000000000000000000, 1.000000000000000000, 1.000000000000000000, 1.000000000000000000, 1.000000000000000000, 1.000000000000000000, 1.000000000000000000, 1.000000000000000000, 1.000000000000000000, 1.000000000000000000, 1.000000000000000000, 1.000000000000000000, 1.000000000000000000, 1.000000000000000000, 1.000000000000000000, 1.000000000000000000, 1.000000000000000000) ) ) 
 REPRESENTATION_ITEM ( '' )  SURFACE ( )  );
#10622 = CARTESIAN_POINT ( 'NONE',  ( 98.29850319112431123, -7.044854747019780206, 18.72964005471164128 ) ) ;
#10623 = PRODUCT ( 'Rotor', 'Rotor', '', ( #22078 ) ) ;
#10624 = CARTESIAN_POINT ( 'NONE',  ( 146.6084372240433709, 24.48358557860356655, -32.08495691632035118 ) ) ;
#10625 = EDGE_CURVE ( 'NONE', #15670, #992, #20349, .T. ) ;
#10626 = CARTESIAN_POINT ( 'NONE',  ( -114.4944481313176823, -7.435744517473530379, 20.59122811151904031 ) ) ;
#10627 = ORIENTED_EDGE ( 'NONE', *, *, #21919, .F. ) ;
#10628 = CARTESIAN_POINT ( 'NONE',  ( -280.0000000000000568, 42.42640687119285303, -14.14213562373088351 ) ) ;
#10629 = DIRECTION ( 'NONE',  ( 1.000000000000000000, 1.303213150798907793E-16, 2.465190328815661892E-32 ) ) ;
#10630 = TOROIDAL_SURFACE ( 'NONE', #3345, 46.18033988749894547, 15.00000000000000000 ) ;
#10631 = CARTESIAN_POINT ( 'NONE',  ( 57.59792236341148453, -26.56190807104700369, 26.56190807104673723 ) ) ;
#10632 = CARTESIAN_POINT ( 'NONE',  ( 11.59303701482569338, -44.86219070952746790, -18.58252782965046279 ) ) ;
#10633 = ADVANCED_FACE ( 'NONE', ( #3592 ), #23810, .T. ) ;
#10634 = ADVANCED_FACE ( 'NONE', ( #11318 ), #22363, .T. ) ;
#10635 = EDGE_LOOP ( 'NONE', ( #988, #18785, #18471, #9063 ) ) ;
#10636 = CARTESIAN_POINT ( 'NONE',  ( 14.38125909742180752, 15.17850393972634038, 0.000000000000000000 ) ) ;
#10637 = CARTESIAN_POINT ( 'NONE',  ( -190.0000000000000000, -52.49999999999992895, -52.49999999999999289 ) ) ;
#10638 = MECHANICAL_DESIGN_GEOMETRIC_PRESENTATION_REPRESENTATION (  '', ( #18274 ), #8 ) ;
#10639 = ORIENTED_EDGE ( 'NONE', *, *, #10042, .F. ) ;
#10640 = CARTESIAN_POINT ( 'NONE',  ( 200.0000000000002842, 11.06692676694369304, -15.45668394874709506 ) ) ;
#10641 = CARTESIAN_POINT ( 'NONE',  ( -114.7756899093957799, -22.09342955265395858, 1.373957298914630032 ) ) ;
#10642 = CARTESIAN_POINT ( 'NONE',  ( -91.56559293963834989, 17.32597176626809343, 2.449293598294708485E-15 ) ) ;
#10643 = CARTESIAN_POINT ( 'NONE',  ( -213.1075012329537230, -18.58567234101102272, -37.98287015391260013 ) ) ;
#10644 = CARTESIAN_POINT ( 'NONE',  ( 199.0087145623001277, 19.98798542585446469, 0.6659850717246563745 ) ) ;
#10645 = CARTESIAN_POINT ( 'NONE',  ( -30.26275506840322294, -57.76657404653985139, -1.198031551616531853 ) ) ;
#10646 = CARTESIAN_POINT ( 'NONE',  ( 146.6084372240433993, 5.715592784339989804E-15, 5.374981219216972583 ) ) ;
#10647 = CARTESIAN_POINT ( 'NONE',  ( 57.59792236341147031, 39.99999999999990763, 37.56421063658199699 ) ) ;
#10648 = DIRECTION ( 'NONE',  ( 0.000000000000000000, 0.6739498806388345420, 0.7387770694782699321 ) ) ;
#10649 = FACE_OUTER_BOUND ( 'NONE', #4914, .T. ) ;
#10650 = CARTESIAN_POINT ( 'NONE',  ( -198.0356074513804572, -10.87444709759729911, 10.87444709759714812 ) ) ;
#10651 = CARTESIAN_POINT ( 'NONE',  ( -198.0356074513804288, -55.37879056873077133, -2.449293598294708485E-15 ) ) ;
#10652 = CARTESIAN_POINT ( 'NONE',  ( -100.7734535825088358, -12.25131212657493052, 12.25131212657478130 ) ) ;
#10653 = CARTESIAN_POINT ( 'NONE',  ( -162.0762913951020892, -1.202636532414034422E-14, -1.694272876828323948 ) ) ;
#10654 = VECTOR ( 'NONE', #12805, 1000.000000000000000 ) ;
#10655 = CARTESIAN_POINT ( 'NONE',  ( -105.2055636156081277, 14.22328983909173061, -16.17146666062084037 ) ) ;
#10656 = CARTESIAN_POINT ( 'NONE',  ( 163.1118516004056573, 40.00000000000017764, -12.73709011382432976 ) ) ;
#10657 = CARTESIAN_POINT ( 'NONE',  ( -198.0356074513804572, -40.00000000000025580, 55.37879056871310013 ) ) ;
#10658 = CARTESIAN_POINT ( 'NONE',  ( 130.8568914410475372, -24.07718906447222551, -24.07718906447233209 ) ) ;
#10659 = CARTESIAN_POINT ( 'NONE',  ( 180.0000000000000000, 4.582242954935206147E-14, 82.49999999999997158 ) ) ;
#10660 = DIRECTION ( 'NONE',  ( 1.937599346585394162E-16, 1.000000000000000000, 0.000000000000000000 ) ) ;
#10661 = CARTESIAN_POINT ( 'NONE',  ( -135.8532207217289738, -50.09629031063965243, -6.472252184284438492 ) ) ;
#10662 = ORIENTED_EDGE ( 'NONE', *, *, #11501, .F. ) ;
#10663 = CARTESIAN_POINT ( 'NONE',  ( -196.0240701155047702, 24.63338802315957565, -44.60678452943314198 ) ) ;
#10664 = DIRECTION ( 'NONE',  ( 0.000000000000000000, -1.000000000000000000, 0.000000000000000000 ) ) ;
#10665 = CARTESIAN_POINT ( 'NONE',  ( 146.6084372240433709, 34.62501878078307982, -40.00000000000002132 ) ) ;
#10666 = CARTESIAN_POINT ( 'NONE',  ( -114.7827960788991959, 16.12461489703415651, -15.17504536826869987 ) ) ;
#10667 = CARTESIAN_POINT ( 'NONE',  ( -135.8532207217289738, -6.472252184284280396, 6.472252184284099208 ) ) ;
#10668 = VERTEX_POINT ( 'NONE', #23907 ) ;
#10669 = ORIENTED_EDGE ( 'NONE', *, *, #3298, .T. ) ;
#10670 = CARTESIAN_POINT ( 'NONE',  ( 200.0000000000000000, -13.44239485489230290, 13.44239485489200803 ) ) ;
#10671 = CARTESIAN_POINT ( 'NONE',  ( 127.8236149080042310, 11.91256696755868205, -28.75948073575747443 ) ) ;
#10672 = CARTESIAN_POINT ( 'NONE',  ( 8.209392600923674621, 14.17653494426514804, 49.31072049264779622 ) ) ;
#10673 = ORIENTED_EDGE ( 'NONE', *, *, #16393, .T. ) ;
#10674 = ORIENTED_EDGE ( 'NONE', *, *, #22495, .T. ) ;
#10675 = CARTESIAN_POINT ( 'NONE',  ( 57.59792236341147031, -30.00663442387700641, 26.56190807104681895 ) ) ;
#10676 = CARTESIAN_POINT ( 'NONE',  ( 199.0174211633917878, -15.97280307358279039, -12.03849830368706009 ) ) ;
#10677 = CARTESIAN_POINT ( 'NONE',  ( -114.7538884076128340, -2.777513412055030884, 21.97380054627827306 ) ) ;
#10678 = CARTESIAN_POINT ( 'NONE',  ( 184.8905102610680444, -43.07788698682576722, 13.49065550809799063 ) ) ;
#10679 = CIRCLE ( 'NONE', #14057, 14.99999999999999822 ) ;
#10680 = AXIS2_PLACEMENT_3D ( 'NONE', #6129, #14111, #4014 ) ;
#10681 = CARTESIAN_POINT ( 'NONE',  ( -315.0000000000000568, 20.53474504356807273, 0.000000000000000000 ) ) ;
#10682 = CARTESIAN_POINT ( 'NONE',  ( 184.8905102610680444, 40.00000000000013500, -20.92133201514430141 ) ) ;
#10683 = SPHERICAL_SURFACE ( 'NONE', #16017, 15.00000000000000000 ) ;
#10684 = DIRECTION ( 'NONE',  ( 0.000000000000000000, 0.000000000000000000, 1.000000000000000000 ) ) ;
#10685 = CARTESIAN_POINT ( 'NONE',  ( 184.8905102610680444, 40.00000000000025580, -19.07866798485515503 ) ) ;
#10686 = CARTESIAN_POINT ( 'NONE',  ( 19.06497207195979726, 40.00000000000017053, -14.19242893257798599 ) ) ;
#10687 = DIRECTION ( 'NONE',  ( 1.000000000000000000, 1.303213150798907793E-16, 2.465190328815661892E-32 ) ) ;
#10688 = DIRECTION ( 'NONE',  ( 1.000000000000000000, 0.000000000000000000, 0.000000000000000000 ) ) ;
#10689 = CARTESIAN_POINT ( 'NONE',  ( 199.0124915487878923, 17.99959093953023270, 8.716253503037693307 ) ) ;
#10690 = CARTESIAN_POINT ( 'NONE',  ( -188.4701769959791022, 23.48627020870861770, 43.05504096897863064 ) ) ;
#10691 = CARTESIAN_POINT ( 'NONE',  ( 136.1360204305621266, 24.77266263493104148, 24.77266263493145004 ) ) ;
#10692 = CARTESIAN_POINT ( 'NONE',  ( -77.90255099906769942, -20.04994828523962269, 8.644468104261498809 ) ) ;
#10693 = CARTESIAN_POINT ( 'NONE',  ( 192.4448373802100889, -14.14213562370313682, 14.14213562370301958 ) ) ;
#10694 = CARTESIAN_POINT ( 'NONE',  ( -200.0000000000000000, -66.50000000000001421, 66.50000000000005684 ) ) ;
#10695 = AXIS2_PLACEMENT_3D ( 'NONE', #23053, #8938, #14782 ) ;
#10696 = CARTESIAN_POINT ( 'NONE',  ( -198.0356074513804288, -39.15871834505882276, -39.15871834505946936 ) ) ;
#10697 = CARTESIAN_POINT ( 'NONE',  ( -626.9846540392142060, 28.28427124746186649, 34.99999999999999289 ) ) ;
#10698 = CARTESIAN_POINT ( 'NONE',  ( 163.1118516004056573, 27.26290988616876021, 40.00000000000002132 ) ) ;
#10699 = CARTESIAN_POINT ( 'NONE',  ( 184.8905102610680444, 13.49065550809757497, 43.07788698682593065 ) ) ;
#10700 = AXIS2_PLACEMENT_3D ( 'NONE', #22855, #2495, #5026 ) ;
#10701 = CARTESIAN_POINT ( 'NONE',  ( -135.8532207217289738, 9.153146818113546246, -0.000000000000000000 ) ) ;
#10702 = CARTESIAN_POINT ( 'NONE',  ( -597.5075361363678894, 40.84977275671060681, 18.90368210877456434 ) ) ;
#10703 = VERTEX_POINT ( 'NONE', #25926 ) ;
#10704 = CARTESIAN_POINT ( 'NONE',  ( -238.4067589809705794, -39.99999999999963762, -40.96449428006383187 ) ) ;
#10705 = CARTESIAN_POINT ( 'NONE',  ( 199.0155016027679551, -13.51399019912108557, -14.74480745368398971 ) ) ;
#10706 = CARTESIAN_POINT ( 'NONE',  ( 133.2080217031555094, -12.38638889282761291, 29.90338805389101751 ) ) ;
#10707 = ORIENTED_EDGE ( 'NONE', *, *, #3427, .T. ) ;
#10709 = VERTEX_POINT ( 'NONE', #24453 ) ;
#10708 = EDGE_CURVE ( 'NONE', #18643, #9825, #14197, .T. ) ;
#10710 = CARTESIAN_POINT ( 'NONE',  ( 0.2972598230769930017, 54.33493731733936016, 40.00000000000002132 ) ) ;
#10711 = AXIS2_PLACEMENT_3D ( 'NONE', #24483, #7825, #4267 ) ;
#10712 = CARTESIAN_POINT ( 'NONE',  ( -110.0574180500383079, -19.22461201380497187, 6.256710540534125009 ) ) ;
#10713 = B_SPLINE_CURVE_WITH_KNOTS ( 'NONE', 3,
 ( #12036, #4465, #22294, #22690, #22431, #26298, #14559, #12561, #20155, #20694, #8038, #2461 ),
 .UNSPECIFIED., .F., .F.,
 ( 4, 2, 2, 2, 2, 4 ),
 ( 2.797157557069881010E-17, 0.005971652981263739571, 0.008957479471895556447, 0.01045039271721150131, 0.01119684933986943645, 0.01194330596252737159 ),
 .UNSPECIFIED. ) ;
#10714 = CARTESIAN_POINT ( 'NONE',  ( 116.7964245048383702, -19.78678521258524725, -19.78678521258533607 ) ) ;
#10715 = DIRECTION ( 'NONE',  ( -1.000000000000000000, 0.000000000000000000, 0.000000000000000000 ) ) ;
#10716 = CARTESIAN_POINT ( 'NONE',  ( 199.9999999999997726, 3.400090818600995934, -18.69490476363523612 ) ) ;
#10717 = CARTESIAN_POINT ( 'NONE',  ( -105.3841230195789791, 6.698392286129924322, -20.33917976067976596 ) ) ;
#10718 = CARTESIAN_POINT ( 'NONE',  ( 184.8905102610680444, -43.07788698682556827, -13.49065550809859104 ) ) ;
#10719 = CARTESIAN_POINT ( 'NONE',  ( -259.2033419157646676, 6.730120644403426944, 6.730120644403592145 ) ) ;
#10720 = CARTESIAN_POINT ( 'NONE',  ( -114.5516905194150183, -19.58901826161396187, -9.952133121982182473 ) ) ;
#10721 = CARTESIAN_POINT ( 'NONE',  ( -105.3755690713226585, 40.00000000000019185, -18.24025645688310249 ) ) ;
#10722 = CARTESIAN_POINT ( 'NONE',  ( 170.2234770963711128, -10.92277846919235529, 45.64576402573175073 ) ) ;
#10723 = CARTESIAN_POINT ( 'NONE',  ( -1.258540240222673523, 13.96099832920788764, 47.88180740053026341 ) ) ;
#10724 = DIRECTION ( 'NONE',  ( -1.000000000000000000, -1.836970198721030181E-16, 0.000000000000000000 ) ) ;
#10725 = CARTESIAN_POINT ( 'NONE',  ( -192.9588430854689705, -38.51493924976963967, 38.51493924976919914 ) ) ;
#10726 = CARTESIAN_POINT ( 'NONE',  ( 199.0129076123475045, 17.63563449655302051, 9.445111419240257433 ) ) ;
#10728 = CARTESIAN_POINT ( 'NONE',  ( -259.2033419157646676, -1.438356298054549103E-14, -9.517827891722632216 ) ) ;
#10727 = CARTESIAN_POINT ( 'NONE',  ( -198.0356074513804572, 10.87444709759730088, -10.87444709759707173 ) ) ;
#10729 = AXIS2_PLACEMENT_3D ( 'NONE', #25229, #484, #21234 ) ;
#10730 = CARTESIAN_POINT ( 'NONE',  ( 67.67011021033935947, 29.29769665555166469, -12.13550330100044583 ) ) ;
#10731 = CARTESIAN_POINT ( 'NONE',  ( 136.1360204305621266, -35.03383547441293899, 0.000000000000000000 ) ) ;
#10732 = CARTESIAN_POINT ( 'NONE',  ( 130.8568914410475088, -52.36146031193419503, 4.207082182989537955 ) ) ;
#10733 = CARTESIAN_POINT ( 'NONE',  ( 19.06497207195980792, 14.19242893257840876, 0.000000000000000000 ) ) ;
#10734 = ORIENTED_EDGE ( 'NONE', *, *, #6710, .F. ) ;
#10735 = CARTESIAN_POINT ( 'NONE',  ( -3.993758944536592193, -47.00698038897011344, 13.83056263162088051 ) ) ;
#10736 = CARTESIAN_POINT ( 'NONE',  ( -213.1075012329537230, 53.71589010951910836, 2.449293598294708485E-15 ) ) ;
#10737 = ORIENTED_EDGE ( 'NONE', *, *, #1640, .F. ) ;
#10738 = CARTESIAN_POINT ( 'NONE',  ( 23.37394308801977871, -23.33966569535037294, -42.85717664514612579 ) ) ;
#10739 = CARTESIAN_POINT ( 'NONE',  ( 57.59792236341147031, -1.722363176415032004, -1.722363176415048880 ) ) ;
#10740 = CARTESIAN_POINT ( 'NONE',  ( -4.081455915266636758, -17.86600351372037565, 43.13234798823257421 ) ) ;
#10741 = CARTESIAN_POINT ( 'NONE',  ( -5.379830816903563573, 13.73345071525145045, -46.52611083735715169 ) ) ;
#10742 = CARTESIAN_POINT ( 'NONE',  ( 199.0258314272957421, -17.94308652430182605, 8.851303907023687856 ) ) ;
#10743 = CARTESIAN_POINT ( 'NONE',  ( 4.995406935893289102, 10.78321810389013002, -10.78321810388986712 ) ) ;
#10744 = CARTESIAN_POINT ( 'NONE',  ( -626.9846540392097722, 75.00000000000000000, 65.00000000000002842 ) ) ;
#10745 = CARTESIAN_POINT ( 'NONE',  ( 170.0000000000000000, -30.00000000000001421, 3.673940397442065489E-15 ) ) ;
#10746 = CARTESIAN_POINT ( 'NONE',  ( -188.2507053402891586, -23.43979243030692317, 42.99082124348444722 ) ) ;
#10747 = CARTESIAN_POINT ( 'NONE',  ( 57.59792236341147031, 1.722363176415040886, 1.722363176415060426 ) ) ;
#10748 = CARTESIAN_POINT ( 'NONE',  ( 130.8568914410475088, 24.07718906446891793, 32.49135343045489321 ) ) ;
#10749 = CARTESIAN_POINT ( 'NONE',  ( -86.96347745069644475, -43.67073346367964604, -12.89780903124457545 ) ) ;
#10750 = CARTESIAN_POINT ( 'NONE',  ( 130.8568914410475372, 24.07718906447210472, 24.07718906447249907 ) ) ;
#10752 = CARTESIAN_POINT ( 'NONE',  ( -259.2033419157646676, -6.730120644402966867, -49.83842185052038332 ) ) ;
#10751 = CARTESIAN_POINT ( 'NONE',  ( -105.3755690713226727, 15.38646221621771737, 15.38646221621800514 ) ) ;
#10753 = CARTESIAN_POINT ( 'NONE',  ( 4.995406935893283773, 39.06748935135171052, 17.50105314357239195 ) ) ;
#10754 = CARTESIAN_POINT ( 'NONE',  ( -56.48582580120558561, -30.84685318188645908, 40.00000000000002132 ) ) ;
#10755 = CARTESIAN_POINT ( 'NONE',  ( -30.26275506840324070, 1.694272468446254232, 0.000000000000000000 ) ) ;
#10756 = CARTESIAN_POINT ( 'NONE',  ( 57.59792236341147031, 54.84617931850881689, -1.722363176414946073 ) ) ;
#10757 = DIRECTION ( 'NONE',  ( 1.000000000000000000, -1.836970198721030181E-16, -0.000000000000000000 ) ) ;
#10758 = CARTESIAN_POINT ( 'NONE',  ( -238.4067589809705794, -0.6820004457337348613, -57.25054294065803617 ) ) ;
#10759 = CARTESIAN_POINT ( 'NONE',  ( -174.2681662549567818, 39.26785901271982482, -16.26527976844781520 ) ) ;
#10760 = VERTEX_POINT ( 'NONE', #8073 ) ;
#10761 = CARTESIAN_POINT ( 'NONE',  ( 151.7948205124836250, 4.785054706301690608, 4.785054706301682614 ) ) ;
#10762 = CARTESIAN_POINT ( 'NONE',  ( -192.1167141818824291, -14.00295881688914790, -48.16218163818186326 ) ) ;
#10763 = CARTESIAN_POINT ( 'NONE',  ( -280.0000000000000000, -14.14213562373108779, 14.14213562373088529 ) ) ;
#10764 = CARTESIAN_POINT ( 'NONE',  ( 13.28449813601724827, -49.16593779331688552, -14.15462405555096304 ) ) ;
#10765 = ORIENTED_EDGE ( 'NONE', *, *, #24755, .F. ) ;
#10766 = CARTESIAN_POINT ( 'NONE',  ( -86.86493150571114086, -19.77569912839162569, 7.943527260496431985 ) ) ;
#10767 = CARTESIAN_POINT ( 'NONE',  ( -77.58456283179702950, -13.58505704039792050, -17.49511081174808069 ) ) ;
#10768 = CARTESIAN_POINT ( 'NONE',  ( 199.9999999999998010, 17.44192585402499418, -7.542491233669909256 ) ) ;
#10769 = DIRECTION ( 'NONE',  ( 0.000000000000000000, 0.000000000000000000, 1.000000000000000000 ) ) ;
#10770 = EDGE_CURVE ( 'NONE', #21913, #14253, #9940, .T. ) ;
#10771 = CARTESIAN_POINT ( 'NONE',  ( 14.38125909742180752, 55.17850393972636880, 2.449293598294708485E-15 ) ) ;
#10772 = CARTESIAN_POINT ( 'NONE',  ( 199.9999999999999432, -14.14213562373115884, 14.14213562373085153 ) ) ;
#10773 = CARTESIAN_POINT ( 'NONE',  ( 199.0198237862232133, 7.937771492746675150, 18.36232769351375538 ) ) ;
#10774 = CARTESIAN_POINT ( 'NONE',  ( -192.9588430854690273, -66.79921049721887982, -10.23066800229569040 ) ) ;
#10775 = CARTESIAN_POINT ( 'NONE',  ( -213.1075012329537230, 39.99999999999979394, 53.71589010950180665 ) ) ;
#10776 = CARTESIAN_POINT ( 'NONE',  ( -259.2033419157646676, -1.438356298054549103E-14, -9.517827891722632216 ) ) ;
#10777 =( BOUNDED_SURFACE ( )  B_SPLINE_SURFACE ( 3, 2, ( 
 ( #15491, #11373, #20267 ),
 ( #2046, #14138, #23620 ),
 ( #5401, #17984, #22269 ),
 ( #13866, #3769, #3912 ),
 ( #5271, #4044, #19993 ),
 ( #15996, #13375, #8013 ) ),
 .UNSPECIFIED., .F., .F., .F. ) 
 B_SPLINE_SURFACE_WITH_KNOTS ( ( 4, 2, 4 ),
 ( 3, 3 ),
 ( 0.04143173980255905609, 0.04845742520045778767, 0.05548311059835652620 ),
 ( 0.000000000000000000, 1.000000000000000000 ),
 .UNSPECIFIED. ) 
 GEOMETRIC_REPRESENTATION_ITEM ( )  RATIONAL_B_SPLINE_SURFACE ( (
 ( 1.000000000000000000, 0.9541700779530454257, 1.000000000000000000),
 ( 1.000000000000000000, 0.9520119910812291364, 1.000000000000000000),
 ( 1.000000000000000000, 0.9503148373211529609, 1.000000000000000000),
 ( 1.000000000000000000, 0.9480088447022436693, 1.000000000000000000),
 ( 1.000000000000000000, 0.9474362535696445597, 1.000000000000000000),
 ( 1.000000000000000000, 0.9474350314971539122, 1.000000000000000000) ) ) 
 REPRESENTATION_ITEM ( '' )  SURFACE ( )  );
#10778 = CARTESIAN_POINT ( 'NONE',  ( -210.0000000000000284, 72.72568232011437317, -59.67546976104961942 ) ) ;
#10779 = CARTESIAN_POINT ( 'NONE',  ( -56.48582580120557850, -30.84685318188645198, -2.449293598294708485E-15 ) ) ;
#10781 = CARTESIAN_POINT ( 'NONE',  ( 163.1118516004056573, 19.27778845538780317, -19.27778845538757224 ) ) ;
#10780 = CARTESIAN_POINT ( 'NONE',  ( 22.66553228237846795, -17.89571368754641867, -43.20407469282425694 ) ) ;
#10782 = ADVANCED_FACE ( 'NONE', ( #13788 ), #15779, .T. ) ;
#10783 = CARTESIAN_POINT ( 'NONE',  ( 130.8568914410475372, -5.949712681206667853, -2.449293598294708485E-15 ) ) ;
#10784 = ADVANCED_FACE ( 'NONE', ( #26059 ), #17903, .T. ) ;
#10785 = CARTESIAN_POINT ( 'NONE',  ( 0.2972598230770048811, -10.13633138497510089, 66.70487387989852834 ) ) ;
#10786 = CARTESIAN_POINT ( 'NONE',  ( 137.0939645874030361, -12.56330697291244824, -30.33050608226196232 ) ) ;
#10787 = CARTESIAN_POINT ( 'NONE',  ( -105.4741150117382205, 19.60045294982718644, -8.366608964594128395 ) ) ;
#10788 = CARTESIAN_POINT ( 'NONE',  ( 200.0000000000000000, 40.00000000000026290, -19.99999999999950617 ) ) ;
#10789 = CARTESIAN_POINT ( 'NONE',  ( 19.06497207195980792, 39.99999999999983658, 54.19242893257857929 ) ) ;
#10790 = CARTESIAN_POINT ( 'NONE',  ( -716.9846540392142060, 66.50000000000009948, 66.50000000000005684 ) ) ;
#10791 = CARTESIAN_POINT ( 'NONE',  ( -190.0000000000000000, 66.50000000000009948, -66.50000000000005684 ) ) ;
#10792 = FACE_OUTER_BOUND ( 'NONE', #14421, .T. ) ;
#10793 = CARTESIAN_POINT ( 'NONE',  ( 170.2234770963711128, -39.20704971665379190, -17.36149277827012938 ) ) ;
#10794 = VERTEX_POINT ( 'NONE', #902 ) ;
#10796 = CARTESIAN_POINT ( 'NONE',  ( -188.7701102708081748, 23.55033952083685023, -43.14144101424751199 ) ) ;
#10795 = CARTESIAN_POINT ( 'NONE',  ( -87.11162894489415010, 17.01505826596463322, -13.17695786912958589 ) ) ;
#10797 = CYLINDRICAL_SURFACE ( 'NONE', #21241, 30.00000000000000355 ) ;
#10798 = CARTESIAN_POINT ( 'NONE',  ( -86.96347745069643054, -18.24025645688353947, -40.00000000000002132 ) ) ;
#10799 = FACE_BOUND ( 'NONE', #19416, .T. ) ;
#10800 =( LENGTH_UNIT ( ) NAMED_UNIT ( * ) SI_UNIT ( .MILLI., .METRE. ) );
#10801 = EDGE_LOOP ( 'NONE', ( #597, #17454, #25006, #2290 ) ) ;
#10802 = ORIENTED_EDGE ( 'NONE', *, *, #17433, .T. ) ;
#10803 = CARTESIAN_POINT ( 'NONE',  ( 199.9999999999999432, -4.478796266106241042, 18.47916794701787069 ) ) ;
#10804 = SPHERICAL_SURFACE ( 'NONE', #12820, 15.00000000000000000 ) ;
#10805 = CARTESIAN_POINT ( 'NONE',  ( 23.40652632867838179, 13.79856377312528082, 46.79646383233881579 ) ) ;
#10806 = ORIENTED_EDGE ( 'NONE', *, *, #26161, .T. ) ;
#10807 = VERTEX_POINT ( 'NONE', #9014 ) ;
#10808 = CARTESIAN_POINT ( 'NONE',  ( 19.06497207195980792, 10.03556273973433299, 10.03556273973436319 ) ) ;
#10809 = CARTESIAN_POINT ( 'NONE',  ( 199.0242480509055270, -19.84286657041863933, 2.617213520271152394 ) ) ;
#10810 = CARTESIAN_POINT ( 'NONE',  ( -114.6297772183134782, -5.474609583110028765, 21.30737554389971677 ) ) ;
#10811 = CARTESIAN_POINT ( 'NONE',  ( 146.6084372240433993, -24.48358557860319706, -24.48358557860330720 ) ) ;
#10812 = CARTESIAN_POINT ( 'NONE',  ( -213.1075012329537230, 9.698598906450410340, 9.698598906450483170 ) ) ;
#10813 = CARTESIAN_POINT ( 'NONE',  ( -56.48582580120560692, 40.00000000000004263, -9.153146818113443217 ) ) ;
#10814 = CARTESIAN_POINT ( 'NONE',  ( -210.0000000000000284, 66.50000000000009948, 66.50000000000005684 ) ) ;
#10815 = CARTESIAN_POINT ( 'NONE',  ( -199.9999999999999147, 4.865628651907465851, 55.16984130227024252 ) ) ;
#10816 = CARTESIAN_POINT ( 'NONE',  ( 130.8568914410475088, 40.00000000000011369, -5.949712681206269949 ) ) ;
#10817 = CARTESIAN_POINT ( 'NONE',  ( 4.995406935893290878, 1.606505379428369110E-13, -15.24977328854832592 ) ) ;
#10818 = CARTESIAN_POINT ( 'NONE',  ( -82.26772520252667675, 17.52690089560000430, 10.09596362476956877 ) ) ;
#10819 = CARTESIAN_POINT ( 'NONE',  ( -369.0000000000000568, -4.857225732735059864E-14, 20.53474504356812247 ) ) ;
#10820 = CARTESIAN_POINT ( 'NONE',  ( 199.0073354103614918, 19.73522450985164411, -3.233483297802316692 ) ) ;
#10821 = CARTESIAN_POINT ( 'NONE',  ( -188.4265004370316205, 13.83489460444899244, 47.03620155434649064 ) ) ;
#10822 = CARTESIAN_POINT ( 'NONE',  ( -208.1127848780264742, -38.89260858015753541, 17.67593391476614784 ) ) ;
#10823 = CARTESIAN_POINT ( 'NONE',  ( -626.9846540392142060, 95.00000000000000000, 0.000000000000000000 ) ) ;
#10824 = CARTESIAN_POINT ( 'NONE',  ( -100.7734535825088500, 16.03295912088683295, 40.53558337403684675 ) ) ;
#10825 = CARTESIAN_POINT ( 'NONE',  ( -82.30220482034332008, -7.992411108785072216, 18.51665893431356480 ) ) ;
#10826 = CARTESIAN_POINT ( 'NONE',  ( 151.7948205124835681, 51.78348778862544322, -4.785054706298002891 ) ) ;
#10827 = CARTESIAN_POINT ( 'NONE',  ( -661.9859089885625281, 45.00097607149663048, -1.164717896653801654 ) ) ;
#10828 = DIRECTION ( 'NONE',  ( -0.01051738777841067576, 0.9166396752739927045, -0.3995761382614180235 ) ) ;
#10829 = CARTESIAN_POINT ( 'NONE',  ( 0.2972598230769938343, 10.13633138497486286, -10.13633138497461594 ) ) ;
#10830 = CARTESIAN_POINT ( 'NONE',  ( 151.7948205124836534, -6.767089262349006873, 40.00000000000002132 ) ) ;
#10831 = CARTESIAN_POINT ( 'NONE',  ( -596.9138871092466161, 41.28087457521051817, 17.94574729593260898 ) ) ;
#10832 = ORIENTED_EDGE ( 'NONE', *, *, #22495, .F. ) ;
#10833 = CARTESIAN_POINT ( 'NONE',  ( -105.3755690713226585, -39.99999999999985079, -18.24025645688394448 ) ) ;
#10834 = CARTESIAN_POINT ( 'NONE',  ( 199.0053898862218205, 12.24380588499195888, -15.86248857793228595 ) ) ;
#10835 = CARTESIAN_POINT ( 'NONE',  ( 141.7948666911894975, -12.58737617328932323, 30.38861427224615852 ) ) ;
#10836 = ORIENTED_EDGE ( 'NONE', *, *, #2252, .F. ) ;
#10837 = ORIENTED_EDGE ( 'NONE', *, *, #25724, .T. ) ;
#10838 = ORIENTED_EDGE ( 'NONE', *, *, #26318, .T. ) ;
#10839 = CARTESIAN_POINT ( 'NONE',  ( -30.26275506840324425, 41.69427246844627177, 40.00000000000002132 ) ) ;
#10840 = CARTESIAN_POINT ( 'NONE',  ( -103.9663809733125959, -19.92521373380484917, -8.574562932411120997 ) ) ;
#10841 = CARTESIAN_POINT ( 'NONE',  ( -110.0791661673351598, -19.70411816747342826, -4.394837301270150043 ) ) ;
#10842 = DIRECTION ( 'NONE',  ( -1.000000000000000000, -1.836970198721030181E-16, 0.000000000000000000 ) ) ;
#10843 = CARTESIAN_POINT ( 'NONE',  ( -362.0709805440841365, -4.857225732735059864E-14, 0.000000000000000000 ) ) ;
#10844 = CARTESIAN_POINT ( 'NONE',  ( 199.9999999999998579, 7.403094706059546226, -17.49952075364730675 ) ) ;
#10845 = CARTESIAN_POINT ( 'NONE',  ( 199.9999999999999147, 8.817827506411962446, -16.83089631069017145 ) ) ;
#10846 = CARTESIAN_POINT ( 'NONE',  ( 130.8568914410475088, -52.36146031193413108, -4.207082182990267150 ) ) ;
#10847 = CARTESIAN_POINT ( 'NONE',  ( 57.59792236341147031, 1.722363176415040886, 1.722363176415060426 ) ) ;
#10848 = FACE_OUTER_BOUND ( 'NONE', #3389, .T. ) ;
#10849 = CARTESIAN_POINT ( 'NONE',  ( -91.56559293963836410, 40.00000000000019185, -17.32597176626768487 ) ) ;
#10850 = CARTESIAN_POINT ( 'NONE',  ( -135.8532207217289738, 6.472252184284096543, 6.472252184284234211 ) ) ;
#10851 = CARTESIAN_POINT ( 'NONE',  ( 23.09931156284630305, 13.81622350327232240, 46.91113948292954205 ) ) ;
#10852 = CARTESIAN_POINT ( 'NONE',  ( 151.7948205124836534, -23.49921654116027980, 33.06932595376354556 ) ) ;
#10853 = CARTESIAN_POINT ( 'NONE',  ( -259.2033419157646676, 6.730120644403214669, 49.83842185052034068 ) ) ;
#10854 = CARTESIAN_POINT ( 'NONE',  ( 199.0081480328640566, 19.97905789705941260, -0.8430309673498267431 ) ) ;
#10856 = CARTESIAN_POINT ( 'NONE',  ( 184.8905102610680444, 40.00000000000013500, -20.92133201514430141 ) ) ;
#10855 = CARTESIAN_POINT ( 'NONE',  ( -259.2033419157646676, -6.730120644403663199, 6.730120644403451813 ) ) ;
#10857 = CARTESIAN_POINT ( 'NONE',  ( -86.96347745069644475, -21.75974354311651737, 0.000000000000000000 ) ) ;
#10858 = CARTESIAN_POINT ( 'NONE',  ( -192.9588430854690273, 10.23066800231970319, 66.79921049724369198 ) ) ;
#10859 = CARTESIAN_POINT ( 'NONE',  ( 192.4448373802101173, -20.00000000003938538, 40.00000000000002132 ) ) ;
#10860 = EDGE_LOOP ( 'NONE', ( #7435, #25551, #20916, #11593 ) ) ;
#10861 = CARTESIAN_POINT ( 'NONE',  ( 15.76057515053193647, -44.53539632573529872, 18.44716516375831716 ) ) ;
#10862 = AXIS2_PLACEMENT_3D ( 'NONE', #13473, #23714, #11466 ) ;
#10863 = AXIS2_PLACEMENT_3D ( 'NONE', #11258, #11013, #13506 ) ;
#10864 = CARTESIAN_POINT ( 'NONE',  ( 199.9999999999999432, 19.99999999999996092, 2.449293598294708485E-15 ) ) ;
#10865 = ADVANCED_FACE ( 'NONE', ( #15121 ), #10621, .T. ) ;
#10866 = ORIENTED_EDGE ( 'NONE', *, *, #14445, .F. ) ;
#10867 = CYLINDRICAL_SURFACE ( 'NONE', #25560, 30.00000000000000000 ) ;
#10868 = B_SPLINE_CURVE_WITH_KNOTS ( 'NONE', 3,
 ( #12355, #5849, #23934, #14092, #24073, #17943, #20221, #13955 ),
 .UNSPECIFIED., .F., .F.,
 ( 4, 2, 2, 4 ),
 ( 0.008467075098540726916, 0.01051709959615203076, 0.01256712409376333460, 0.01666717308898594402 ),
 .UNSPECIFIED. ) ;
#10869 = CARTESIAN_POINT ( 'NONE',  ( 19.06497207195980792, 10.03556273973433299, 10.03556273973436319 ) ) ;
#10870 = CARTESIAN_POINT ( 'NONE',  ( -62.62756078637954005, -10.52198127419510598, 25.40230989532181383 ) ) ;
#10871 = DIRECTION ( 'NONE',  ( 0.000000000000000000, 0.000000000000000000, 1.000000000000000000 ) ) ;
#10872 = EDGE_CURVE ( 'NONE', #23760, #13429, #20197, .T. ) ;
#10873 = CARTESIAN_POINT ( 'NONE',  ( 14.38125909742180752, 10.73282306404720465, 10.73282306404724018 ) ) ;
#10874 = CARTESIAN_POINT ( 'NONE',  ( 5.009865950673480839, -14.14399394884917527, -49.09576456953148949 ) ) ;
#10875 = CARTESIAN_POINT ( 'NONE',  ( 199.0232879746372134, -20.00360196692749071, -0.1645009869758431997 ) ) ;
#10876 = CARTESIAN_POINT ( 'NONE',  ( 57.59792236341147031, -1.722363176415055985, 1.722363176415024677 ) ) ;
#10877 = CARTESIAN_POINT ( 'NONE',  ( -82.23866954408245533, -20.16514221457112299, 1.261533135312056242 ) ) ;
#10878 = CARTESIAN_POINT ( 'NONE',  ( 130.8568914410475372, -34.05028731879786363, 0.000000000000000000 ) ) ;
#10879 = CARTESIAN_POINT ( 'NONE',  ( -194.4222169614009204, -14.07715596671739533, 48.65437996131331744 ) ) ;
#10880 = CARTESIAN_POINT ( 'NONE',  ( 19.06497207195981147, -10.03556273973425483, -10.03556273973443247 ) ) ;
#10881 = ADVANCED_FACE ( 'NONE', ( #21759 ), #7156, .F. ) ;
#10882 = CARTESIAN_POINT ( 'NONE',  ( 200.0000000000000000, 42.42640687119290988, 14.14213562373111976 ) ) ;
#10883 = CARTESIAN_POINT ( 'NONE',  ( -238.4067589809705794, 0.6820004457912851592, -0.6820004457913123597 ) ) ;
#10884 = LINE ( 'NONE', #9134, #15917 ) ;
#10885 = AXIS2_PLACEMENT_3D ( 'NONE', #25044, #18777, #6662 ) ;
#10886 = CIRCLE ( 'NONE', #4954, 15.00000000000000178 ) ;
#10888 = CARTESIAN_POINT ( 'NONE',  ( -259.2033419157646676, 21.55415060305860209, -21.55415060305812602 ) ) ;
#10887 = CARTESIAN_POINT ( 'NONE',  ( -192.9588430854690273, 18.05360324515473280, -38.51493924976924177 ) ) ;
#10889 = CARTESIAN_POINT ( 'NONE',  ( -100.7734535825088358, 12.25131212657497848, -12.25131212657469604 ) ) ;
#10890 = CARTESIAN_POINT ( 'NONE',  ( -208.1127848780265026, -15.00245453012673202, 0.000000000000000000 ) ) ;
#10891 = CARTESIAN_POINT ( 'NONE',  ( 170.2234770963711128, 15.44714144992819627, -40.00000000000002132 ) ) ;
#10892 = CARTESIAN_POINT ( 'NONE',  ( 151.7948205124836534, 33.06932595376365924, -23.49921654116018743 ) ) ;
#10893 = LINE ( 'NONE', #912, #22531 ) ;
#10894 = CARTESIAN_POINT ( 'NONE',  ( -56.48582580120559982, -21.81201906317804173, 34.75652343174591152 ) ) ;
#10895 = CARTESIAN_POINT ( 'NONE',  ( -187.8778500559049007, 43.02985669703468830, -17.82355023088518564 ) ) ;
#10896 = EDGE_LOOP ( 'NONE', ( #12988, #22449, #23055, #3622 ) ) ;
#10897 = CIRCLE ( 'NONE', #7470, 5.000000000000004441 ) ;
#10898 = CARTESIAN_POINT ( 'NONE',  ( -208.1127848780265026, 38.89260858015724409, 38.89260858015741462 ) ) ;
#10899 = CARTESIAN_POINT ( 'NONE',  ( -65.65550967526378656, 24.89650881518296188, -9.107276986623963566 ) ) ;
#10900 = CARTESIAN_POINT ( 'NONE',  ( -135.8532207217289738, 6.472252184283881604, 50.09629031063969506 ) ) ;
#10901 = CARTESIAN_POINT ( 'NONE',  ( 17.91733029159629709, -48.44632265251725300, -14.04577174277931384 ) ) ;
#10902 = ORIENTED_EDGE ( 'NONE', *, *, #9390, .F. ) ;
#10903 = CARTESIAN_POINT ( 'NONE',  ( -185.5190358317587709, -42.39054933780622036, 17.55874045219087165 ) ) ;
#10904 = CARTESIAN_POINT ( 'NONE',  ( -105.2054292635175585, -15.19799821370228621, -15.19799821370231818 ) ) ;
#10905 = CARTESIAN_POINT ( 'NONE',  ( 200.0000000000001421, 17.31676413174603013, -7.825505819403215213 ) ) ;
#10906 = CARTESIAN_POINT ( 'NONE',  ( 18.90082769090739134, 14.00978943384327735, -48.20711988125814429 ) ) ;
#10907 = CARTESIAN_POINT ( 'NONE',  ( -100.7734535825088500, 17.32597176626809699, -40.00000000000002132 ) ) ;
#10908 = CARTESIAN_POINT ( 'NONE',  ( -238.4067589809705794, 0.6820004457912851592, -0.6820004457913123597 ) ) ;
#10909 = CARTESIAN_POINT ( 'NONE',  ( 199.0120006491917479, 18.40818734026414560, 7.815811290271758693 ) ) ;
#10910 = AXIS2_PLACEMENT_3D ( 'NONE', #22957, #5000, #11105 ) ;
#10911 = CARTESIAN_POINT ( 'NONE',  ( 170.2234770963711128, -10.92277846919235529, 45.64576402573175073 ) ) ;
#10912 = CARTESIAN_POINT ( 'NONE',  ( -100.7734535825088500, -40.00000000000009948, 17.32597176626796909 ) ) ;
#10913 = CARTESIAN_POINT ( 'NONE',  ( -192.9588430854690273, 39.99999999999992895, 14.46834944099983922 ) ) ;
#10914 = CARTESIAN_POINT ( 'NONE',  ( -296.0000000000000000, -4.605747634845933236E-14, -20.53474504356812247 ) ) ;
#10915 = CARTESIAN_POINT ( 'NONE',  ( 136.1360204305621551, -4.966164525587036138, -40.00000000000002132 ) ) ;
#10917 = CARTESIAN_POINT ( 'NONE',  ( 91.82158438592158234, 12.16597498397773869, -12.16597498397759303 ) ) ;
#10916 = CARTESIAN_POINT ( 'NONE',  ( 22.76403192593580016, -17.88468650128144333, -43.17745271018603859 ) ) ;
#10918 = CARTESIAN_POINT ( 'NONE',  ( -208.1127848780264742, -55.00245453014425578, -40.00000000000002132 ) ) ;
#10919 = CARTESIAN_POINT ( 'NONE',  ( -105.3755690713226727, 15.38646221621793231, -15.38646221621779020 ) ) ;
#10920 = CARTESIAN_POINT ( 'NONE',  ( 144.1620285550791039, -12.51613133675853895, -30.21661402164560073 ) ) ;
#10921 = CARTESIAN_POINT ( 'NONE',  ( -198.0356074513804572, -39.99999999999990052, -15.37879056873112482 ) ) ;
#10922 = CARTESIAN_POINT ( 'NONE',  ( 91.82158438592158234, -12.16597498397761967, -12.16597498397768007 ) ) ;
#10923 = CARTESIAN_POINT ( 'NONE',  ( 35.93765801217426059, -20.78447758813318202, 38.99300236454103441 ) ) ;
#10924 = CARTESIAN_POINT ( 'NONE',  ( 98.29820294273281434, -7.653668647304240125, 18.47759065023114644 ) ) ;
#10925 = B_SPLINE_CURVE_WITH_KNOTS ( 'NONE', 3,
 ( #3612, #3232, #19452, #25848, #23828, #11723 ),
 .UNSPECIFIED., .F., .F.,
 ( 4, 2, 4 ),
 ( -5.998621905802982250E-08, 0.03938016914544736902, 0.07876039827711379948 ),
 .UNSPECIFIED. ) ;
#10926 = CARTESIAN_POINT ( 'NONE',  ( -280.0000000000000568, 14.14213562373067745, 42.42640687119295251 ) ) ;
#10927 = ORIENTED_EDGE ( 'NONE', *, *, #14192, .T. ) ;
#10929 = CARTESIAN_POINT ( 'NONE',  ( -7.233308327732243193, 42.27575367455148125, -17.51119053152626037 ) ) ;
#10928 = CARTESIAN_POINT ( 'NONE',  ( -77.67292258764865664, -4.800060567486668539, -21.50168463689548659 ) ) ;
#10930 = CARTESIAN_POINT ( 'NONE',  ( -716.9846540392142060, 66.50000000000009948, 66.50000000000005684 ) ) ;
#10931 = CARTESIAN_POINT ( 'NONE',  ( 14.38125909742181285, -15.17850393972633505, -40.00000000000002132 ) ) ;
#10932 = EDGE_CURVE ( 'NONE', #19642, #9531, #11604, .T. ) ;
#10933 = CARTESIAN_POINT ( 'NONE',  ( -114.4944481313177675, 9.302331659127901275, -19.81806240209493808 ) ) ;
#10934 = CARTESIAN_POINT ( 'NONE',  ( -188.6889827002346465, 43.11787295909656592, -23.53286111060870311 ) ) ;
#10935 = ORIENTED_EDGE ( 'NONE', *, *, #117, .F. ) ;
#10936 = EDGE_LOOP ( 'NONE', ( #13341, #10902, #25558, #4953, #20351, #14119 ) ) ;
#10937 = CARTESIAN_POINT ( 'NONE',  ( 199.9999999999999147, -4.931750674013845703, 18.35953736552815130 ) ) ;
#10938 = CARTESIAN_POINT ( 'NONE',  ( -86.86493150571126876, 8.366608963954069722, -19.60045294882757005 ) ) ;
#10939 = ORIENTED_EDGE ( 'NONE', *, *, #3266, .T. ) ;
#10940 = AXIS2_PLACEMENT_3D ( 'NONE', #25550, #15166, #23662 ) ;
#10941 = ORIENTED_EDGE ( 'NONE', *, *, #4114, .F. ) ;
#10942 = CARTESIAN_POINT ( 'NONE',  ( 130.8568914410475372, -24.07718906447222551, -24.07718906447233209 ) ) ;
#10943 = CARTESIAN_POINT ( 'NONE',  ( 199.0161314855084527, -14.37392100214799839, -13.91043101682956973 ) ) ;
#10944 = CARTESIAN_POINT ( 'NONE',  ( 190.0000000000000000, 61.50000000000009948, 66.50000000000005684 ) ) ;
#10945 = EDGE_CURVE ( 'NONE', #17137, #23643, #368, .T. ) ;
#10946 = CARTESIAN_POINT ( 'NONE',  ( 136.1360204305621266, -24.77266263493116583, -24.77266263493127951 ) ) ;
#10947 = AXIS2_PLACEMENT_3D ( 'NONE', #6499, #12622, #526 ) ;
#10948 = CARTESIAN_POINT ( 'NONE',  ( -162.0762913951020892, 1.198031840385716418, 1.198031840385750169 ) ) ;
#10949 = CARTESIAN_POINT ( 'NONE',  ( 4.995406935893292655, 39.99999999999982947, 55.24977328856478209 ) ) ;
#10950 = DIRECTION ( 'NONE',  ( -1.000000000000000000, -1.303213150798907793E-16, -2.465190328815661892E-32 ) ) ;
#10951 = CARTESIAN_POINT ( 'NONE',  ( -199.9999999999999432, -2.318131689465268957E-13, 55.16984130226961724 ) ) ;
#10952 = CARTESIAN_POINT ( 'NONE',  ( -213.1075012329537230, -39.99999999999948841, -53.71589010950208376 ) ) ;
#10953 = CARTESIAN_POINT ( 'NONE',  ( 136.1360204305621551, 39.99999999999968026, 35.03383547441337953 ) ) ;
#10954 = DIRECTION ( 'NONE',  ( 1.000000000000000000, 1.836970198721025990E-16, 0.000000000000000000 ) ) ;
#10955 = FACE_OUTER_BOUND ( 'NONE', #14523, .T. ) ;
#10956 = CARTESIAN_POINT ( 'NONE',  ( 199.0054512189284424, 16.16316501604694622, -11.77153054567511425 ) ) ;
#10957 = CARTESIAN_POINT ( 'NONE',  ( -238.4067589809705794, -0.6820004457913680929, 0.6820004457913170226 ) ) ;
#10958 = CARTESIAN_POINT ( 'NONE',  ( 199.9999999999999432, 14.14213562373093680, 14.14213562373114641 ) ) ;
#10959 = CARTESIAN_POINT ( 'NONE',  ( -350.0000000000001137, -4.857225732735059864E-14, 0.000000000000000000 ) ) ;
#10960 = CARTESIAN_POINT ( 'NONE',  ( 130.8568914410475372, -4.207082182992846420, 4.207082182992822439 ) ) ;
#10961 = CARTESIAN_POINT ( 'NONE',  ( -77.70933353445910541, -18.93828009115086886, 11.19441472888376410 ) ) ;
#10962 = CARTESIAN_POINT ( 'NONE',  ( -105.3755690713226585, 43.67073346367988051, -12.89780903124366418 ) ) ;
#10963 = CARTESIAN_POINT ( 'NONE',  ( -200.0000000000000000, 45.36622447512545619, -20.93268228684340571 ) ) ;
#10964 = CARTESIAN_POINT ( 'NONE',  ( -91.56559293963836410, 22.67402823373189946, -0.000000000000000000 ) ) ;
#10965 = ORIENTED_EDGE ( 'NONE', *, *, #16772, .T. ) ;
#10966 = CARTESIAN_POINT ( 'NONE',  ( -100.7734535825088500, 40.53558337403654832, 16.03295912088756481 ) ) ;
#10967 = CARTESIAN_POINT ( 'NONE',  ( 200.0000000000000000, -19.99999999999989342, 40.00000000000002132 ) ) ;
#10968 = CARTESIAN_POINT ( 'NONE',  ( -605.6399024805725730, 35.40302691160776050, 27.82394750457201127 ) ) ;
#10969 = EDGE_LOOP ( 'NONE', ( #6764, #6895, #23580, #12691 ) ) ;
#10970 = CARTESIAN_POINT ( 'NONE',  ( -198.0356074513804572, -39.99999999999990052, -15.37879056873112482 ) ) ;
#10971 = CARTESIAN_POINT ( 'NONE',  ( 199.0084482301557216, 0.03073351504823504388, -19.99623419276333536 ) ) ;
#10972 = CARTESIAN_POINT ( 'NONE',  ( 125.5832160019859600, -11.61997419108413609, 28.05309928653982965 ) ) ;
#10973 = ORIENTED_EDGE ( 'NONE', *, *, #25740, .T. ) ;
#10974 = VERTEX_POINT ( 'NONE', #9914 ) ;
#10975 = VERTEX_POINT ( 'NONE', #17497 ) ;
#10976 = CARTESIAN_POINT ( 'NONE',  ( -198.0356074513804572, 55.37879056871320671, 40.00000000000002132 ) ) ;
#10977 = ADVANCED_FACE ( 'NONE', ( #5528 ), #3308, .T. ) ;
#10978 = DIRECTION ( 'NONE',  ( 1.000000000000000000, 0.000000000000000000, 0.000000000000000000 ) ) ;
#10979 = DIRECTION ( 'NONE',  ( 0.000000000000000000, 0.000000000000000000, 1.000000000000000000 ) ) ;
#10980 = CARTESIAN_POINT ( 'NONE',  ( -199.9999999999998010, 49.28189405767604114, -14.17215463606931358 ) ) ;
#10981 = CARTESIAN_POINT ( 'NONE',  ( -105.3755690713226727, 5.661656051307470077E-14, -21.75974354311649961 ) ) ;
#10982 = CARTESIAN_POINT ( 'NONE',  ( 199.9999999999998863, -4.322767242657778120, -18.50495320732392557 ) ) ;
#10983 = CARTESIAN_POINT ( 'NONE',  ( 199.9999999999999716, -5.827982453606887603, -18.08981252677385498 ) ) ;
#10984 = CARTESIAN_POINT ( 'NONE',  ( 170.2234770963711128, -17.36149277826940462, -39.20704971665412586 ) ) ;
#10985 = CARTESIAN_POINT ( 'NONE',  ( 4.995406935893293543, -10.78321810388990265, -10.78321810389009272 ) ) ;
#10986 = DIRECTION ( 'NONE',  ( 0.000000000000000000, 1.000000000000000000, 0.000000000000000000 ) ) ;
#10987 = CARTESIAN_POINT ( 'NONE',  ( -192.9588430854689989, 5.375290060580374156E-13, -54.46834944099972375 ) ) ;
#10988 = LINE ( 'NONE', #2609, #16382 ) ;
#10989 = CARTESIAN_POINT ( 'NONE',  ( 19.06497207195981503, -14.19242893257840166, 0.000000000000000000 ) ) ;
#10990 = CARTESIAN_POINT ( 'NONE',  ( 91.82158438592159655, -16.11829626346147393, 16.11829626346132116 ) ) ;
#10991 = CARTESIAN_POINT ( 'NONE',  ( 199.0053897493126556, 15.86173083671449113, -12.24509968457356202 ) ) ;
#10993 = CARTESIAN_POINT ( 'NONE',  ( 4.995406935893290878, -5.232665749138292703E-14, 15.24977328854832592 ) ) ;
#10992 = CARTESIAN_POINT ( 'NONE',  ( -100.7734535825088358, -16.03295912088728770, 16.03295912088687913 ) ) ;
#10994 = DIRECTION ( 'NONE',  ( 1.000000000000000000, 1.836970198721030427E-16, -0.000000000000000000 ) ) ;
#10995 = CARTESIAN_POINT ( 'NONE',  ( 14.38125909742181463, 10.73282306405862485, 67.30136555898259587 ) ) ;
#10996 = CARTESIAN_POINT ( 'NONE',  ( -91.56559293963834989, 17.32597176626808988, 40.00000000000002132 ) ) ;
#10997 = EDGE_LOOP ( 'NONE', ( #2868, #23768, #25564, #16342, #13854 ) ) ;
#10998 = CARTESIAN_POINT ( 'NONE',  ( 16.10036699868849652, -48.79524671500755773, 14.09853761973996988 ) ) ;
#10999 = CARTESIAN_POINT ( 'NONE',  ( -213.1075012329537230, 53.71589010950162191, -40.00000000000002132 ) ) ;
#11000 = CARTESIAN_POINT ( 'NONE',  ( -200.0000000000000000, 66.50000000000009948, 66.50000000000005684 ) ) ;
#11001 = CARTESIAN_POINT ( 'NONE',  ( -259.2033419157646676, 21.55415060305830366, 21.55415060305842800 ) ) ;
#11002 = CARTESIAN_POINT ( 'NONE',  ( 57.59792236341147031, 1.908507979671054758E-14, -2.435789363418160658 ) ) ;
#11003 = CARTESIAN_POINT ( 'NONE',  ( -86.95085644346978881, 20.31668269185783871, -6.657466348996070593 ) ) ;
#11004 = CARTESIAN_POINT ( 'NONE',  ( -39.58644176656166991, 13.59899295360881588, -32.83087322320439938 ) ) ;
#11005 = CARTESIAN_POINT ( 'NONE',  ( 199.0234090143162859, -20.00365258984362882, 0.1656111763342176801 ) ) ;
#11006 = CARTESIAN_POINT ( 'NONE',  ( -259.2033419157646676, 49.83842185052017015, 6.730120644404137487 ) ) ;
#11007 = CARTESIAN_POINT ( 'NONE',  ( -77.55640685867214756, -22.13135000840951250, 0.6928334182904269944 ) ) ;
#11008 = SURFACE_STYLE_USAGE ( .BOTH. , #636 ) ;
#11010 = CARTESIAN_POINT ( 'NONE',  ( -198.9233928134752034, -14.16707757975546045, 49.24835219440009126 ) ) ;
#11009 = CIRCLE ( 'NONE', #822, 75.00000000000000000 ) ;
#11011 = CARTESIAN_POINT ( 'NONE',  ( 184.8905102610680444, -1.851754852062639767E-13, 20.92133201514444352 ) ) ;
#11012 = CARTESIAN_POINT ( 'NONE',  ( 170.2234770963711128, 45.64576402573181468, 10.92277846919223627 ) ) ;
#11013 = DIRECTION ( 'NONE',  ( 1.000000000000000000, 1.303213150798907793E-16, 2.465190328815661892E-32 ) ) ;
#11014 = CARTESIAN_POINT ( 'NONE',  ( -716.9846540392142060, -52.49999999999991473, 82.49999999999998579 ) ) ;
#11016 = CARTESIAN_POINT ( 'NONE',  ( -91.56559293963834989, 40.53558337403654832, 16.03295912088756481 ) ) ;
#11015 = CARTESIAN_POINT ( 'NONE',  ( -198.0356074513804572, 17.40982414986501325, -39.15871834505897198 ) ) ;
#11017 = CARTESIAN_POINT ( 'NONE',  ( 136.1360204305621551, 31.79587985999232558, 24.77266263493161702 ) ) ;
#11018 = CARTESIAN_POINT ( 'NONE',  ( 130.8568914410475088, 5.949712681206719367, -40.00000000000002132 ) ) ;
#11019 = CARTESIAN_POINT ( 'NONE',  ( -208.1127848780264742, 38.89260858015732936, -17.67593391476642140 ) ) ;
#11020 = DIRECTION ( 'NONE',  ( 0.000000000000000000, 0.000000000000000000, 1.000000000000000000 ) ) ;
#11021 = CARTESIAN_POINT ( 'NONE',  ( 4.995406935893312195, -67.35176059882525124, -10.78321810390210445 ) ) ;
#11022 = SPHERICAL_SURFACE ( 'NONE', #53, 15.00000000000000000 ) ;
#11023 = EDGE_LOOP ( 'NONE', ( #24477, #5237, #2558, #10001 ) ) ;
#11024 = CARTESIAN_POINT ( 'NONE',  ( -238.4067589809705794, 0.6820004457340470561, 57.25054294065803617 ) ) ;
#11025 = CYLINDRICAL_SURFACE ( 'NONE', #1437, 6.000000000000019540 ) ;
#11026 = CARTESIAN_POINT ( 'NONE',  ( -135.8532207217289738, 34.75652343174594705, 21.81201906317792449 ) ) ;
#11027 = CARTESIAN_POINT ( 'NONE',  ( 98.29820294273291381, -18.47759065023123526, -7.653668647304108674 ) ) ;
#11028 = ORIENTED_EDGE ( 'NONE', *, *, #13296, .F. ) ;
#11029 = CARTESIAN_POINT ( 'NONE',  ( -188.2870673237550818, -46.98612534495526205, 13.82722856953792068 ) ) ;
#11030 = EDGE_CURVE ( 'NONE', #21077, #5318, #13951, .T. ) ;
#11031 = CARTESIAN_POINT ( 'NONE',  ( 199.9999999999998579, -10.30558286630674658, -15.96802547070553047 ) ) ;
#11032 = CARTESIAN_POINT ( 'NONE',  ( 190.0000000000000000, 7.164183775012018789E-14, 0.000000000000000000 ) ) ;
#11033 = CARTESIAN_POINT ( 'NONE',  ( -280.0000000000000568, -20.00000000000006750, -40.00000000000002132 ) ) ;
#11034 = CARTESIAN_POINT ( 'NONE',  ( 200.0000000000000000, 60.27431767988573341, -73.32453023895050137 ) ) ;
#11035 = CARTESIAN_POINT ( 'NONE',  ( 199.0128224874292471, 17.70345943908711561, 9.303337553156843853 ) ) ;
#11036 = CARTESIAN_POINT ( 'NONE',  ( -208.1127848780265026, -10.60833733269537227, -10.60833733269551793 ) ) ;
#11037 = CARTESIAN_POINT ( 'NONE',  ( -162.0762913951020892, -1.777970010055771463E-13, 41.69427287682835015 ) ) ;
#11038 = CARTESIAN_POINT ( 'NONE',  ( -30.26275506840324070, -1.147469862568086380E-14, 1.694272468446259783 ) ) ;
#11039 = CARTESIAN_POINT ( 'NONE',  ( 0.4289713102705600689, 48.32239598606162900, -14.02712011273571946 ) ) ;
#11040 = CARTESIAN_POINT ( 'NONE',  ( 14.38125909742182884, -55.17850393974264733, -40.00000000000002132 ) ) ;
#11042 = CARTESIAN_POINT ( 'NONE',  ( -605.5768371412766555, 34.03271882474869159, 21.02205817263521226 ) ) ;
#11041 = CARTESIAN_POINT ( 'NONE',  ( 27.00968939605884245, -17.38581019152039531, -41.97305875718011237 ) ) ;
#11043 = CARTESIAN_POINT ( 'NONE',  ( 130.8568914410475088, 34.05028731879790627, 40.00000000000002132 ) ) ;
#11044 = CARTESIAN_POINT ( 'NONE',  ( -280.0000000000000000, 14.14213562373098299, -14.14213562373088706 ) ) ;
#11045 = CARTESIAN_POINT ( 'NONE',  ( 4.995406935893283773, 40.00000000000017764, -15.24977328854790848 ) ) ;
#11046 = CARTESIAN_POINT ( 'NONE',  ( -105.2276882639850015, 13.16704209471405029, -17.02247659825660975 ) ) ;
#11047 = CARTESIAN_POINT ( 'NONE',  ( -56.48582580120558561, -40.00000000000012790, 9.153146818113166105 ) ) ;
#11048 = CARTESIAN_POINT ( 'NONE',  ( -86.96347745069644475, -15.38646221621786125, -15.38646221621789856 ) ) ;
#11049 = CARTESIAN_POINT ( 'NONE',  ( 153.3016677565462942, -28.42263824612669154, -11.77304223996991261 ) ) ;
#11050 = CARTESIAN_POINT ( 'NONE',  ( -56.48582580120559982, 21.81201906317729922, 34.75652343174635917 ) ) ;
#11051 = CARTESIAN_POINT ( 'NONE',  ( -280.0000000000000568, 42.42640687119274645, 14.14213562373118194 ) ) ;
#11052 = ORIENTED_EDGE ( 'NONE', *, *, #9955, .F. ) ;
#11054 = CARTESIAN_POINT ( 'NONE',  ( -70.33906594826318326, 22.79894061131100003, -9.443630412774925986 ) ) ;
#11053 = CARTESIAN_POINT ( 'NONE',  ( -87.13361725327074225, 16.16366093422423589, -14.23233549119255059 ) ) ;
#11055 = FACE_OUTER_BOUND ( 'NONE', #1246, .T. ) ;
#11056 = CARTESIAN_POINT ( 'NONE',  ( 0.2972598230769983307, -14.33493731733933352, 40.00000000000002132 ) ) ;
#11057 = AXIS2_PLACEMENT_3D ( 'NONE', #17382, #25521, #23002 ) ;
#11058 = CARTESIAN_POINT ( 'NONE',  ( -192.9588430854689989, 10.23066800230756712, -10.23066800230735396 ) ) ;
#11059 = CARTESIAN_POINT ( 'NONE',  ( -190.7345856381643898, 47.78725959878585172, -13.94676320010617054 ) ) ;
#11060 = DIRECTION ( 'NONE',  ( 1.836970198721030181E-16, -1.000000000000000000, 1.047444401652940007E-14 ) ) ;
#11061 = ORIENTED_EDGE ( 'NONE', *, *, #6208, .T. ) ;
#11062 = ORIENTED_EDGE ( 'NONE', *, *, #4457, .F. ) ;
#11063 = CARTESIAN_POINT ( 'NONE',  ( 73.43468099484969969, -26.88834960806366681, -12.96803874020853797 ) ) ;
#11064 = CARTESIAN_POINT ( 'NONE',  ( -199.9999999999998579, 44.86878812508723513, -24.82633483071237634 ) ) ;
#11065 = ORIENTED_EDGE ( 'NONE', *, *, #6891, .T. ) ;
#11066 = CARTESIAN_POINT ( 'NONE',  ( 199.0208257245452899, -19.09599194444923143, -5.955353076589812389 ) ) ;
#11067 = CARTESIAN_POINT ( 'NONE',  ( -210.0000000000000284, 72.72568232011437317, -59.67546976104961942 ) ) ;
#11068 = CARTESIAN_POINT ( 'NONE',  ( -30.26275506840324070, 1.198031551615912571, 57.76657404653985139 ) ) ;
#11069 = CARTESIAN_POINT ( 'NONE',  ( 190.0000000000000000, -71.50000000000002842, -66.50000000000005684 ) ) ;
#11070 = CARTESIAN_POINT ( 'NONE',  ( -91.56559293963836410, 40.00000000000008527, -22.67402823373177867 ) ) ;
#11071 = CARTESIAN_POINT ( 'NONE',  ( -200.0000000000000568, -46.84854965773187985, 17.28402242884639151 ) ) ;
#11072 = FACE_BOUND ( 'NONE', #24172, .T. ) ;
#11073 = AXIS2_PLACEMENT_3D ( 'NONE', #16277, #8425, #6172 ) ;
#11074 = CARTESIAN_POINT ( 'NONE',  ( 14.38125909742182529, -39.99999999999944578, -55.17850393971050238 ) ) ;
#11075 = CARTESIAN_POINT ( 'NONE',  ( 192.4448373802100889, 2.472897170449861688E-13, -19.99999999996060751 ) ) ;
#11076 = CARTESIAN_POINT ( 'NONE',  ( -114.5514240060904001, -19.59008466214005750, 9.949107728608549195 ) ) ;
#11077 = DIRECTION ( 'NONE',  ( -0.000000000000000000, 0.000000000000000000, 1.000000000000000000 ) ) ;
#11078 = CARTESIAN_POINT ( 'NONE',  ( -30.26275506840324070, -1.147469862568086380E-14, 1.694272468446259783 ) ) ;
#11079 = CARTESIAN_POINT ( 'NONE',  ( 151.7948205124836250, 23.49921654116361225, -23.49921654116333514 ) ) ;
#11080 = CARTESIAN_POINT ( 'NONE',  ( -89.92902785008678279, 8.088236460649781634, 20.44110050034142745 ) ) ;
#11081 = CARTESIAN_POINT ( 'NONE',  ( -99.29480781227293562, 8.934325994365014623, 20.48155342677144475 ) ) ;
#11082 = FACE_BOUND ( 'NONE', #3490, .T. ) ;
#11083 = CARTESIAN_POINT ( 'NONE',  ( 14.38125909742182529, -39.01709431150879936, -39.01709431150948859 ) ) ;
#11084 = CARTESIAN_POINT ( 'NONE',  ( -129.2303573021169143, -9.309001178959640299, -25.82247248365550263 ) ) ;
#11085 = CARTESIAN_POINT ( 'NONE',  ( -1.821043593238330205, 23.89737153267520142, 43.61003463695173821 ) ) ;
#11086 = ORIENTED_EDGE ( 'NONE', *, *, #3146, .T. ) ;
#11087 = CARTESIAN_POINT ( 'NONE',  ( 57.59792236341147031, -1.722363176415055985, 1.722363176415024677 ) ) ;
#11088 = CARTESIAN_POINT ( 'NONE',  ( 151.7948205124836250, 33.23291073765556547, 0.000000000000000000 ) ) ;
#11089 = CARTESIAN_POINT ( 'NONE',  ( -592.3042890440465271, 44.75177432878896155, -4.872409619293819105 ) ) ;
#11090 = ORIENTED_EDGE ( 'NONE', *, *, #13704, .T. ) ;
#11091 = CARTESIAN_POINT ( 'NONE',  ( -135.8532207217289738, -40.00000000000014211, 9.153146818113153671 ) ) ;
#11092 = CARTESIAN_POINT ( 'NONE',  ( 199.0119170695921582, -7.658365714851820272, -18.47347012762973151 ) ) ;
#11093 = DIRECTION ( 'NONE',  ( 0.000000000000000000, -1.000000000000000000, 0.000000000000000000 ) ) ;
#11094 = EDGE_LOOP ( 'NONE', ( #21206, #24113 ) ) ;
#11095 = EDGE_LOOP ( 'NONE', ( #3790, #4422, #4300, #20257 ) ) ;
#11096 = EDGE_LOOP ( 'NONE', ( #4200, #3546, #7551, #20553 ) ) ;
#11097 = CARTESIAN_POINT ( 'NONE',  ( -280.0000000000000568, 19.99999999999996447, -40.00000000000002132 ) ) ;
#11098 = B_SPLINE_CURVE_WITH_KNOTS ( 'NONE', 3,
 ( #843, #8687, #13079, #2847, #19061, #16666 ),
 .UNSPECIFIED., .F., .F.,
 ( 4, 2, 4 ),
 ( 0.000000000000000000, 0.004089961189160419563, 0.008179922378320839127 ),
 .UNSPECIFIED. ) ;
#11099 = EDGE_CURVE ( 'NONE', #3746, #87, #20431, .T. ) ;
#11100 = CARTESIAN_POINT ( 'NONE',  ( -77.67292258764859980, -18.59814239105924827, 11.80983163630759414 ) ) ;
#11101 = CARTESIAN_POINT ( 'NONE',  ( 184.8905102610680444, 1.070102760522089011E-13, -20.92133201514444352 ) ) ;
#11102 = CARTESIAN_POINT ( 'NONE',  ( 200.0000000000000000, -10.04040541317802315, -16.13598245992451297 ) ) ;
#11103 = CIRCLE ( 'NONE', #17467, 74.99999999999995737 ) ;
#11104 = EDGE_CURVE ( 'NONE', #3577, #19812, #20778, .T. ) ;
#11105 = DIRECTION ( 'NONE',  ( 0.000000000000000000, 0.000000000000000000, 1.000000000000000000 ) ) ;
#11106 = CARTESIAN_POINT ( 'NONE',  ( -70.35386311798177417, -8.707385185642063874, -23.12931224674694164 ) ) ;
#11107 = CARTESIAN_POINT ( 'NONE',  ( 91.82158438592158234, 12.16597498397756993, 12.16597498397776356 ) ) ;
#11108 = FACE_OUTER_BOUND ( 'NONE', #9697, .T. ) ;
#11109 = CARTESIAN_POINT ( 'NONE',  ( -259.2033419157646676, 2.741182173978444749E-13, -30.48217210827739621 ) ) ;
#11110 = CARTESIAN_POINT ( 'NONE',  ( 91.82158438592158234, 12.16597498397756993, 12.16597498397776356 ) ) ;
#11111 = CARTESIAN_POINT ( 'NONE',  ( 130.8568914410475088, 34.05028731879790627, -40.00000000000002132 ) ) ;
#11112 = ADVANCED_FACE ( 'NONE', ( #6066, #16300 ), #24561, .F. ) ;
#11113 = EDGE_CURVE ( 'NONE', #21343, #21338, #6323, .T. ) ;
#11114 = CARTESIAN_POINT ( 'NONE',  ( 0.2972598230770048811, -10.13633138497510089, 66.70487387989852834 ) ) ;
#11115 = CARTESIAN_POINT ( 'NONE',  ( -280.0000000000000000, 19.99999999999996092, -0.000000000000000000 ) ) ;
#11117 = CARTESIAN_POINT ( 'NONE',  ( -135.8532207217289738, 7.002209520526292428E-15, -9.153146818113572891 ) ) ;
#11116 = CARTESIAN_POINT ( 'NONE',  ( -238.4067589809705794, 0.6820004457912851592, -0.6820004457913123597 ) ) ;
#11118 = FACE_OUTER_BOUND ( 'NONE', #16211, .T. ) ;
#11119 = CARTESIAN_POINT ( 'NONE',  ( 136.1360204305621266, -24.77266263493116583, -24.77266263493127951 ) ) ;
#11120 = CARTESIAN_POINT ( 'NONE',  ( 57.59792236341147031, -2.435789363418150444, 0.000000000000000000 ) ) ;
#11121 = B_SPLINE_CURVE_WITH_KNOTS ( 'NONE', 3,
 ( #19177, #5322, #9066, #25306, #15301, #23305, #13187, #3084, #1082, #5846 ),
 .UNSPECIFIED., .F., .F.,
 ( 4, 2, 2, 2, 4 ),
 ( 0.7921542097163948304, 0.8508620842112317728, 0.8814014469398914198, 0.9119408096685510667, 0.9406682828395580565 ),
 .UNSPECIFIED. ) ;
#11122 = ORIENTED_EDGE ( 'NONE', *, *, #3532, .F. ) ;
#11123 = CARTESIAN_POINT ( 'NONE',  ( 21.80824205439684249, -43.30754100652733740, 23.67346680103123191 ) ) ;
#11124 = CONICAL_SURFACE ( 'NONE', #3051, 20.53474504356812247, 0.7853981633974725929 ) ;
#11125 = CARTESIAN_POINT ( 'NONE',  ( 57.59792236341147031, -2.435789363418150000, -40.00000000000002132 ) ) ;
#11126 = CARTESIAN_POINT ( 'NONE',  ( -105.2110227778628939, 16.13864963247413442, -14.20565731138971088 ) ) ;
#11127 = CARTESIAN_POINT ( 'NONE',  ( -259.2033419157646676, -6.730120644403667640, 49.83842185052029805 ) ) ;
#11128 = CARTESIAN_POINT ( 'NONE',  ( 146.6084372240433993, 1.478241399363601114E-13, -34.62501878078305850 ) ) ;
#11129 = CARTESIAN_POINT ( 'NONE',  ( -87.00601149411200197, 20.66743745453288739, 5.745309048958548992 ) ) ;
#11130 = CARTESIAN_POINT ( 'NONE',  ( 199.0053211801402426, 14.13499912481545451, -14.14174623454970536 ) ) ;
#11131 = CARTESIAN_POINT ( 'NONE',  ( 199.0228518427889242, -19.96294788386713037, -1.312843269464072815 ) ) ;
#11132 = CARTESIAN_POINT ( 'NONE',  ( -213.1075012329537230, 9.698598906450543566, -9.698598906450348167 ) ) ;
#11133 = CARTESIAN_POINT ( 'NONE',  ( -82.23729782345287731, -1.277530580954402861, -20.19443213282674776 ) ) ;
#11134 = CARTESIAN_POINT ( 'NONE',  ( -213.1075012329537230, 9.698598906450543566, -9.698598906450348167 ) ) ;
#11135 = DIRECTION ( 'NONE',  ( 0.000000000000000000, 0.000000000000000000, 1.000000000000000000 ) ) ;
#11136 = CARTESIAN_POINT ( 'NONE',  ( -213.1075012329537230, 18.58567234101121102, 37.98287015391247223 ) ) ;
#11137 = CARTESIAN_POINT ( 'NONE',  ( 91.82158438592158234, -12.16597498397778843, 12.16597498397750954 ) ) ;
#11138 = CARTESIAN_POINT ( 'NONE',  ( -280.0000000000000000, 14.14213562373078581, 14.14213562373108424 ) ) ;
#11139 = VECTOR ( 'NONE', #25591, 1000.000000000000000 ) ;
#11141 = CARTESIAN_POINT ( 'NONE',  ( 136.1360204305621551, 31.79587985999232558, 24.77266263493161702 ) ) ;
#11140 = CARTESIAN_POINT ( 'NONE',  ( 163.1118516004056573, 19.27778845538753316, 19.27778845538783870 ) ) ;
#11142 = CARTESIAN_POINT ( 'NONE',  ( -192.9588430854689989, 38.51493924976983152, -38.51493924976893624 ) ) ;
#11143 = CARTESIAN_POINT ( 'NONE',  ( -56.48582580120559982, 30.84685318188643777, -40.00000000000002132 ) ) ;
#11144 = CARTESIAN_POINT ( 'NONE',  ( 170.2234770963711128, 10.92277846919210660, -45.64576402573182889 ) ) ;
#11145 = CARTESIAN_POINT ( 'NONE',  ( -200.0000000000000000, 52.49999999999987210, 82.49999999999998579 ) ) ;
#11146 = CARTESIAN_POINT ( 'NONE',  ( -56.48582580120558561, -50.09629031063971638, 6.472252184283745713 ) ) ;
#11147 = LINE ( 'NONE', #4647, #16184 ) ;
#11148 = ORIENTED_EDGE ( 'NONE', *, *, #14182, .F. ) ;
#11149 = CARTESIAN_POINT ( 'NONE',  ( 91.82158438592158234, 16.11829626346139577, 16.11829626346143840 ) ) ;
#11150 = CARTESIAN_POINT ( 'NONE',  ( 170.0000000000001421, 9.369682556672135121, 22.62041470344889760 ) ) ;
#11151 = CARTESIAN_POINT ( 'NONE',  ( -47.45115950045780551, -29.80449331803366775, -14.84795788642767356 ) ) ;
#11152 = ORIENTED_EDGE ( 'NONE', *, *, #9144, .F. ) ;
#11153 = CARTESIAN_POINT ( 'NONE',  ( -121.8281105901183849, -23.07023229738023673, 8.694016233238142988 ) ) ;
#11154 = CARTESIAN_POINT ( 'NONE',  ( 199.9999999999999147, 1.697088945475840660, -18.92594139730135439 ) ) ;
#11155 = CARTESIAN_POINT ( 'NONE',  ( 23.36927571439207796, -23.34061495561071808, 42.85861222363632805 ) ) ;
#11156 = CARTESIAN_POINT ( 'NONE',  ( 98.29820294267314296, 18.47759065023127079, 7.653668647304075812 ) ) ;
#11157 = CARTESIAN_POINT ( 'NONE',  ( 199.0127395736742244, 17.77917978336349236, 9.157720830221606434 ) ) ;
#11158 = CARTESIAN_POINT ( 'NONE',  ( -100.7734535825088500, -12.25131212657524316, 44.31723036834888774 ) ) ;
#11159 = CARTESIAN_POINT ( 'NONE',  ( -213.1075012329537230, -8.703598725189323045E-14, 13.71589010951911902 ) ) ;
#11160 = CARTESIAN_POINT ( 'NONE',  ( 190.0000000000001137, 30.00000000000007461, 0.000000000000000000 ) ) ;
#11161 = CARTESIAN_POINT ( 'NONE',  ( 136.1360204305621266, 35.03383547441298163, -40.00000000000002132 ) ) ;
#11163 = CARTESIAN_POINT ( 'NONE',  ( -598.5566012994313496, 38.83482129691294205, 9.596881470589549323 ) ) ;
#11162 = CARTESIAN_POINT ( 'NONE',  ( 23.37583784646148644, -13.80085822090975434, -46.80752016581924835 ) ) ;
#11164 = CARTESIAN_POINT ( 'NONE',  ( 200.0000000000000000, 20.00000000000013856, 40.00000000000002132 ) ) ;
#11165 = CARTESIAN_POINT ( 'NONE',  ( 19.06497207195980792, 18.24870850772737185, 38.31983398719634692 ) ) ;
#11166 = CARTESIAN_POINT ( 'NONE',  ( 184.8905102610680444, 39.99999999999983658, 20.92133201514485563 ) ) ;
#11167 = CYLINDRICAL_SURFACE ( 'NONE', #22144, 5.000000000000004441 ) ;
#11168 = CARTESIAN_POINT ( 'NONE',  ( -105.3755690713226585, -39.99999999999985079, -18.24025645688394448 ) ) ;
#11169 = EDGE_CURVE ( 'NONE', #25214, #16256, #2077, .T. ) ;
#11170 = CARTESIAN_POINT ( 'NONE',  ( 133.2072010122031713, -29.90326689760170709, -12.38633870824907568 ) ) ;
#11171 = CARTESIAN_POINT ( 'NONE',  ( -105.3755690713226727, -15.38646221621807619, 15.38646221621768362 ) ) ;
#11172 = CARTESIAN_POINT ( 'NONE',  ( -213.1075012329537230, -9.698598906438496314, 66.26714140136188291 ) ) ;
#11173 = VERTEX_POINT ( 'NONE', #18288 ) ;
#11175 = CARTESIAN_POINT ( 'NONE',  ( 8.273828130719147467, 44.87796109790431842, -18.58906013839431282 ) ) ;
#11174 = CARTESIAN_POINT ( 'NONE',  ( -77.55672185583993894, -1.410533997352584334, -22.12963403628582171 ) ) ;
#11176 = CARTESIAN_POINT ( 'NONE',  ( -162.0762913951021176, -1.694272876828353702, 40.00000000000002132 ) ) ;
#11177 = CARTESIAN_POINT ( 'NONE',  ( -138.9613198120158302, -29.42718893709543337, 10.11110880661598443 ) ) ;
#11178 = LINE ( 'NONE', #19293, #11496 ) ;
#11179 = DIRECTION ( 'NONE',  ( 1.000000000000000000, 0.000000000000000000, 0.000000000000000000 ) ) ;
#11180 = VERTEX_POINT ( 'NONE', #18562 ) ;
#11181 = ORIENTED_EDGE ( 'NONE', *, *, #6382, .F. ) ;
#11182 = CARTESIAN_POINT ( 'NONE',  ( -97.72675010090424053, -20.56394680065914926, 8.987772175319408419 ) ) ;
#11183 = CARTESIAN_POINT ( 'NONE',  ( -93.02511667906942705, 8.169918093965671702, -20.82219708225684940 ) ) ;
#11184 = VERTEX_POINT ( 'NONE', #16435 ) ;
#11185 = CARTESIAN_POINT ( 'NONE',  ( 199.9999999999997726, -8.411091645968788555, 17.05096182211362432 ) ) ;
#11186 = FACE_OUTER_BOUND ( 'NONE', #25047, .T. ) ;
#11187 = ADVANCED_FACE ( 'NONE', ( #4470, #22565 ), #12436, .T. ) ;
#11188 = CARTESIAN_POINT ( 'NONE',  ( 170.2234770963711128, -17.36149277826985937, -17.36149277826995174 ) ) ;
#11189 = DIRECTION ( 'NONE',  ( 1.000000000000000000, 0.000000000000000000, 0.000000000000000000 ) ) ;
#11190 = CARTESIAN_POINT ( 'NONE',  ( 163.1118516004056573, 40.00000000000014921, -27.26290988616858968 ) ) ;
#11191 = CARTESIAN_POINT ( 'NONE',  ( 17.76569288431004878, -14.04863394049465519, 48.46476365406687137 ) ) ;
#11192 = ADVANCED_BREP_SHAPE_REPRESENTATION ( '', ( #26080, #21058 ), #20184 ) ;
#11193 = EDGE_CURVE ( 'NONE', #10668, #16337, #8312, .T. ) ;
#11194 = DIRECTION ( 'NONE',  ( 1.000000000000000000, 1.836970198721030427E-16, -0.000000000000000000 ) ) ;
#11195 = CARTESIAN_POINT ( 'NONE',  ( -162.0762913951021176, -40.00000000000003553, -1.694272876828743168 ) ) ;
#11196 = CARTESIAN_POINT ( 'NONE',  ( 151.7948205124836534, 40.00000000000012079, -6.767089262348609857 ) ) ;
#11197 = CARTESIAN_POINT ( 'NONE',  ( -716.9846540392142060, -82.49999999999991473, -52.49999999999977973 ) ) ;
#11198 = CARTESIAN_POINT ( 'NONE',  ( -56.48582580120559271, 6.472252184284211118, -6.472252184284153387 ) ) ;
#11199 = CARTESIAN_POINT ( 'NONE',  ( -265.0000000000000000, -4.734761052820324716E-14, -10.00000000000000000 ) ) ;
#11200 = CARTESIAN_POINT ( 'NONE',  ( -198.0356074513804572, -10.87444709759729911, 10.87444709759714812 ) ) ;
#11201 = LINE ( 'NONE', #15318, #25742 ) ;
#11202 = EDGE_CURVE ( 'NONE', #17668, #8569, #2521, .T. ) ;
#11203 = DIRECTION ( 'NONE',  ( 0.000000000000000000, 0.000000000000000000, 1.000000000000000000 ) ) ;
#11204 = DIRECTION ( 'NONE',  ( -1.000000000000000000, -0.000000000000000000, -0.000000000000000000 ) ) ;
#11205 = CARTESIAN_POINT ( 'NONE',  ( -77.59243545049976376, -13.54949188064048116, 17.47199274922497381 ) ) ;
#11206 = CARTESIAN_POINT ( 'NONE',  ( 184.8905102610680444, -41.77492675556007384, 14.79361573936348684 ) ) ;
#11207 = CARTESIAN_POINT ( 'NONE',  ( -151.7004448983857117, -13.46262099565286796, -32.50164219297025170 ) ) ;
#11208 = CARTESIAN_POINT ( 'NONE',  ( 7.340276910564533352, 24.82763627182876931, 44.87059041559387396 ) ) ;
#11209 = EDGE_LOOP ( 'NONE', ( #8255, #20603, #7101, #26084, #23341, #6798, #10275, #19776, #3652, #14485 ) ) ;
#11210 = CARTESIAN_POINT ( 'NONE',  ( -86.96347745069644475, -15.38646221621738164, -41.18208027870615240 ) ) ;
#11211 = DIRECTION ( 'NONE',  ( 0.000000000000000000, 1.000000000000000000, 0.000000000000000000 ) ) ;
#11212 = CARTESIAN_POINT ( 'NONE',  ( -618.6895405067469937, 29.47063081262555784, 34.00782742777329304 ) ) ;
#11213 = VERTEX_POINT ( 'NONE', #2468 ) ;
#11214 = APPLICATION_CONTEXT ( 'automotive_design' ) ;
#11215 = CARTESIAN_POINT ( 'NONE',  ( -91.56559293963834989, -2.543181659092656077E-13, 22.67402823373191723 ) ) ;
#11216 = CARTESIAN_POINT ( 'NONE',  ( 199.0233417977821091, -20.00361827599568798, -0.01770272352667627211 ) ) ;
#11217 = CARTESIAN_POINT ( 'NONE',  ( 14.32711916788068152, -44.71189734681519923, 24.71075626504589096 ) ) ;
#11218 = ORIENTED_EDGE ( 'NONE', *, *, #465, .F. ) ;
#11219 = VERTEX_POINT ( 'NONE', #6580 ) ;
#11220 = CARTESIAN_POINT ( 'NONE',  ( 57.59792236341147031, 37.56421063658187620, 2.449293598294708485E-15 ) ) ;
#11221 = UNCERTAINTY_MEASURE_WITH_UNIT (LENGTH_MEASURE( 1.000000000000000082E-05 ), #25985, 'distance_accuracy_value', 'NONE');
#11222 = CARTESIAN_POINT ( 'NONE',  ( -91.56559293963836410, 16.03295912088714203, -16.03295912088699282 ) ) ;
#11223 = CARTESIAN_POINT ( 'NONE',  ( 184.8905102610680444, 39.99999999999999289, 19.07866798485573057 ) ) ;
#11224 = CARTESIAN_POINT ( 'NONE',  ( -77.70896657118075268, -18.93513500903290137, 11.20032855622331702 ) ) ;
#11225 = CARTESIAN_POINT ( 'NONE',  ( -238.4067589809705794, -40.00000000000007105, 0.9644942799824426372 ) ) ;
#11226 = CARTESIAN_POINT ( 'NONE',  ( 199.9999999999998579, -18.00099009291985297, -6.105420735363839668 ) ) ;
#11227 = DIRECTION ( 'NONE',  ( 0.9698969544100555229, 0.09318942523065473771, -0.2249791742612613499 ) ) ;
#11228 = CARTESIAN_POINT ( 'NONE',  ( -8.197988474444986906, -17.40147972965361589, -42.01088836873536536 ) ) ;
#11229 = CARTESIAN_POINT ( 'NONE',  ( 136.1360204305621266, 24.77266263493104148, 24.77266263493145004 ) ) ;
#11230 = CARTESIAN_POINT ( 'NONE',  ( -105.2272256531326207, -17.01582848540546777, -13.17790690984702984 ) ) ;
#11231 = CARTESIAN_POINT ( 'NONE',  ( 184.8905102610680444, -39.99999999999978684, -19.07866798485600768 ) ) ;
#11232 = DIRECTION ( 'NONE',  ( 0.000000000000000000, 1.000000000000000000, 0.000000000000000000 ) ) ;
#11233 = CARTESIAN_POINT ( 'NONE',  ( 136.1360204305621551, -4.966164525587036138, -40.00000000000002132 ) ) ;
#11234 = CARTESIAN_POINT ( 'NONE',  ( 170.2234770963711128, -39.20704971665379190, -17.36149277827012938 ) ) ;
#11235 = CARTESIAN_POINT ( 'NONE',  ( -56.48582580120559982, 9.153146818113574668, -40.00000000000002132 ) ) ;
#11237 = CARTESIAN_POINT ( 'NONE',  ( -105.3755690713226727, 5.661656051307470077E-14, -21.75974354311649961 ) ) ;
#11236 = CARTESIAN_POINT ( 'NONE',  ( 23.30631261066300297, -42.87793822514719011, -23.35506702544013180 ) ) ;
#11238 = CARTESIAN_POINT ( 'NONE',  ( 170.0000000000000000, 1.183443619805854272E-13, -24.95097643317000546 ) ) ;
#11239 = CARTESIAN_POINT ( 'NONE',  ( -198.0356074513804572, 67.44298959253333692, 10.87444709760969452 ) ) ;
#11240 = CARTESIAN_POINT ( 'NONE',  ( -192.9588430854689989, 54.46834944099968823, 2.449293598294708485E-15 ) ) ;
#11241 = ORIENTED_EDGE ( 'NONE', *, *, #20205, .T. ) ;
#11242 = EDGE_CURVE ( 'NONE', #10069, #1078, #21222, .T. ) ;
#11243 = CARTESIAN_POINT ( 'NONE',  ( -3.417371742523301670, -43.31092608455668369, 17.93997298316205047 ) ) ;
#11244 = DIRECTION ( 'NONE',  ( -1.850371707708594760E-15, 0.9166903767334100284, -0.3995982397413169185 ) ) ;
#11245 = EDGE_CURVE ( 'NONE', #18786, #12394, #2446, .T. ) ;
#11246 = CARTESIAN_POINT ( 'NONE',  ( 163.1118516004056573, -19.27778845539233998, 37.29075403953149959 ) ) ;
#11247 = CARTESIAN_POINT ( 'NONE',  ( -105.3755690713226727, 5.661656051307470077E-14, -21.75974354311649961 ) ) ;
#11248 = CARTESIAN_POINT ( 'NONE',  ( -87.06808288329423817, 21.06763942722659877, 4.035072084556908578 ) ) ;
#11249 = EDGE_CURVE ( 'NONE', #10794, #23424, #876, .T. ) ;
#11250 = CARTESIAN_POINT ( 'NONE',  ( -4.039451493210483690, -13.82811171175408127, -46.99046209229819482 ) ) ;
#11251 = CARTESIAN_POINT ( 'NONE',  ( 200.0000000000000000, 2.003163845861910097, 18.90332168644373567 ) ) ;
#11252 = CARTESIAN_POINT ( 'NONE',  ( -652.7925989268254625, 36.95172673408348629, -15.41345145336517319 ) ) ;
#11253 = CARTESIAN_POINT ( 'NONE',  ( 200.0000000000000000, -13.44239485489230290, 13.44239485489200803 ) ) ;
#11254 = CARTESIAN_POINT ( 'NONE',  ( 0.2972598230769938343, 10.13633138497486286, -10.13633138497461594 ) ) ;
#11255 = CARTESIAN_POINT ( 'NONE',  ( -30.26275506840323359, -1.198031551615522439, -57.76657404653986561 ) ) ;
#11256 = AXIS2_PLACEMENT_3D ( 'NONE', #13182, #5316, #3078 ) ;
#11257 = CARTESIAN_POINT ( 'NONE',  ( -86.96347745069645896, 43.67073346367970288, 12.89780903124427702 ) ) ;
#11258 = CARTESIAN_POINT ( 'NONE',  ( 190.0000000000000000, -66.50000000000001421, 66.50000000000005684 ) ) ;
#11259 = CARTESIAN_POINT ( 'NONE',  ( -208.1127848780264742, -38.89260858015704514, -38.89260858015768463 ) ) ;
#11261 = CARTESIAN_POINT ( 'NONE',  ( -100.7734535825088500, -44.31723036834885932, -12.25131212657538171 ) ) ;
#11260 = CARTESIAN_POINT ( 'NONE',  ( -135.8532207217289738, 6.472252184284583265, -50.09629031063960980 ) ) ;
#11262 = CARTESIAN_POINT ( 'NONE',  ( 192.4448373802100889, 14.14213562370330379, -14.14213562370292365 ) ) ;
#11263 = CARTESIAN_POINT ( 'NONE',  ( 57.59792236341147031, -2.435789363418150000, -40.00000000000002132 ) ) ;
#11264 = CARTESIAN_POINT ( 'NONE',  ( 151.7948205124836250, -23.49921654116339553, -23.49921654116350211 ) ) ;
#11265 = CARTESIAN_POINT ( 'NONE',  ( -200.0000000000000000, 2.362121657692426575E-30, 0.000000000000000000 ) ) ;
#11266 = MECHANICAL_DESIGN_GEOMETRIC_PRESENTATION_REPRESENTATION (  '', ( #24456 ), #12990 ) ;
#11267 = CARTESIAN_POINT ( 'NONE',  ( 199.9999999999999432, -14.14213562373073607, -14.14213562373102206 ) ) ;
#11268 = CIRCLE ( 'NONE', #12541, 5.000000000000004441 ) ;
#11269 = CARTESIAN_POINT ( 'NONE',  ( -188.2956751479547393, 43.00407324591997593, -23.44846780264088437 ) ) ;
#11270 = EDGE_LOOP ( 'NONE', ( #24949, #8086 ) ) ;
#11271 = CARTESIAN_POINT ( 'NONE',  ( -105.3755690713226585, 41.18208027870598187, -15.38646221621779731 ) ) ;
#11272 = DIRECTION ( 'NONE',  ( 0.000000000000000000, -1.000000000000000000, 0.000000000000000000 ) ) ;
#11273 = CARTESIAN_POINT ( 'NONE',  ( 16.10036699856384956, 14.09853761972935615, 48.79524671503644129 ) ) ;
#11274 = CARTESIAN_POINT ( 'NONE',  ( -87.02142894580126153, -20.76642173392621515, 5.408203463872810701 ) ) ;
#11275 = ORIENTED_EDGE ( 'NONE', *, *, #6541, .T. ) ;
#11276 = CARTESIAN_POINT ( 'NONE',  ( -105.2349941599195802, 17.04272630156315316, 13.08094329434171144 ) ) ;
#11277 = PRODUCT_DEFINITION_FORMATION_WITH_SPECIFIED_SOURCE ( 'ANY', '', #3800, .NOT_KNOWN. ) ;
#11278 = CARTESIAN_POINT ( 'NONE',  ( 200.0000000000005116, -0.6320235832414241584, -19.00127953747481868 ) ) ;
#11279 = CARTESIAN_POINT ( 'NONE',  ( 22.50777602749776207, -17.91321921095823910, 43.24633676486227785 ) ) ;
#11280 = ADVANCED_FACE ( 'NONE', ( #4608 ), #25474, .T. ) ;
#11281 = CARTESIAN_POINT ( 'NONE',  ( 27.79909650596783877, 22.43832426418754267, -41.49206490659992141 ) ) ;
#11282 = CARTESIAN_POINT ( 'NONE',  ( 199.0067627483201989, 19.31843298438769807, -5.161535144790875940 ) ) ;
#11283 = AXIS2_PLACEMENT_3D ( 'NONE', #17787, #7673, #5303 ) ;
#11284 = CARTESIAN_POINT ( 'NONE',  ( -296.0000000000000000, -4.857225732735059864E-14, 0.000000000000000000 ) ) ;
#11285 = CARTESIAN_POINT ( 'NONE',  ( 19.06497207195979726, 39.99999999999997158, 14.19242893257854554 ) ) ;
#11286 = CARTESIAN_POINT ( 'NONE',  ( 163.1118516004056573, 1.251511021549353291E-13, -27.26290988616872824 ) ) ;
#11287 = CARTESIAN_POINT ( 'NONE',  ( -199.9999999999999716, -16.05666331275163117, -47.66874763508944568 ) ) ;
#11288 = CARTESIAN_POINT ( 'NONE',  ( -105.3755690713226585, -18.24025645688353947, -40.00000000000002132 ) ) ;
#11290 = FACE_OUTER_BOUND ( 'NONE', #6333, .T. ) ;
#11289 = CARTESIAN_POINT ( 'NONE',  ( 20.69615274310995190, -23.88537831998747052, -43.59383154590273790 ) ) ;
#11291 = CARTESIAN_POINT ( 'NONE',  ( -91.56559293963834989, -17.32597176626812896, 40.00000000000002132 ) ) ;
#11293 = CARTESIAN_POINT ( 'NONE',  ( -213.1075012329537230, -13.71589010951915810, 0.000000000000000000 ) ) ;
#11292 = AXIS2_PLACEMENT_3D ( 'NONE', #13664, #3055, #5056 ) ;
#11294 = AXIS2_PLACEMENT_3D ( 'NONE', #9817, #25796, #3563 ) ;
#11295 = CARTESIAN_POINT ( 'NONE',  ( 163.1118516004056573, 39.99999999999976552, 27.26290988616914746 ) ) ;
#11296 = CARTESIAN_POINT ( 'NONE',  ( 4.995406935893297984, -39.99999999999986500, -15.24977328854874870 ) ) ;
#11297 = AXIS2_PLACEMENT_3D ( 'NONE', #16971, #4749, #2754 ) ;
#11298 = CARTESIAN_POINT ( 'NONE',  ( 127.8226996004795950, -28.75922372236458813, -11.91246050912548071 ) ) ;
#11299 = EDGE_LOOP ( 'NONE', ( #22745, #23294, #14784, #9282 ) ) ;
#11301 = CARTESIAN_POINT ( 'NONE',  ( -4.004886986945064287, 43.01537795656800256, -23.45685150724343870 ) ) ;
#11300 = DIRECTION ( 'NONE',  ( 0.000000000000000000, -1.000000000000000000, 0.000000000000000000 ) ) ;
#11302 = CARTESIAN_POINT ( 'NONE',  ( -280.0000000000000568, -20.00000000000007105, 40.00000000000002132 ) ) ;
#11303 = CARTESIAN_POINT ( 'NONE',  ( -199.0731274799843504, 44.83667511838923048, -18.57195892570682361 ) ) ;
#11304 = EDGE_LOOP ( 'NONE', ( #24636, #13682 ) ) ;
#11305 = ORIENTED_EDGE ( 'NONE', *, *, #1499, .T. ) ;
#11306 = CARTESIAN_POINT ( 'NONE',  ( -99.29480781227283614, -20.48155342677143409, 8.934325994365179824 ) ) ;
#11307 = CARTESIAN_POINT ( 'NONE',  ( 90.71511022951216319, -21.46756116403335568, -8.335579107441619229 ) ) ;
#11308 = EDGE_LOOP ( 'NONE', ( #1372, #18952, #15075, #19174 ) ) ;
#11309 = ORIENTED_EDGE ( 'NONE', *, *, #7502, .F. ) ;
#11310 =( BOUNDED_CURVE ( )  B_SPLINE_CURVE ( 3, ( #25893, #23743, #17243, #5152 ),
 .UNSPECIFIED., .F., .F. ) 
 B_SPLINE_CURVE_WITH_KNOTS ( ( 4, 4 ),
 ( 0.01388163287021919670, 0.02359082919309990825 ),
 .UNSPECIFIED. ) 
 CURVE ( )  GEOMETRIC_REPRESENTATION_ITEM ( )  RATIONAL_B_SPLINE_CURVE ( ( 1.000000000000000000, 0.8672072324489000783, 0.7608653435686208999, 0.6809743333591623538 ) ) 
 REPRESENTATION_ITEM ( '' )  );
#11311 = CARTESIAN_POINT ( 'NONE',  ( 199.9999999999998863, -7.850736592177782747, 17.31604939001003274 ) ) ;
#11312 = CARTESIAN_POINT ( 'NONE',  ( -109.1264249741452232, 13.72187187126506558, -33.12752917268247188 ) ) ;
#11313 = AXIS2_PLACEMENT_3D ( 'NONE', #10341, #1971, #1838 ) ;
#11314 = CARTESIAN_POINT ( 'NONE',  ( 184.8905102610680444, 13.49065550809807945, 13.49065550809809544 ) ) ;
#11315 = DIRECTION ( 'NONE',  ( 1.000000000000000000, 1.303213150798907793E-16, 2.465190328815661892E-32 ) ) ;
#11316 = CARTESIAN_POINT ( 'NONE',  ( 4.995406935893290878, -5.232665749138292703E-14, 15.24977328854832592 ) ) ;
#11317 = CARTESIAN_POINT ( 'NONE',  ( -200.0000000000000284, -45.36622447512538514, 20.93268228684354426 ) ) ;
#11318 = FACE_OUTER_BOUND ( 'NONE', #15939, .T. ) ;
#11319 = CARTESIAN_POINT ( 'NONE',  ( -105.3755690713226585, -40.00000000000027711, 21.75974354311608749 ) ) ;
#11320 = CARTESIAN_POINT ( 'NONE',  ( 0.2972598230770030492, 5.716321584140269555E-13, -54.33493731733936016 ) ) ;
#11321 = CARTESIAN_POINT ( 'NONE',  ( -105.3178975793387337, -18.51275824393216496, 10.85284064411901817 ) ) ;
#11322 = CARTESIAN_POINT ( 'NONE',  ( 184.8905102610680444, -13.49065550809780412, -43.07788698682583828 ) ) ;
#11323 = CARTESIAN_POINT ( 'NONE',  ( 170.2234770963711128, 1.169953928977015745E-13, -24.55285855007187124 ) ) ;
#11324 = CARTESIAN_POINT ( 'NONE',  ( -362.0709805440841365, -4.857225732735059864E-14, 20.53474504356812247 ) ) ;
#11325 = CARTESIAN_POINT ( 'NONE',  ( 127.8236149080040889, 28.75948073575744601, 11.91256696755863054 ) ) ;
#11326 = CARTESIAN_POINT ( 'NONE',  ( 98.29820294271928560, -10.07205412907102549, -17.47586258463233477 ) ) ;
#11327 = CARTESIAN_POINT ( 'NONE',  ( -56.48582580120559271, 6.472252184284211118, -6.472252184284153387 ) ) ;
#11328 = CARTESIAN_POINT ( 'NONE',  ( -77.55658273871470954, -16.64052652070192195, 14.65657382809084552 ) ) ;
#11329 = CARTESIAN_POINT ( 'NONE',  ( -56.48582580120559982, -34.75652343174615311, 21.81201906317766870 ) ) ;
#11330 = CARTESIAN_POINT ( 'NONE',  ( -86.96347745069645896, -12.89780903124443689, 43.67073346367968156 ) ) ;
#11331 = CARTESIAN_POINT ( 'NONE',  ( -658.8956941877264626, 42.64142712027438620, -14.38834502120623249 ) ) ;
#11332 = CARTESIAN_POINT ( 'NONE',  ( -726.9846540392142060, 52.49999999999991473, -82.49999999999998579 ) ) ;
#11333 = ORIENTED_EDGE ( 'NONE', *, *, #24254, .F. ) ;
#11334 = CARTESIAN_POINT ( 'NONE',  ( -162.0762913951020892, 29.48230308784799902, -29.48230308784730980 ) ) ;
#11335 = DIRECTION ( 'NONE',  ( 0.000000000000000000, -1.000000000000000000, 0.000000000000000000 ) ) ;
#11336 = AXIS2_PLACEMENT_3D ( 'NONE', #1184, #5295, #5052 ) ;
#11337 = FACE_OUTER_BOUND ( 'NONE', #9253, .T. ) ;
#11338 = ORIENTED_EDGE ( 'NONE', *, *, #19215, .T. ) ;
#11339 = CARTESIAN_POINT ( 'NONE',  ( -208.1127848780265026, 1.189126717069624012E-13, -15.00245453012669472 ) ) ;
#11340 = CARTESIAN_POINT ( 'NONE',  ( 199.0233350887612289, -20.00359049402684875, -0.03597354547537223030 ) ) ;
#11341 = CARTESIAN_POINT ( 'NONE',  ( 0.4289717129526404160, -44.08776571100848685, 24.25042218720266618 ) ) ;
#11342 = EDGE_LOOP ( 'NONE', ( #15263, #16946, #17103, #3330 ) ) ;
#11343 = ORIENTED_EDGE ( 'NONE', *, *, #8923, .T. ) ;
#11344 = CARTESIAN_POINT ( 'NONE',  ( -200.4318156386405576, -49.29858106685330910, -14.17468120671522236 ) ) ;
#11345 = CARTESIAN_POINT ( 'NONE',  ( -198.0356074513804572, 39.99999999999979394, 55.37879056874835726 ) ) ;
#11346 = ADVANCED_FACE ( 'NONE', ( #20832 ), #23100, .F. ) ;
#11347 = ADVANCED_FACE ( 'NONE', ( #9241 ), #2462, .T. ) ;
#11348 = CARTESIAN_POINT ( 'NONE',  ( 190.0000000000000000, 7.164183775012017527E-14, 0.000000000000000000 ) ) ;
#11349 = DIRECTION ( 'NONE',  ( -1.000000000000000000, -0.000000000000000000, -0.000000000000000000 ) ) ;
#11350 = CARTESIAN_POINT ( 'NONE',  ( 199.9999999999999147, -14.49496992596536771, -12.29673964441684042 ) ) ;
#11351 = CARTESIAN_POINT ( 'NONE',  ( 190.0000000000000000, 52.50000000000007816, 52.49999999999999289 ) ) ;
#11352 = CARTESIAN_POINT ( 'NONE',  ( -70.35386311679275195, -10.19784240597756941, -22.51194465199612438 ) ) ;
#11353 = CARTESIAN_POINT ( 'NONE',  ( -208.1127848780264742, 17.67593391476678377, -38.89260858015718014 ) ) ;
#11354 = CARTESIAN_POINT ( 'NONE',  ( -77.61444910505873906, -21.81614215778263244, 3.470426107494282597 ) ) ;
#11355 = CARTESIAN_POINT ( 'NONE',  ( -280.0000000000000568, -39.99999999999987210, -20.00000000000043343 ) ) ;
#11356 = CARTESIAN_POINT ( 'NONE',  ( 48.46159092537987334, -37.63079858261907873, -11.89574569450916286 ) ) ;
#11357 = CARTESIAN_POINT ( 'NONE',  ( -162.0762913951020892, -1.694272876828353702, 0.000000000000000000 ) ) ;
#11358 = CARTESIAN_POINT ( 'NONE',  ( 151.7948205124835681, 33.23291073765556547, -40.00000000000002132 ) ) ;
#11359 = CARTESIAN_POINT ( 'NONE',  ( 192.4448373802101173, 42.42640687122070631, 14.14213562370331623 ) ) ;
#11360 = CARTESIAN_POINT ( 'NONE',  ( -208.1127848780264742, -15.00245453012673202, -40.00000000000002132 ) ) ;
#11362 = DIRECTION ( 'NONE',  ( -0.000000000000000000, -1.000000000000000000, -0.000000000000000000 ) ) ;
#11361 = CARTESIAN_POINT ( 'NONE',  ( -4.039451493210478361, -43.00522595893993838, -23.44932283416681429 ) ) ;
#11363 = CARTESIAN_POINT ( 'NONE',  ( -280.0000000000000000, -2.609240458947769655E-13, 20.00000000000001421 ) ) ;
#11364 = CARTESIAN_POINT ( 'NONE',  ( 146.6084372240433709, 32.08495691632064961, -24.48358557860320417 ) ) ;
#11365 = CARTESIAN_POINT ( 'NONE',  ( -91.56559293963834989, 17.32597176626809343, 2.449293598294708485E-15 ) ) ;
#11366 = ORIENTED_EDGE ( 'NONE', *, *, #22166, .T. ) ;
#11367 = CARTESIAN_POINT ( 'NONE',  ( 22.75856136761861492, -43.17893233522182328, 17.88529938203894787 ) ) ;
#11368 = CARTESIAN_POINT ( 'NONE',  ( -86.95488169845611992, -9.644899311047964829, 19.11867441905828002 ) ) ;
#11369 = CARTESIAN_POINT ( 'NONE',  ( -105.3755690713226727, 12.89780903124400879, 12.89780903124407452 ) ) ;
#11370 = CARTESIAN_POINT ( 'NONE',  ( -86.83718372825752851, 19.60232422073417879, 8.316105076740864632 ) ) ;
#11371 = CARTESIAN_POINT ( 'NONE',  ( -5.296937277117006460, 17.72975434250563254, -42.80341339123120292 ) ) ;
#11372 = CARTESIAN_POINT ( 'NONE',  ( 199.9999999999999716, -3.868950841772955673, 18.61236034055575317 ) ) ;
#11373 = CARTESIAN_POINT ( 'NONE',  ( -82.30220482034327745, -18.74474319042430892, -7.441767004318710299 ) ) ;
#11374 = CARTESIAN_POINT ( 'NONE',  ( -77.90255099906775627, -8.064892378658402805, -20.29001641120661148 ) ) ;
#11375 = CARTESIAN_POINT ( 'NONE',  ( 91.82158438592158234, -12.16597498397778843, 12.16597498397750954 ) ) ;
#11376 = CARTESIAN_POINT ( 'NONE',  ( 192.4448373802101173, 42.42640687122089815, -14.14213562370272470 ) ) ;
#11377 = CARTESIAN_POINT ( 'NONE',  ( -114.6419057268807791, 21.37096723866840975, -5.444467006605387738 ) ) ;
#11378 = DIRECTION ( 'NONE',  ( 1.836970198721030181E-16, 1.000000000000000000, -1.321694076934715579E-16 ) ) ;
#11379 = CARTESIAN_POINT ( 'NONE',  ( -238.4067589809705794, -0.6820004457337348613, -57.25054294065803617 ) ) ;
#11381 = CARTESIAN_POINT ( 'NONE',  ( 14.38125909742181463, 10.73282306403652875, -67.30136555895941797 ) ) ;
#11380 = CARTESIAN_POINT ( 'NONE',  ( 14.38125909742181996, -10.73282306405815234, -67.30136555898266693 ) ) ;
#11382 = CARTESIAN_POINT ( 'NONE',  ( 14.38125909742180397, 67.30136555898270956, -10.73282306405792319 ) ) ;
#11383 = CARTESIAN_POINT ( 'NONE',  ( 0.2972598230769930572, 14.33493731733933352, 0.000000000000000000 ) ) ;
#11384 = CARTESIAN_POINT ( 'NONE',  ( 0.000000000000000000, 0.000000000000000000, 0.000000000000000000 ) ) ;
#11385 = CARTESIAN_POINT ( 'NONE',  ( 19.06497207195981147, -4.605042221739098431E-14, 14.19242893257840521 ) ) ;
#11386 = CARTESIAN_POINT ( 'NONE',  ( 163.1118516004056573, -37.29075403953166301, 19.27778845539196695 ) ) ;
#11387 = CARTESIAN_POINT ( 'NONE',  ( -192.9588430854690273, 14.46834944099966336, 40.00000000000002132 ) ) ;
#11388 = EDGE_LOOP ( 'NONE', ( #22684, #7859, #23547, #9118 ) ) ;
#11389 = CARTESIAN_POINT ( 'NONE',  ( -100.7734535825088500, 40.53558337403677569, -16.03295912088699993 ) ) ;
#11390 = CARTESIAN_POINT ( 'NONE',  ( -89.92902785008715227, -20.44110050034142745, -8.088236460650017889 ) ) ;
#11391 = CARTESIAN_POINT ( 'NONE',  ( -28.75808802591297209, -12.03522322449749637, -38.33175228464058648 ) ) ;
#11392 = CARTESIAN_POINT ( 'NONE',  ( -4.660840668352969729, -46.77528141313101173, -13.78427145221207262 ) ) ;
#11393 = EDGE_LOOP ( 'NONE', ( #17424, #6102, #10838, #20473 ) ) ;
#11394 = CARTESIAN_POINT ( 'NONE',  ( -188.2956751479547108, -43.00407324591987646, 23.44846780264116859 ) ) ;
#11395 = CARTESIAN_POINT ( 'NONE',  ( 199.9999999999997726, -2.174764995058875439, -18.87968408895515182 ) ) ;
#11396 = CARTESIAN_POINT ( 'NONE',  ( 98.29820294267315717, -7.653668647304115780, 18.47759065023121039 ) ) ;
#11397 = VECTOR ( 'NONE', #3244, 1000.000000000000000 ) ;
#11398 = CARTESIAN_POINT ( 'NONE',  ( 170.0000000000000000, -12.70659020859111088, 21.59613885783081955 ) ) ;
#11399 = CARTESIAN_POINT ( 'NONE',  ( 199.0077026597514021, 2.114100997916472657, -19.88449140175694296 ) ) ;
#11400 =( BOUNDED_SURFACE ( )  B_SPLINE_SURFACE ( 3, 2, ( 
 ( #13803, #5448, #16071 ),
 ( #26347, #5698, #15799 ),
 ( #21938, #1719, #18195 ),
 ( #24200, #11816, #24062 ),
 ( #19935, #10092, #11678 ),
 ( #19670, #5972, #8088 ),
 ( #7555, #20208, #16208 ),
 ( #11953, #19803, #7685 ),
 ( #20078, #15667, #13549 ),
 ( #1856, #23923, #23793 ),
 ( #1590, #9959, #21678 ),
 ( #22212, #21802, #14081 ) ),
 .UNSPECIFIED., .F., .F., .F. ) 
 B_SPLINE_SURFACE_WITH_KNOTS ( ( 4, 2, 2, 2, 2, 4 ),
 ( 3, 3 ),
 ( 0.006022589392325213183, 0.01254516766564344951, 0.01580645680230256811, 0.01906774593896168671, 0.02559032421227992043, 0.03211290248559815763 ),
 ( 0.000000000000000000, 1.000000000000000000 ),
 .UNSPECIFIED. ) 
 GEOMETRIC_REPRESENTATION_ITEM ( )  RATIONAL_B_SPLINE_SURFACE ( (
 ( 1.000000000000000000, 0.9998834880171258988, 1.000000000000000000),
 ( 1.000000000000000000, 0.9998139205012247510, 1.000000000000000000),
 ( 1.000000000000000000, 0.9997315632444677691, 1.000000000000000000),
 ( 1.000000000000000000, 0.9996405464946958030, 1.000000000000000000),
 ( 1.000000000000000000, 0.9996155081776925133, 1.000000000000000000),
 ( 1.000000000000000000, 0.9995814087511105672, 1.000000000000000000),
 ( 1.000000000000000000, 0.9995724100939918921, 1.000000000000000000),
 ( 1.000000000000000000, 0.9995726760936894939, 1.000000000000000000),
 ( 1.000000000000000000, 0.9996103361816741639, 1.000000000000000000),
 ( 1.000000000000000000, 0.9997312749796802844, 1.000000000000000000),
 ( 1.000000000000000000, 0.9998135910914284219, 1.000000000000000000),
 ( 1.000000000000000000, 0.9998834880173383954, 1.000000000000000000) ) ) 
 REPRESENTATION_ITEM ( '' )  SURFACE ( )  );
#11401 = DIRECTION ( 'NONE',  ( 0.000000000000000000, 1.000000000000000000, 0.000000000000000000 ) ) ;
#11402 = CARTESIAN_POINT ( 'NONE',  ( 200.0000000000000000, 39.99999999999999289, 20.00000000000007105 ) ) ;
#11403 = CARTESIAN_POINT ( 'NONE',  ( 170.2234770963711128, 1.169953928977015745E-13, -24.55285855007187124 ) ) ;
#11404 = EDGE_CURVE ( 'NONE', #16682, #17385, #1004, .T. ) ;
#11405 = CARTESIAN_POINT ( 'NONE',  ( 12.01676479903289874, 49.30523874212545365, -14.17570730777195998 ) ) ;
#11406 = CARTESIAN_POINT ( 'NONE',  ( -30.26275506840323004, -41.69427246844629309, 40.00000000000002132 ) ) ;
#11408 = CARTESIAN_POINT ( 'NONE',  ( -599.5988719536647977, 38.07837741337411330, -12.25825338881973359 ) ) ;
#11407 = CARTESIAN_POINT ( 'NONE',  ( -151.4802930568858415, 11.09498731357607504, -33.96623840857670729 ) ) ;
#11409 = EDGE_CURVE ( 'NONE', #12267, #6802, #6576, .T. ) ;
#11410 = CARTESIAN_POINT ( 'NONE',  ( 130.8568914410475088, -5.949712681206671405, 40.00000000000002132 ) ) ;
#11411 = CARTESIAN_POINT ( 'NONE',  ( -208.1127848780265026, -10.60833733269551971, 10.60833733269537049 ) ) ;
#11412 = CARTESIAN_POINT ( 'NONE',  ( 57.59792236341147031, -2.435789363418150444, 0.000000000000000000 ) ) ;
#11413 = CARTESIAN_POINT ( 'NONE',  ( -198.0356074513804572, 40.00000000000014921, -15.37879056873028816 ) ) ;
#11414 = CARTESIAN_POINT ( 'NONE',  ( 57.59792236341148453, -40.00000000000003553, 2.435789363417741438 ) ) ;
#11415 = CARTESIAN_POINT ( 'NONE',  ( -16.41594856550787895, -39.35878123526666172, 21.03672846785433137 ) ) ;
#11416 = ADVANCED_FACE ( 'NONE', ( #10848 ), #4740, .T. ) ;
#11417 = ADVANCED_FACE ( 'NONE', ( #11108 ), #22960, .T. ) ;
#11418 = VERTEX_POINT ( 'NONE', #17217 ) ;
#11420 = CARTESIAN_POINT ( 'NONE',  ( -3.675706741948014500, 43.24173023805430205, -17.91131112508040601 ) ) ;
#11419 = DIRECTION ( 'NONE',  ( 0.000000000000000000, -0.000000000000000000, 1.000000000000000000 ) ) ;
#11421 = CARTESIAN_POINT ( 'NONE',  ( -259.2033419157646676, -30.48217210827744950, 40.00000000000002132 ) ) ;
#11422 = CARTESIAN_POINT ( 'NONE',  ( -114.6379801953803650, 5.502459769868860207, -21.35001481053563666 ) ) ;
#11423 = DIRECTION ( 'NONE',  ( 0.000000000000000000, 0.000000000000000000, 1.000000000000000000 ) ) ;
#11424 = EDGE_LOOP ( 'NONE', ( #16041, #9830 ) ) ;
#11425 = ORIENTED_EDGE ( 'NONE', *, *, #19566, .T. ) ;
#11426 = DIRECTION ( 'NONE',  ( -0.000000000000000000, -1.321694076934715579E-16, -1.000000000000000000 ) ) ;
#11427 = DIRECTION ( 'NONE',  ( 0.000000000000000000, 1.000000000000000000, 0.000000000000000000 ) ) ;
#11428 = AXIS2_PLACEMENT_3D ( 'NONE', #10790, #17028, #18900 ) ;
#11429 = CARTESIAN_POINT ( 'NONE',  ( -215.0000000000000284, 72.72568232011437317, -59.67546976104961942 ) ) ;
#11430 = ORIENTED_EDGE ( 'NONE', *, *, #19467, .F. ) ;
#11431 = CARTESIAN_POINT ( 'NONE',  ( 199.0263730241462099, -14.60190056250242030, 13.67829565473005715 ) ) ;
#11432 = CARTESIAN_POINT ( 'NONE',  ( -126.6834156230595454, 11.16464796290217087, -24.04426801068344588 ) ) ;
#11433 = CARTESIAN_POINT ( 'NONE',  ( 136.1360204305621551, 31.79587985999267374, -24.77266263493117293 ) ) ;
#11434 = CARTESIAN_POINT ( 'NONE',  ( -121.8281150758585341, -22.46071699780029363, -10.16552079116060803 ) ) ;
#11435 = CARTESIAN_POINT ( 'NONE',  ( -30.26275506840324070, -1.147469862568086380E-14, 1.694272468446259783 ) ) ;
#11436 = CARTESIAN_POINT ( 'NONE',  ( -105.3174402647060361, -10.86264740497938242, -18.50711184654230479 ) ) ;
#11437 = DIRECTION ( 'NONE',  ( 0.000000000000000000, 0.000000000000000000, 1.000000000000000000 ) ) ;
#11438 = DIRECTION ( 'NONE',  ( 0.000000000000000000, 0.000000000000000000, 1.000000000000000000 ) ) ;
#11439 = CARTESIAN_POINT ( 'NONE',  ( -105.3755690713226585, -39.99999999999985079, -18.24025645688394448 ) ) ;
#11440 = CARTESIAN_POINT ( 'NONE',  ( 163.1118516004056573, 40.00000000000017764, -12.73709011382432976 ) ) ;
#11441 = CARTESIAN_POINT ( 'NONE',  ( -110.0822598093819522, -11.09289860105409353, 16.86905266169973316 ) ) ;
#11442 = CARTESIAN_POINT ( 'NONE',  ( -162.0762913951020892, -1.198031840385783919, 1.198031840385741731 ) ) ;
#11443 = CARTESIAN_POINT ( 'NONE',  ( 146.6084372240433709, 40.00000000000017053, -34.62501878078291639 ) ) ;
#11444 = CARTESIAN_POINT ( 'NONE',  ( 199.9999999999999432, 14.14213562373113398, -14.14213562373094923 ) ) ;
#11445 = CARTESIAN_POINT ( 'NONE',  ( 200.0000000000000284, -82.49999999999990052, 52.49999999999977973 ) ) ;
#11446 = CARTESIAN_POINT ( 'NONE',  ( -77.90255099906853786, 8.644468104252323926, -20.04994828524279882 ) ) ;
#11447 = CARTESIAN_POINT ( 'NONE',  ( -280.0000000000000000, 14.14213562373098299, -14.14213562373088706 ) ) ;
#11448 = CARTESIAN_POINT ( 'NONE',  ( -259.2033419157646676, -1.438356298054549103E-14, -9.517827891722632216 ) ) ;
#11449 = CARTESIAN_POINT ( 'NONE',  ( -280.0000000000000568, -14.14213562373108601, 42.42640687119285303 ) ) ;
#11450 = CARTESIAN_POINT ( 'NONE',  ( -135.8532207217289738, -50.09629031063973770, 6.472252184283735943 ) ) ;
#11451 = CARTESIAN_POINT ( 'NONE',  ( -144.1957134277073465, -12.48102206811670811, -30.13185274890651399 ) ) ;
#11452 = DIRECTION ( 'NONE',  ( 0.000000000000000000, 0.000000000000000000, 1.000000000000000000 ) ) ;
#11453 = VERTEX_POINT ( 'NONE', #9490 ) ;
#11454 = CARTESIAN_POINT ( 'NONE',  ( 151.7948205124836250, 4.785054706301759886, -4.785054706301612448 ) ) ;
#11455 = DIRECTION ( 'NONE',  ( 1.000000000000000000, 1.836970198721030427E-16, -0.000000000000000000 ) ) ;
#11456 =( BOUNDED_CURVE ( )  B_SPLINE_CURVE ( 3, ( #3023, #5399, #11130, #26299 ),
 .UNSPECIFIED., .F., .T. ) 
 B_SPLINE_CURVE_WITH_KNOTS ( ( 4, 4 ),
 ( 0.4999406519327141418, 0.5000000000000000000 ),
 .UNSPECIFIED. ) 
 CURVE ( )  GEOMETRIC_REPRESENTATION_ITEM ( )  RATIONAL_B_SPLINE_CURVE ( ( 1.000000000000000000, 0.9998807446028390444, 0.9997615105384527467, 0.9996422978068409959 ) ) 
 REPRESENTATION_ITEM ( '' )  );
#11457 = CARTESIAN_POINT ( 'NONE',  ( -625.7632191285248382, 28.30420643832251670, 34.98391645891658186 ) ) ;
#11458 = EDGE_LOOP ( 'NONE', ( #14554, #17516 ) ) ;
#11459 = CARTESIAN_POINT ( 'NONE',  ( 192.4448373802100889, -1.741373372144848397E-13, 20.00000000003942091 ) ) ;
#11460 = CARTESIAN_POINT ( 'NONE',  ( 199.0233445383804565, -20.00362565020445871, -0.01023483319826397862 ) ) ;
#11461 = CARTESIAN_POINT ( 'NONE',  ( -62.72988123315806064, 10.50767649796025616, 25.36777511002372876 ) ) ;
#11462 = VERTEX_POINT ( 'NONE', #15727 ) ;
#11463 = EDGE_LOOP ( 'NONE', ( #2512, #683, #18170, #10535, #5319, #9836 ) ) ;
#11464 = CARTESIAN_POINT ( 'NONE',  ( 0.2972598230769976091, -10.13633138497479180, 10.13633138497468522 ) ) ;
#11465 = CARTESIAN_POINT ( 'NONE',  ( 91.82158438592156813, 39.99999999999995737, 22.79471317813484887 ) ) ;
#11466 = DIRECTION ( 'NONE',  ( 0.000000000000000000, -0.9307566067258455922, 0.3656393565197673112 ) ) ;
#11467 = CIRCLE ( 'NONE', #9354, 14.99999999999999822 ) ;
#11468 = CARTESIAN_POINT ( 'NONE',  ( -200.0000000000001421, -14.17215463606902404, -49.28189405767602693 ) ) ;
#11469 = CARTESIAN_POINT ( 'NONE',  ( -280.0000000000000000, -1.237140859393462838E-13, 20.00000000000001421 ) ) ;
#11470 = CARTESIAN_POINT ( 'NONE',  ( 199.9999999999999147, -18.99336422956244874, -0.7807574862979690389 ) ) ;
#11471 = CARTESIAN_POINT ( 'NONE',  ( 91.82158438592158234, 7.693928927950222250E-14, -17.20528682183300262 ) ) ;
#11472 = CARTESIAN_POINT ( 'NONE',  ( -716.9846540392142060, -66.50000000000001421, -66.50000000000005684 ) ) ;
#11473 = CARTESIAN_POINT ( 'NONE',  ( -5.787027468458424195, -17.67457596682273291, -42.67020100828553808 ) ) ;
#11474 = CARTESIAN_POINT ( 'NONE',  ( 184.8905102610680444, 43.07788698682591644, -13.49065550809769221 ) ) ;
#11475 = CARTESIAN_POINT ( 'NONE',  ( -77.90255099906769942, -20.29001641120661859, 8.064892378658379712 ) ) ;
#11476 = CARTESIAN_POINT ( 'NONE',  ( -135.8532207217289738, -39.99999999999972289, -30.84685318188688541 ) ) ;
#11477 = CARTESIAN_POINT ( 'NONE',  ( 85.88525995977231275, -23.37195345543618430, -8.769880559910854245 ) ) ;
#11478 = CARTESIAN_POINT ( 'NONE',  ( 184.8905102610680444, -19.07866798485554938, 40.00000000000002132 ) ) ;
#11479 = CARTESIAN_POINT ( 'NONE',  ( -208.1127848780264742, -55.00245453014425578, -40.00000000000002132 ) ) ;
#11480 = CARTESIAN_POINT ( 'NONE',  ( -198.0356074513804572, 17.40982414986446969, 39.15871834505921356 ) ) ;
#11481 = CARTESIAN_POINT ( 'NONE',  ( 14.38125909742181285, -15.17850393972633505, -40.00000000000002132 ) ) ;
#11483 = CARTESIAN_POINT ( 'NONE',  ( -83.21262154144233136, 13.72187187059966895, -33.12752917119015450 ) ) ;
#11482 = CARTESIAN_POINT ( 'NONE',  ( -1.815588850254795217, -43.60036197523984924, -23.89016120430183676 ) ) ;
#11484 = CARTESIAN_POINT ( 'NONE',  ( -192.9588430854689989, 1.161019517985663313E-13, -14.46834944099969533 ) ) ;
#11485 = CARTESIAN_POINT ( 'NONE',  ( 184.8905102610680444, -14.79361573936389540, 41.77492675555996016 ) ) ;
#11486 = CARTESIAN_POINT ( 'NONE',  ( -280.0000000000000568, 19.99999999999996447, -40.00000000000002132 ) ) ;
#11487 = ORIENTED_EDGE ( 'NONE', *, *, #1162, .F. ) ;
#11488 = CARTESIAN_POINT ( 'NONE',  ( 23.42154907652887630, -46.79103593565392316, 13.79745687233760876 ) ) ;
#11489 = SPHERICAL_SURFACE ( 'NONE', #22332, 15.00000000000000000 ) ;
#11490 = CARTESIAN_POINT ( 'NONE',  ( -105.3755690713226585, -15.38646221621796251, 41.18208027870593924 ) ) ;
#11491 = CARTESIAN_POINT ( 'NONE',  ( 0.2972598230769957217, -4.999556039334937811E-14, 14.33493731733933352 ) ) ;
#11492 = AXIS2_PLACEMENT_3D ( 'NONE', #9440, #1081, #25435 ) ;
#11493 = FACE_OUTER_BOUND ( 'NONE', #19677, .T. ) ;
#11494 = B_SPLINE_CURVE_WITH_KNOTS ( 'NONE', 3,
 ( #21307, #5082, #17172, #11063, #7065, #13431 ),
 .UNSPECIFIED., .F., .F.,
 ( 4, 2, 4 ),
 ( -6.000000002287634284E-08, 0.04017169446089188106, 0.08034344892178377218 ),
 .UNSPECIFIED. ) ;
#11495 = CARTESIAN_POINT ( 'NONE',  ( 91.82158438592158234, 22.79471317813472453, -40.00000000000002132 ) ) ;
#11496 = VECTOR ( 'NONE', #1076, 1000.000000000000000 ) ;
#11497 = CIRCLE ( 'NONE', #3444, 75.00000000000000000 ) ;
#11498 = CARTESIAN_POINT ( 'NONE',  ( -114.4098922876147384, 20.15198150140922451, 8.347224046571190215 ) ) ;
#11499 = CARTESIAN_POINT ( 'NONE',  ( 200.0000000000000284, -9.508146755684434126, 16.46234680784547777 ) ) ;
#11500 = ADVANCED_BREP_SHAPE_REPRESENTATION ( '', ( #8871, #21058 ), #7428 ) ;
#11501 = EDGE_CURVE ( 'NONE', #9531, #1858, #20543, .T. ) ;
#11502 = CARTESIAN_POINT ( 'NONE',  ( -77.90255099906772784, 8.064892378658852223, -20.29001641120641608 ) ) ;
#11503 = CARTESIAN_POINT ( 'NONE',  ( 170.0000000000000000, -24.95097643316997704, 0.000000000000000000 ) ) ;
#11504 = CARTESIAN_POINT ( 'NONE',  ( -192.9588430854690273, -10.23066800231931239, -66.79921049724377724 ) ) ;
#11505 = CARTESIAN_POINT ( 'NONE',  ( -105.2050109279299761, 21.49594509020261413, -0.1304588126430248907 ) ) ;
#11506 = CARTESIAN_POINT ( 'NONE',  ( -77.78761611110736851, 9.949180589398501695, -19.59005896965153326 ) ) ;
#11507 = CARTESIAN_POINT ( 'NONE',  ( 0.2972598230770048811, -10.13633138497415942, -66.70487387989865624 ) ) ;
#11509 = CARTESIAN_POINT ( 'NONE',  ( -198.0356074513804572, 10.87444709759730088, -10.87444709759707173 ) ) ;
#11508 = CARTESIAN_POINT ( 'NONE',  ( -198.0356074513804572, -10.87444709758429262, -67.44298959250878056 ) ) ;
#11510 = CARTESIAN_POINT ( 'NONE',  ( -162.0762913951020892, 1.198031840385732849, -1.198031840385733515 ) ) ;
#11511 = CARTESIAN_POINT ( 'NONE',  ( -105.2940237833718982, -11.46076537570947451, 18.12284447398040754 ) ) ;
#11512 = FACE_BOUND ( 'NONE', #15071, .T. ) ;
#11513 = CARTESIAN_POINT ( 'NONE',  ( -100.7734535825088500, -40.00000000000009948, 17.32597176626796909 ) ) ;
#11514 = CARTESIAN_POINT ( 'NONE',  ( -56.48582580120559271, 6.472252184284121412, 6.472252184284244869 ) ) ;
#11515 = CIRCLE ( 'NONE', #12838, 15.00000000000000000 ) ;
#11516 = CARTESIAN_POINT ( 'NONE',  ( 151.7948205124836534, -33.23291073765550863, 40.00000000000002132 ) ) ;
#11517 = ORIENTED_EDGE ( 'NONE', *, *, #7185, .T. ) ;
#11518 = CARTESIAN_POINT ( 'NONE',  ( 184.8905102610680444, 13.49065550809817715, -43.07788698682574591 ) ) ;
#11519 = CARTESIAN_POINT ( 'NONE',  ( -19.45810057983592500, 38.38097177479090760, 15.89791904617739249 ) ) ;
#11520 = CARTESIAN_POINT ( 'NONE',  ( 83.06440094989142153, 9.006081069517801296, 24.44702070087263834 ) ) ;
#11521 = CARTESIAN_POINT ( 'NONE',  ( -4.121597284766468583, -46.96202426942434727, -13.82232031191962562 ) ) ;
#11522 = VERTEX_POINT ( 'NONE', #23985 ) ;
#11523 = CARTESIAN_POINT ( 'NONE',  ( -197.4154352060510575, -44.73190714601606288, 24.72550168626919742 ) ) ;
#11524 = CARTESIAN_POINT ( 'NONE',  ( 199.9999999999999147, -10.43683117453143261, -15.88259547814976180 ) ) ;
#11525 = CARTESIAN_POINT ( 'NONE',  ( 23.25494099740784293, -17.82744980609922791, 43.03927110441377124 ) ) ;
#11526 = CARTESIAN_POINT ( 'NONE',  ( 98.29820294269173075, 19.99999999998819433, -2.308575297063409524E-13 ) ) ;
#11527 = CARTESIAN_POINT ( 'NONE',  ( 199.0056892241198625, 17.33029760820262410, -9.978133259584877734 ) ) ;
#11528 = CONICAL_SURFACE ( 'NONE', #20061, 60.00000000000000000, 0.7853981633974447263 ) ;
#11529 = CARTESIAN_POINT ( 'NONE',  ( -87.08627934007971305, 21.18514689813062191, 3.496387290698740102 ) ) ;
#11530 = CARTESIAN_POINT ( 'NONE',  ( 91.82158438592156813, 39.99999999999995737, 22.79471317813484887 ) ) ;
#11531 = CARTESIAN_POINT ( 'NONE',  ( -87.13361725325452767, -1.359581015579222063, 21.49321519332998065 ) ) ;
#11532 = CARTESIAN_POINT ( 'NONE',  ( 1.564252679174713778, 48.56509332159259884, -14.06374044400957501 ) ) ;
#11533 = CARTESIAN_POINT ( 'NONE',  ( 130.8568914410475088, 34.05028731879790627, 40.00000000000002132 ) ) ;
#11535 = CARTESIAN_POINT ( 'NONE',  ( -626.9846540392142060, 26.45751311064579880, -30.00000000000005329 ) ) ;
#11534 = DIRECTION ( 'NONE',  ( 1.000000000000000000, 1.836970198721030181E-16, -0.000000000000000000 ) ) ;
#11536 = CARTESIAN_POINT ( 'NONE',  ( -162.0762913951020892, -1.694272876828353702, 0.000000000000000000 ) ) ;
#11537 = CARTESIAN_POINT ( 'NONE',  ( 163.1118516004056573, 27.26290988616876021, -40.00000000000002132 ) ) ;
#11538 = CARTESIAN_POINT ( 'NONE',  ( -86.96347745069644475, -21.75974354311651737, 0.000000000000000000 ) ) ;
#11539 = CARTESIAN_POINT ( 'NONE',  ( -280.0000000000000568, 40.00000000000017764, -19.99999999999959144 ) ) ;
#11540 = CARTESIAN_POINT ( 'NONE',  ( -56.48582580120559271, -1.062504017861011783E-13, 9.153146818113587102 ) ) ;
#11541 = CARTESIAN_POINT ( 'NONE',  ( 113.0017353590611293, -23.76250624610700513, -9.842752363112978742 ) ) ;
#11542 = EDGE_LOOP ( 'NONE', ( #9316, #8733, #6468, #5451 ) ) ;
#11544 = CARTESIAN_POINT ( 'NONE',  ( -3.449394506061540966, 43.30266483527620380, -17.93655106166781366 ) ) ;
#11543 = CARTESIAN_POINT ( 'NONE',  ( -4.039451493210481026, -46.99046209229813797, 13.82811171175447917 ) ) ;
#11545 = CARTESIAN_POINT ( 'NONE',  ( 170.2234770963711128, -15.44714144992812876, -2.449293598294708485E-15 ) ) ;
#11546 = CARTESIAN_POINT ( 'NONE',  ( -114.4364955367328491, -20.29001642038857156, 8.064892380842218600 ) ) ;
#11547 = FACE_OUTER_BOUND ( 'NONE', #15453, .T. ) ;
#11548 = ORIENTED_EDGE ( 'NONE', *, *, #19960, .T. ) ;
#11549 = ORIENTED_EDGE ( 'NONE', *, *, #13205, .T. ) ;
#11550 = AXIS2_PLACEMENT_3D ( 'NONE', #7338, #1110, #5109 ) ;
#11551 = DIRECTION ( 'NONE',  ( 1.000000000000000000, 1.836970198721030427E-16, -0.000000000000000000 ) ) ;
#11552 = LINE ( 'NONE', #15179, #8107 ) ;
#11553 = ORIENTED_EDGE ( 'NONE', *, *, #13932, .T. ) ;
#11554 = ORIENTED_EDGE ( 'NONE', *, *, #18389, .F. ) ;
#11555 = EDGE_CURVE ( 'NONE', #13654, #8031, #9740, .T. ) ;
#11556 = ORIENTED_EDGE ( 'NONE', *, *, #6961, .T. ) ;
#11557 = CARTESIAN_POINT ( 'NONE',  ( 199.9999999999997726, -5.383989893674753446, 18.23209102328170061 ) ) ;
#11558 = FACE_OUTER_BOUND ( 'NONE', #11542, .T. ) ;
#11559 = CARTESIAN_POINT ( 'NONE',  ( -30.26275506840325136, 57.76657404653985139, 1.198031551616126178 ) ) ;
#11560 = EDGE_CURVE ( 'NONE', #4752, #11180, #11009, .T. ) ;
#11561 = DIRECTION ( 'NONE',  ( 1.000000000000000000, 1.836970198721030181E-16, -0.000000000000000000 ) ) ;
#11562 = CARTESIAN_POINT ( 'NONE',  ( 14.38125909742181108, -5.035366881890652543E-14, 15.17850393972633682 ) ) ;
#11563 = CARTESIAN_POINT ( 'NONE',  ( 12.01361943528961262, -14.17591515420103754, 49.30661675909298935 ) ) ;
#11564 = PLANE ( 'NONE',  #6847 ) ;
#11565 = EDGE_CURVE ( 'NONE', #11184, #23643, #5249, .T. ) ;
#11566 = EDGE_CURVE ( 'NONE', #4257, #16610, #19470, .T. ) ;
#11567 = DIRECTION ( 'NONE',  ( -1.000000000000000000, 1.836970198721030181E-16, 0.000000000000000000 ) ) ;
#11568 = CARTESIAN_POINT ( 'NONE',  ( 4.995406935893290878, 1.606505379428369110E-13, -15.24977328854832592 ) ) ;
#11569 = CARTESIAN_POINT ( 'NONE',  ( -280.0000000000000568, -39.99999999999987210, -20.00000000000043343 ) ) ;
#11570 = CARTESIAN_POINT ( 'NONE',  ( -114.6659165474107311, -11.80608088190434302, 18.60032035379251170 ) ) ;
#11571 = CARTESIAN_POINT ( 'NONE',  ( 146.6084372240433709, -3.800685668858344801, -52.76785682606520567 ) ) ;
#11572 = CARTESIAN_POINT ( 'NONE',  ( -280.0000000000000000, 1.839446121267387017E-14, -20.00000000000001421 ) ) ;
#11573 = CARTESIAN_POINT ( 'NONE',  ( 14.38125909742181818, -39.01709431150904095, -17.55144818341490165 ) ) ;
#11574 = CARTESIAN_POINT ( 'NONE',  ( 144.1620285550791323, 30.21661402164551191, 12.51613133675876810 ) ) ;
#11575 = CARTESIAN_POINT ( 'NONE',  ( -4.039451493210481026, -46.99046209229813797, 13.82811171175447917 ) ) ;
#11576 = CARTESIAN_POINT ( 'NONE',  ( -208.1127848780265026, -10.60833733269551971, 10.60833733269537049 ) ) ;
#11577 = CARTESIAN_POINT ( 'NONE',  ( -86.96347745069643054, -39.99999999999995737, -21.75974354311664527 ) ) ;
#11578 = CARTESIAN_POINT ( 'NONE',  ( -280.0000000000000000, 14.14213562373088351, 14.14213562373098654 ) ) ;
#11579 = CARTESIAN_POINT ( 'NONE',  ( 130.8568914410475372, -4.207082182992785135, -4.207082182992884611 ) ) ;
#11580 = CARTESIAN_POINT ( 'NONE',  ( -166.3490736461069446, -19.13702016934220040, -36.43932733823757530 ) ) ;
#11581 = CARTESIAN_POINT ( 'NONE',  ( -77.58504658027047185, 13.57343625279989219, 17.50303174137573592 ) ) ;
#11582 = ORIENTED_EDGE ( 'NONE', *, *, #23315, .F. ) ;
#11583 = CARTESIAN_POINT ( 'NONE',  ( 151.7948205124836534, 33.06932595376333239, 23.49921654116065284 ) ) ;
#11584 = CARTESIAN_POINT ( 'NONE',  ( 184.8905102610680444, 20.92133201514447549, 0.000000000000000000 ) ) ;
#11585 = DIRECTION ( 'NONE',  ( 0.000000000000000000, 1.000000000000000000, 0.000000000000000000 ) ) ;
#11586 = CARTESIAN_POINT ( 'NONE',  ( -102.2610585947572872, 22.27377874548541925, -0.000000000000000000 ) ) ;
#11587 = VERTEX_POINT ( 'NONE', #17595 ) ;
#11588 = CARTESIAN_POINT ( 'NONE',  ( -213.1075012329537230, 1.045191102001431893E-13, -13.71589010951911902 ) ) ;
#11589 = CARTESIAN_POINT ( 'NONE',  ( 199.0227794283635205, -19.94987460103941501, -1.494179565802910670 ) ) ;
#11590 = CARTESIAN_POINT ( 'NONE',  ( 18.89824403360313099, -43.99464769172834622, 24.18164459663369925 ) ) ;
#11591 = EDGE_LOOP ( 'NONE', ( #21044, #9089, #4623, #2731 ) ) ;
#11592 = PRODUCT_DEFINITION ( 'UNKNOWN', '', #2813, #25476 ) ;
#11593 = ORIENTED_EDGE ( 'NONE', *, *, #21349, .T. ) ;
#11594 = EDGE_CURVE ( 'NONE', #6393, #19936, #22057, .T. ) ;
#11595 = CARTESIAN_POINT ( 'NONE',  ( 136.1360204305621551, 4.966164525587093870, -40.00000000000002132 ) ) ;
#11596 = CARTESIAN_POINT ( 'NONE',  ( -213.1075012329537230, -37.98287015391232302, -18.58567234101164800 ) ) ;
#11597 = CARTESIAN_POINT ( 'NONE',  ( 200.0000000000000000, 39.99999999999999289, 20.00000000000007105 ) ) ;
#11598 = LINE ( 'NONE', #1639, #22754 ) ;
#11599 = DIRECTION ( 'NONE',  ( -0.000000000000000000, -1.000000000000000000, -0.000000000000000000 ) ) ;
#11600 = CARTESIAN_POINT ( 'NONE',  ( 0.2972598230769957217, 1.502051041545559470E-13, -14.33493731733933352 ) ) ;
#11601 = CARTESIAN_POINT ( 'NONE',  ( -105.3755690713226727, -8.549198663894545631E-14, 18.24025645688352881 ) ) ;
#11602 = CARTESIAN_POINT ( 'NONE',  ( 200.0000000000000853, -8.685123034760072969, -16.90575535186691880 ) ) ;
#11603 = CARTESIAN_POINT ( 'NONE',  ( -238.4067589809705794, -4.716212492215116094E-14, 0.9644942799825824142 ) ) ;
#11604 = B_SPLINE_CURVE_WITH_KNOTS ( 'NONE', 3,
 ( #9650, #1283, #17621, #7771, #3533, #15752 ),
 .UNSPECIFIED., .F., .F.,
 ( 4, 2, 4 ),
 ( 0.0003134778200527471104, 0.004479062015275551457, 0.008644646210498357214 ),
 .UNSPECIFIED. ) ;
#11605 = CARTESIAN_POINT ( 'NONE',  ( 0.000000000000000000, 0.000000000000000000, 0.000000000000000000 ) ) ;
#11606 = CARTESIAN_POINT ( 'NONE',  ( -7.769366557094651959, -13.56374645826313063, -45.69637362128903391 ) ) ;
#11607 = CARTESIAN_POINT ( 'NONE',  ( -100.7734535825088500, 44.31723036834907958, -12.25131212657445801 ) ) ;
#11608 =( BOUNDED_SURFACE ( )  B_SPLINE_SURFACE ( 3, 3, ( 
 ( #7982, #11448, #26247, #11982, #21702, #20106, #3479, #3603, #25840, #11712, #13575, #3741, #1883, #5730, #19697, #17568, #9987, #19832, #3348, #13972, #9725, #17827, #1618, #25974, #23820, #26106, #18098, #9461, #13455, #7714 ),
 ( #15825, #22106, #25705, #19571, #3882, #23955, #16100, #7456, #24232, #9590, #21574, #13834, #11577, #15571, #11846, #21969, #19967, #1748, #9856, #1485, #1362, #23695, #17959, #7844, #5602, #15966, #5475, #13709, #24091, #5866 ),
 ( #17695, #7584, #15696, #21834, #14504, #10657, #8250, #16636, #8518, #24368, #275, #16367, #8654, #20372, #10123, #12644, #4016, #24765, #24630, #22766, #24501, #22508, #18366, #6518, #12116, #18631, #14113, #146, #6131, #14375 ),
 ( #16762, #6262, #4286, #6388, #22241, #22635, #14629, #12250, #12375, #18224, #18766, #6005, #8383, #20240, #10384, #16505, #4546, #20769, #12504, #2147, #4410, #11, #20503, #10257, #8122, #2275, #18495, #14239, #550, #2021 ),
 ( #20632, #2539, #16239, #2407, #22379, #4155, #10517, #414, #4675, #6651, #14766, #22896, #24896, #12777, #2682, #18899, #20904, #678, #10789, #8787, #19598, #4008, #25730, #21599, #14367, #9486, #24493, #16230, #2011, #6254 ),
 ( #8114, #24359, #6123, #22498, #25864, #4277, #10376, #12107, #13477, #1385, #137, #14231, #10249, #8376, #3370, #5499, #8241, #5997, #14103, #18487, #3505, #13599, #24223, #22232, #23718, #20232, #15723, #19727, #22371, #1514 ),
 ( #16359, #17590, #11603, #10116, #268, #2, #21729, #18216, #4147, #20364, #12240, #2138, #18358, #12367, #20495, #9619, #2268, #17723, #23594, #5372, #11471, #7480, #15593, #7608, #4537, #20624, #16498, #804, #19149, #2531 ) ),
 .UNSPECIFIED., .T., .F., .F. ) 
 B_SPLINE_SURFACE_WITH_KNOTS ( ( 4, 3, 4 ),
 ( 4, 2, 2, 2, 2, 2, 2, 2, 2, 2, 2, 2, 2, 2, 4 ),
 ( 0.000000000000000000, 0.5000000000000000000, 1.000000000000000000 ),
 ( 0.000000000000000000, 0.1357259735107005372, 0.1651108541090157700, 0.1944957347073310028, 0.3598804999793158710, 0.3867117631979620773, 0.4135430264166082281, 0.5789277916885930964, 0.6062785021374117456, 0.6336292125862302838, 0.8508620842112317728, 0.8814014469398914198, 0.9119408096685510667, 0.9559704048342755334, 1.000000000000000000 ),
 .UNSPECIFIED. ) 
 GEOMETRIC_REPRESENTATION_ITEM ( )  RATIONAL_B_SPLINE_SURFACE ( (
 ( 1.000000000000000000, 1.000000000000000000, 1.000000000000000000, 1.000000000000000000, 1.000000000000000000, 1.000000000000000000, 1.000000000000000000, 1.000000000000000000, 1.000000000000000000, 1.000000000000000000, 1.000000000000000000, 1.000000000000000000, 1.000000000000000000, 1.000000000000000000, 1.000000000000000000, 1.000000000000000000, 1.000000000000000000, 1.000000000000000000, 1.000000000000000000, 1.000000000000000000, 1.000000000000000000, 1.000000000000000000, 1.000000000000000000, 1.000000000000000000, 1.000000000000000000, 1.000000000000000000, 1.000000000000000000, 1.000000000000000000, 1.000000000000000000, 1.000000000000000000),
 ( 0.3333333333333333703, 0.3333333333333333703, 0.3333333333333333703, 0.3333333333333333703, 0.3333333333333333703, 0.3333333333333333703, 0.3333333333333333703, 0.3333333333333333703, 0.3333333333333333703, 0.3333333333333333703, 0.3333333333333333703, 0.3333333333333333703, 0.3333333333333333703, 0.3333333333333333703, 0.3333333333333333703, 0.3333333333333333703, 0.3333333333333333703, 0.3333333333333333703, 0.3333333333333333703, 0.3333333333333333703, 0.3333333333333333703, 0.3333333333333333703, 0.3333333333333333703, 0.3333333333333333703, 0.3333333333333333703, 0.3333333333333333703, 0.3333333333333333703, 0.3333333333333333703, 0.3333333333333333703, 0.3333333333333333703),
 ( 0.3333333333333333703, 0.3333333333333333703, 0.3333333333333333703, 0.3333333333333333703, 0.3333333333333333703, 0.3333333333333333703, 0.3333333333333333703, 0.3333333333333333703, 0.3333333333333333703, 0.3333333333333333703, 0.3333333333333333703, 0.3333333333333333703, 0.3333333333333333703, 0.3333333333333333703, 0.3333333333333333703, 0.3333333333333333703, 0.3333333333333333703, 0.3333333333333333703, 0.3333333333333333703, 0.3333333333333333703, 0.3333333333333333703, 0.3333333333333333703, 0.3333333333333333703, 0.3333333333333333703, 0.3333333333333333703, 0.3333333333333333703, 0.3333333333333333703, 0.3333333333333333703, 0.3333333333333333703, 0.3333333333333333703),
 ( 1.000000000000000000, 1.000000000000000000, 1.000000000000000000, 1.000000000000000000, 1.000000000000000000, 1.000000000000000000, 1.000000000000000000, 1.000000000000000000, 1.000000000000000000, 1.000000000000000000, 1.000000000000000000, 1.000000000000000000, 1.000000000000000000, 1.000000000000000000, 1.000000000000000000, 1.000000000000000000, 1.000000000000000000, 1.000000000000000000, 1.000000000000000000, 1.000000000000000000, 1.000000000000000000, 1.000000000000000000, 1.000000000000000000, 1.000000000000000000, 1.000000000000000000, 1.000000000000000000, 1.000000000000000000, 1.000000000000000000, 1.000000000000000000, 1.000000000000000000),
 ( 0.3333333333333333703, 0.3333333333333333703, 0.3333333333333333703, 0.3333333333333333703, 0.3333333333333333703, 0.3333333333333333703, 0.3333333333333333703, 0.3333333333333333703, 0.3333333333333333703, 0.3333333333333333703, 0.3333333333333333703, 0.3333333333333333703, 0.3333333333333333703, 0.3333333333333333703, 0.3333333333333333703, 0.3333333333333333703, 0.3333333333333333703, 0.3333333333333333703, 0.3333333333333333703, 0.3333333333333333703, 0.3333333333333333703, 0.3333333333333333703, 0.3333333333333333703, 0.3333333333333333703, 0.3333333333333333703, 0.3333333333333333703, 0.3333333333333333703, 0.3333333333333333703, 0.3333333333333333703, 0.3333333333333333703),
 ( 0.3333333333333333703, 0.3333333333333333703, 0.3333333333333333703, 0.3333333333333333703, 0.3333333333333333703, 0.3333333333333333703, 0.3333333333333333703, 0.3333333333333333703, 0.3333333333333333703, 0.3333333333333333703, 0.3333333333333333703, 0.3333333333333333703, 0.3333333333333333703, 0.3333333333333333703, 0.3333333333333333703, 0.3333333333333333703, 0.3333333333333333703, 0.3333333333333333703, 0.3333333333333333703, 0.3333333333333333703, 0.3333333333333333703, 0.3333333333333333703, 0.3333333333333333703, 0.3333333333333333703, 0.3333333333333333703, 0.3333333333333333703, 0.3333333333333333703, 0.3333333333333333703, 0.3333333333333333703, 0.3333333333333333703),
 ( 1.000000000000000000, 1.000000000000000000, 1.000000000000000000, 1.000000000000000000, 1.000000000000000000, 1.000000000000000000, 1.000000000000000000, 1.000000000000000000, 1.000000000000000000, 1.000000000000000000, 1.000000000000000000, 1.000000000000000000, 1.000000000000000000, 1.000000000000000000, 1.000000000000000000, 1.000000000000000000, 1.000000000000000000, 1.000000000000000000, 1.000000000000000000, 1.000000000000000000, 1.000000000000000000, 1.000000000000000000, 1.000000000000000000, 1.000000000000000000, 1.000000000000000000, 1.000000000000000000, 1.000000000000000000, 1.000000000000000000, 1.000000000000000000, 1.000000000000000000) ) ) 
 REPRESENTATION_ITEM ( '' )  SURFACE ( )  );
#11609 = PLANE ( 'NONE',  #24611 ) ;
#11610 = CARTESIAN_POINT ( 'NONE',  ( -208.1127848780265026, 1.189126717069624012E-13, -15.00245453012669472 ) ) ;
#11611 = CYLINDRICAL_SURFACE ( 'NONE', #3616, 29.99999999999999645 ) ;
#11612 = CARTESIAN_POINT ( 'NONE',  ( 14.38125909742181285, -15.17850393972633505, 0.000000000000000000 ) ) ;
#11613 = CARTESIAN_POINT ( 'NONE',  ( -135.8532207217289454, -30.84685318188648750, -40.00000000000002132 ) ) ;
#11614 = CARTESIAN_POINT ( 'NONE',  ( 130.8568914410475088, 24.07718906446891793, 32.49135343045489321 ) ) ;
#11615 = CARTESIAN_POINT ( 'NONE',  ( -238.4067589809705794, -40.96449427990185654, -40.00000000000002132 ) ) ;
#11616 = CARTESIAN_POINT ( 'NONE',  ( -114.5247514186166313, 19.74212785478623999, 9.597443935963386963 ) ) ;
#11617 = CARTESIAN_POINT ( 'NONE',  ( -135.8532207217289738, -1.208299557080134822E-13, 9.153146818113572891 ) ) ;
#11618 = CARTESIAN_POINT ( 'NONE',  ( -56.48582580120559271, 21.81201906317768291, 21.81201906317777173 ) ) ;
#11619 = CARTESIAN_POINT ( 'NONE',  ( -30.26275506840324070, 41.69427246844628598, 2.449293598294708485E-15 ) ) ;
#11620 = EDGE_LOOP ( 'NONE', ( #24956, #21462, #14422, #10034 ) ) ;
#11621 = CARTESIAN_POINT ( 'NONE',  ( 23.64688638900299722, -42.77321027809698961, 23.28414885118088762 ) ) ;
#11622 = AXIS2_PLACEMENT_3D ( 'NONE', #2514, #10629, #18741 ) ;
#11623 = CARTESIAN_POINT ( 'NONE',  ( -716.9846540392142060, 82.50000000000008527, 52.49999999999980105 ) ) ;
#11624 = CARTESIAN_POINT ( 'NONE',  ( -100.7734535825088500, 12.25131212657490209, -44.31723036834897300 ) ) ;
#11625 = CARTESIAN_POINT ( 'NONE',  ( 200.0000000000000000, -40.00000000000005684, 19.99999999999978328 ) ) ;
#11626 = CARTESIAN_POINT ( 'NONE',  ( 192.4448373802101173, 14.14213562370261279, 42.42640687122091236 ) ) ;
#11627 = CARTESIAN_POINT ( 'NONE',  ( 57.59792236341147031, -2.435789363418150000, -40.00000000000002132 ) ) ;
#11628 = CARTESIAN_POINT ( 'NONE',  ( -210.0000000000000284, 60.27431767988564104, -73.32453023895048716 ) ) ;
#11629 = CARTESIAN_POINT ( 'NONE',  ( 199.9999999999998863, 12.86276811643300810, 13.99220397845184749 ) ) ;
#11630 = CARTESIAN_POINT ( 'NONE',  ( -77.56349232229743507, 1.384135235510518758, -22.09269011744814648 ) ) ;
#11631 = CARTESIAN_POINT ( 'NONE',  ( 91.82158438592158234, 16.11829626348378142, 40.45024623143977749 ) ) ;
#11632 = CARTESIAN_POINT ( 'NONE',  ( 0.2972598230770048811, -10.13633138497415942, -66.70487387989865624 ) ) ;
#11633 = CARTESIAN_POINT ( 'NONE',  ( -105.3824009378448494, 20.34996249420144565, -6.674565453639575985 ) ) ;
#11634 = CARTESIAN_POINT ( 'NONE',  ( -82.23866184891308251, 13.36787606754487534, -15.15017645651541045 ) ) ;
#11635 = CARTESIAN_POINT ( 'NONE',  ( -192.9588430854690273, -10.23066800231931239, -66.79921049724377724 ) ) ;
#11637 = CARTESIAN_POINT ( 'NONE',  ( -192.9588430854690273, -18.05360324515400094, -38.51493924976961836 ) ) ;
#11636 = CARTESIAN_POINT ( 'NONE',  ( 170.2234770963711128, 17.36149277827028925, -39.20704971665377059 ) ) ;
#11638 = CARTESIAN_POINT ( 'NONE',  ( -238.4067589809705794, 0.6820004457912851592, -0.6820004457913123597 ) ) ;
#11639 = CARTESIAN_POINT ( 'NONE',  ( 163.1118516004056573, -27.26290988616869626, 0.000000000000000000 ) ) ;
#11640 = CARTESIAN_POINT ( 'NONE',  ( 136.1360204305621266, -24.77266263493116583, -24.77266263493127951 ) ) ;
#11642 = CARTESIAN_POINT ( 'NONE',  ( -86.96347745069643054, -40.00000000000009948, 18.24025645688337960 ) ) ;
#11641 = CARTESIAN_POINT ( 'NONE',  ( 136.1360204305621266, -24.77266263493151044, 24.77266263493093135 ) ) ;
#11643 = CARTESIAN_POINT ( 'NONE',  ( 146.6084372240433993, -3.800685668858652999, 3.800685668858636568 ) ) ;
#11644 = CARTESIAN_POINT ( 'NONE',  ( 136.1360204305621266, 24.77266263493104148, 24.77266263493145004 ) ) ;
#11645 = CARTESIAN_POINT ( 'NONE',  ( -135.8532207217289738, 30.84685318188643421, 40.00000000000002132 ) ) ;
#11647 = EDGE_CURVE ( 'NONE', #13223, #9531, #10585, .T. ) ;
#11646 = ORIENTED_EDGE ( 'NONE', *, *, #12245, .F. ) ;
#11648 = CARTESIAN_POINT ( 'NONE',  ( 4.995406935893287326, 67.35176059882533650, 10.78321810390163549 ) ) ;
#11649 = DIRECTION ( 'NONE',  ( 1.000000000000000000, 1.836970198721030181E-16, 0.000000000000000000 ) ) ;
#11650 = CARTESIAN_POINT ( 'NONE',  ( 60.14720761598680099, 15.75494750870317517, 31.22869220294058934 ) ) ;
#11651 = CARTESIAN_POINT ( 'NONE',  ( -100.7734535825088500, -22.67402823373193499, 40.00000000000002132 ) ) ;
#11652 = ORIENTED_EDGE ( 'NONE', *, *, #4789, .F. ) ;
#11653 = CARTESIAN_POINT ( 'NONE',  ( -195.1686598215339075, -48.78512304066069305, 14.09692385499214673 ) ) ;
#11654 = CARTESIAN_POINT ( 'NONE',  ( 200.0000000000001705, -18.10265802883496278, 5.810802590798905598 ) ) ;
#11655 = CARTESIAN_POINT ( 'NONE',  ( -0.1993645193002740457, -18.24262160098860264, 44.04158448240443846 ) ) ;
#11656 = EDGE_CURVE ( 'NONE', #1634, #15141, #21471, .T. ) ;
#11657 = EDGE_CURVE ( 'NONE', #15674, #8800, #3702, .T. ) ;
#11658 = CARTESIAN_POINT ( 'NONE',  ( 25.31597067608072393, 17.58652183054798357, -42.45761951827109471 ) ) ;
#11659 = CARTESIAN_POINT ( 'NONE',  ( 199.0064300168743898, 6.416848550863170964, -18.94043562797172697 ) ) ;
#11660 = UNCERTAINTY_MEASURE_WITH_UNIT (LENGTH_MEASURE( 1.000000000000000082E-05 ), #15541, 'distance_accuracy_value', 'NONE');
#11661 = CARTESIAN_POINT ( 'NONE',  ( -88.39148973765163930, -19.92926839984433229, -8.577159256668494436 ) ) ;
#11662 = CARTESIAN_POINT ( 'NONE',  ( -238.4067589809705794, 39.99999999999997158, 0.9644942799827220803 ) ) ;
#11663 = DIRECTION ( 'NONE',  ( 0.000000000000000000, -1.000000000000000000, 0.000000000000000000 ) ) ;
#11664 = CARTESIAN_POINT ( 'NONE',  ( 8.517493190815718762, 49.32792454093251422, -14.17913040910384126 ) ) ;
#11665 = CARTESIAN_POINT ( 'NONE',  ( -259.2033419157646676, -30.48217210827744950, 40.00000000000002132 ) ) ;
#11667 = CARTESIAN_POINT ( 'NONE',  ( 169.9999999999999716, 22.62041470344888339, -9.369682556672254137 ) ) ;
#11666 = CARTESIAN_POINT ( 'NONE',  ( -187.3037411061767727, 23.25513534570619356, -42.71163782366665629 ) ) ;
#11668 = CARTESIAN_POINT ( 'NONE',  ( 98.29820294267349823, -16.98253775143801292, -10.58389073156956961 ) ) ;
#11669 = CARTESIAN_POINT ( 'NONE',  ( -280.0000000000000568, 19.99999999999996092, -40.00000000000002132 ) ) ;
#11670 = CARTESIAN_POINT ( 'NONE',  ( -135.8532207217289738, -9.153146818113595984, 40.00000000000002132 ) ) ;
#11671 = CARTESIAN_POINT ( 'NONE',  ( 91.82158438592159655, -39.99999999999976552, -22.79471317813512599 ) ) ;
#11672 = CARTESIAN_POINT ( 'NONE',  ( 199.9999999999999432, -1.727494763561684666E-13, 20.00000000000010303 ) ) ;
#11673 = CARTESIAN_POINT ( 'NONE',  ( -198.0356074513804572, -10.87444709759714634, -10.87444709759729911 ) ) ;
#11674 = ORIENTED_EDGE ( 'NONE', *, *, #11905, .F. ) ;
#11675 = CARTESIAN_POINT ( 'NONE',  ( -370.0000000000001137, -4.857225732735059864E-14, 0.000000000000000000 ) ) ;
#11676 = CARTESIAN_POINT ( 'NONE',  ( 184.8905102610680444, 20.92133201514447194, 40.00000000000002132 ) ) ;
#11677 = CARTESIAN_POINT ( 'NONE',  ( 191.7962200090128988, -14.19927417784172974, 14.19927417784142243 ) ) ;
#11678 = CARTESIAN_POINT ( 'NONE',  ( -99.31364972218659659, -8.933506367414295823, 20.48028939130929160 ) ) ;
#11679 = APPLICATION_PROTOCOL_DEFINITION ( 'draft international standard', 'automotive_design', 1998, #23780 ) ;
#11680 = ORIENTED_EDGE ( 'NONE', *, *, #13374, .T. ) ;
#11681 = ORIENTED_EDGE ( 'NONE', *, *, #21128, .F. ) ;
#11682 = CARTESIAN_POINT ( 'NONE',  ( 98.29820294267528880, -14.14213562373450017, -14.14213562373441668 ) ) ;
#11683 = CARTESIAN_POINT ( 'NONE',  ( 20.91285618069844077, -43.54130497318310233, -23.84652503052226535 ) ) ;
#11684 = ORIENTED_EDGE ( 'NONE', *, *, #3297, .F. ) ;
#11685 = CARTESIAN_POINT ( 'NONE',  ( 19.06497207195980792, 54.19242893257844429, -40.00000000000002132 ) ) ;
#11686 = CARTESIAN_POINT ( 'NONE',  ( -105.4732637872244112, -19.68494377761390268, 8.153770687239109805 ) ) ;
#11687 = ORIENTED_EDGE ( 'NONE', *, *, #9770, .T. ) ;
#11688 = CARTESIAN_POINT ( 'NONE',  ( 199.0261122283987731, -17.00127104892409591, 10.56324628376440877 ) ) ;
#11689=STYLED_ITEM('',(#26409),#8606);
#11690 = CONICAL_SURFACE ( 'NONE', #17632, 60.00000000000000000, 0.7853981633974447263 ) ;
#11691 = CARTESIAN_POINT ( 'NONE',  ( -190.1935165880706222, 13.92226094463962127, 47.62328200654616950 ) ) ;
#11692 = CARTESIAN_POINT ( 'NONE',  ( -86.96347745069644475, 12.89780903124401057, 12.89780903124407629 ) ) ;
#11693 = DIRECTION ( 'NONE',  ( 0.000000000000000000, -1.000000000000000000, 0.000000000000000000 ) ) ;
#11694 = CARTESIAN_POINT ( 'NONE',  ( 91.82158438592158234, 7.693928927950222250E-14, -17.20528682183300262 ) ) ;
#11695 = CARTESIAN_POINT ( 'NONE',  ( -208.1127848780265026, 38.89260858015777700, -38.89260858015687461 ) ) ;
#11696 = CARTESIAN_POINT ( 'NONE',  ( -105.2054292635175585, -2.444554031225951202E-13, 21.49321519473985020 ) ) ;
#11697 = CIRCLE ( 'NONE', #6623, 5.000000000000004441 ) ;
#11698 = CIRCLE ( 'NONE', #21914, 29.99999999999999645 ) ;
#11699 = VECTOR ( 'NONE', #21699, 1000.000000000000000 ) ;
#11700 = LINE ( 'NONE', #15310, #1229 ) ;
#11701 = CARTESIAN_POINT ( 'NONE',  ( 136.1360204305621266, -3.419521671106983309E-13, 35.03383547441296741 ) ) ;
#11702 = DIRECTION ( 'NONE',  ( 0.000000000000000000, 0.000000000000000000, 1.000000000000000000 ) ) ;
#11703 = CARTESIAN_POINT ( 'NONE',  ( 91.82158438592159655, -40.00000000000017764, 17.20528682183258340 ) ) ;
#11704 = CARTESIAN_POINT ( 'NONE',  ( -110.1017491837281597, -13.37584907588316518, 15.18340520632177260 ) ) ;
#11705 = CARTESIAN_POINT ( 'NONE',  ( -86.96347745069645896, -12.89780903124382938, -43.67073346367985920 ) ) ;
#11706 = CARTESIAN_POINT ( 'NONE',  ( 146.6084372240433993, 34.62501878078308692, 0.000000000000000000 ) ) ;
#11707 = CARTESIAN_POINT ( 'NONE',  ( -162.0762913951020892, -57.76657433524000851, 1.198031840315820329 ) ) ;
#11708 = CARTESIAN_POINT ( 'NONE',  ( -200.0000000000000000, -52.49999999999972999, -82.49999999999998579 ) ) ;
#11709 = EDGE_CURVE ( 'NONE', #21418, #2760, #23598, .T. ) ;
#11710 = CARTESIAN_POINT ( 'NONE',  ( -3.486753633152337439, -47.18604396268657553, 13.85715877881439262 ) ) ;
#11711 = CARTESIAN_POINT ( 'NONE',  ( -162.0762913951021176, 40.00000000000001421, -1.694272876827905394 ) ) ;
#11712 = CARTESIAN_POINT ( 'NONE',  ( -105.3755690713226727, 5.661656051307470077E-14, -21.75974354311649961 ) ) ;
#11713 = CARTESIAN_POINT ( 'NONE',  ( 4.995406935893294431, -17.50105314357198694, 39.06748935135188816 ) ) ;
#11714 = AXIS2_PLACEMENT_3D ( 'NONE', #24564, #14439, #8050 ) ;
#11715 = CARTESIAN_POINT ( 'NONE',  ( 136.1360204305621266, 24.77266263493104148, 24.77266263493145004 ) ) ;
#11716 = CARTESIAN_POINT ( 'NONE',  ( -195.1685814578710279, -14.09692187701076982, -48.78510996053330473 ) ) ;
#11717 = CARTESIAN_POINT ( 'NONE',  ( -86.96347745069645896, -12.89780903124382938, -43.67073346367985920 ) ) ;
#11718 = VERTEX_POINT ( 'NONE', #7233 ) ;
#11719 = CARTESIAN_POINT ( 'NONE',  ( -280.0000000000000000, 14.14213562373108246, -14.14213562373078581 ) ) ;
#11720 = ADVANCED_FACE ( 'NONE', ( #23477 ), #11609, .T. ) ;
#11721 = CARTESIAN_POINT ( 'NONE',  ( -317.0000000000000568, -4.857225732735059864E-14, 0.000000000000000000 ) ) ;
#11722 = CARTESIAN_POINT ( 'NONE',  ( -200.0000000000000000, -52.49999999999970868, 82.49999999999998579 ) ) ;
#11723 = CARTESIAN_POINT ( 'NONE',  ( -77.90255099906767100, 8.064892378658102601, -20.29001641120677846 ) ) ;
#11724 = CARTESIAN_POINT ( 'NONE',  ( -105.3755690713226585, -43.67073346367964604, -12.89780903124457545 ) ) ;
#11725 = CARTESIAN_POINT ( 'NONE',  ( -295.0000000000000568, -4.857225732735059864E-14, 19.53474504356812602 ) ) ;
#11726 = VERTEX_POINT ( 'NONE', #17727 ) ;
#11727 = CARTESIAN_POINT ( 'NONE',  ( 170.2234770963711128, -2.259079968736224833E-13, 24.55285855007187124 ) ) ;
#11728 = ADVANCED_FACE ( 'NONE', ( #21603 ), #19464, .T. ) ;
#11729 = CARTESIAN_POINT ( 'NONE',  ( 199.0255884649229756, -18.48832673850237285, 7.640083164573010954 ) ) ;
#11730 = CARTESIAN_POINT ( 'NONE',  ( -3.675706741950853118, 17.91131112508025680, 43.24173023805306570 ) ) ;
#11731 = ORIENTED_EDGE ( 'NONE', *, *, #7828, .T. ) ;
#11732 = ORIENTED_EDGE ( 'NONE', *, *, #16051, .F. ) ;
#11733 = CARTESIAN_POINT ( 'NONE',  ( -213.1075012329537230, 13.71589010951907817, -40.00000000000002132 ) ) ;
#11734 = CARTESIAN_POINT ( 'NONE',  ( 91.82158438592158234, 12.16597498397773869, -12.16597498397759303 ) ) ;
#11735 = CARTESIAN_POINT ( 'NONE',  ( -105.3755690713226585, 39.99999999999993605, 18.24025645688366737 ) ) ;
#11736 = CARTESIAN_POINT ( 'NONE',  ( -114.5520593196445418, -19.58754258080286093, -9.956319649466946586 ) ) ;
#11737 = CARTESIAN_POINT ( 'NONE',  ( 57.59792236341147031, 26.56190807104720975, -26.56190807104655249 ) ) ;
#11738 = CARTESIAN_POINT ( 'NONE',  ( 23.37394308801978937, 23.33966569535129310, -42.85717664514559999 ) ) ;
#11739 = CARTESIAN_POINT ( 'NONE',  ( 200.0000000000000853, -18.58433719308212773, 4.010382776060092525 ) ) ;
#11740 = DIRECTION ( 'NONE',  ( 0.000000000000000000, 1.000000000000000000, 0.000000000000000000 ) ) ;
#11741 = CARTESIAN_POINT ( 'NONE',  ( 6.011245401487375517, -18.54985650213898651, -44.78331514753573828 ) ) ;
#11742 = CARTESIAN_POINT ( 'NONE',  ( -56.48582580120559982, 34.75652343174628101, -21.81201906317743067 ) ) ;
#11743 = CIRCLE ( 'NONE', #12611, 5.000000000000011546 ) ;
#11744 = EDGE_CURVE ( 'NONE', #10228, #1453, #9403, .T. ) ;
#11745 = CARTESIAN_POINT ( 'NONE',  ( -397.9898987322331436, -69.99999999999998579, 8.572527594031463526E-15 ) ) ;
#11746 = CARTESIAN_POINT ( 'NONE',  ( 4.995406935893310418, -67.35176059880237176, 10.78321810387813429 ) ) ;
#11747 = CARTESIAN_POINT ( 'NONE',  ( 57.59792236341148453, -40.00000000000003553, 2.435789363417741438 ) ) ;
#11748 = DIRECTION ( 'NONE',  ( 1.000000000000000000, -1.836970198721030181E-16, -0.000000000000000000 ) ) ;
#11749 = CARTESIAN_POINT ( 'NONE',  ( 200.0000000000000000, 63.70262460423112572, -57.69613583541415380 ) ) ;
#11750 = CARTESIAN_POINT ( 'NONE',  ( 130.8568914410475088, -5.949712681206671405, 40.00000000000002132 ) ) ;
#11751 = CARTESIAN_POINT ( 'NONE',  ( 170.2234770963711128, 17.36149277826973503, 39.20704971665401217 ) ) ;
#11752 = CARTESIAN_POINT ( 'NONE',  ( -105.3755690713226727, -18.24025645688354302, -2.449293598294708485E-15 ) ) ;
#11753 = CARTESIAN_POINT ( 'NONE',  ( -105.3175882261754310, 5.408274864382292435, 20.76660717853357951 ) ) ;
#11754 = DIRECTION ( 'NONE',  ( 0.000000000000000000, 0.000000000000000000, -1.000000000000000000 ) ) ;
#11755 = EDGE_CURVE ( 'NONE', #22554, #23676, #3371, .T. ) ;
#11756 = CARTESIAN_POINT ( 'NONE',  ( 136.1360204305621266, 3.511608612530704665, 3.511608612530695339 ) ) ;
#11757 = ADVANCED_FACE ( 'NONE', ( #20536 ), #5901, .F. ) ;
#11758 = CARTESIAN_POINT ( 'NONE',  ( 14.38125909742180752, 55.17850393971008316, -40.00000000000002132 ) ) ;
#11759 = ORIENTED_EDGE ( 'NONE', *, *, #14441, .T. ) ;
#11760 = DIRECTION ( 'NONE',  ( 0.000000000000000000, 1.000000000000000000, 0.000000000000000000 ) ) ;
#11761 = CARTESIAN_POINT ( 'NONE',  ( -200.0000000000000000, -44.88127304974053544, -30.70179486994611295 ) ) ;
#11762 = AXIS2_PLACEMENT_3D ( 'NONE', #20827, #4602, #8578 ) ;
#11763 = CARTESIAN_POINT ( 'NONE',  ( 163.1118516004056573, 9.006482792074356425, -47.56205970284957374 ) ) ;
#11764 = CARTESIAN_POINT ( 'NONE',  ( 170.2234770963711128, -2.511315425431857630E-14, 15.44714144992816074 ) ) ;
#11765 = DIRECTION ( 'NONE',  ( 1.000000000000000000, 1.836970198721030181E-16, -0.000000000000000000 ) ) ;
#11766 = CARTESIAN_POINT ( 'NONE',  ( 170.2234770963711128, -2.259079968736224833E-13, 24.55285855007187124 ) ) ;
#11767 = CIRCLE ( 'NONE', #10947, 29.99999999999999645 ) ;
#11768 = CARTESIAN_POINT ( 'NONE',  ( -86.96347745069644475, -21.75974354311651737, 0.000000000000000000 ) ) ;
#11769 = CARTESIAN_POINT ( 'NONE',  ( -87.13361725327072804, 5.903697393916396424E-14, -21.49321519333428299 ) ) ;
#11770 = CARTESIAN_POINT ( 'NONE',  ( 200.0000000000001421, 18.96284454896564142, 1.255519873078760229 ) ) ;
#11771 = CARTESIAN_POINT ( 'NONE',  ( 199.9999999999999432, -9.506243415956056708, -16.45614580735059107 ) ) ;
#11772 = CARTESIAN_POINT ( 'NONE',  ( 4.995406935893290878, 39.06748935135239265, -39.06748935135144762 ) ) ;
#11773 = CARTESIAN_POINT ( 'NONE',  ( 0.2972598230769923355, 18.14793986248751168, -38.42060263243650553 ) ) ;
#11774 = B_SPLINE_CURVE_WITH_KNOTS ( 'NONE', 3,
 ( #5115, #25598, #19456, #15212, #3493, #17457 ),
 .UNSPECIFIED., .F., .F.,
 ( 4, 2, 4 ),
 ( -5.998621905801447002E-08, 0.03937827992696037865, 0.07875661984013980488 ),
 .UNSPECIFIED. ) ;
#11775 = CARTESIAN_POINT ( 'NONE',  ( 151.7948205124836250, 23.49921654116361225, -23.49921654116333514 ) ) ;
#11776 = CARTESIAN_POINT ( 'NONE',  ( -77.72936527555063435, 19.09948130765502938, -10.88227939677040013 ) ) ;
#11777 = CARTESIAN_POINT ( 'NONE',  ( 146.6084372240433709, 24.48358557860356655, -32.08495691632035118 ) ) ;
#11779 = CARTESIAN_POINT ( 'NONE',  ( 0.2972598230770011618, 10.13633138497555919, -66.70487387989845729 ) ) ;
#11778 = CARTESIAN_POINT ( 'NONE',  ( -91.56559293963834989, 16.03295912088740849, -40.53558337403661938 ) ) ;
#11780 = CARTESIAN_POINT ( 'NONE',  ( 19.06497207195981858, 10.03556273973516078, -66.60410523465806421 ) ) ;
#11781 = CARTESIAN_POINT ( 'NONE',  ( 151.7948205124836250, -33.23291073765550863, 0.000000000000000000 ) ) ;
#11782 = CARTESIAN_POINT ( 'NONE',  ( 98.29820294269173075, 19.99999999998819433, -2.308575297063409524E-13 ) ) ;
#11784 = CARTESIAN_POINT ( 'NONE',  ( 192.4448373802100889, 1.051811698935164031E-13, -20.00000000003942091 ) ) ;
#11783 = CARTESIAN_POINT ( 'NONE',  ( 170.2234770963711128, -17.36149277827010096, 17.36149277826970660 ) ) ;
#11785 = CARTESIAN_POINT ( 'NONE',  ( 57.59792236341148453, 1.722363176414758668, 54.84617931850880268 ) ) ;
#11786 = CARTESIAN_POINT ( 'NONE',  ( 19.06497207195980792, 10.03556273973447155, -10.03556273973422286 ) ) ;
#11787 = CARTESIAN_POINT ( 'NONE',  ( 91.82158438592158234, -17.20528682183298486, 40.00000000000002132 ) ) ;
#11788 = ORIENTED_EDGE ( 'NONE', *, *, #4630, .T. ) ;
#11789 = CARTESIAN_POINT ( 'NONE',  ( 146.6084372240433709, 3.800685668858776900, -52.76785682606518435 ) ) ;
#11790 = CARTESIAN_POINT ( 'NONE',  ( 190.0000000000000284, -82.49999999999990052, 52.49999999999977973 ) ) ;
#11791 = CARTESIAN_POINT ( 'NONE',  ( -188.2995950289364373, 13.82811170417132196, 46.99046209955516673 ) ) ;
#11792 = ADVANCED_BREP_SHAPE_REPRESENTATION ( '', ( #17642, #21058 ), #3629 ) ;
#11793 = CARTESIAN_POINT ( 'NONE',  ( -91.56559293963834989, -22.67402823373193499, 0.000000000000000000 ) ) ;
#11794 = ORIENTED_EDGE ( 'NONE', *, *, #21128, .T. ) ;
#11795 = CARTESIAN_POINT ( 'NONE',  ( -188.4265004370326722, -47.03620155434649064, 13.83489460444966923 ) ) ;
#11796 = DIRECTION ( 'NONE',  ( 0.000000000000000000, 1.000000000000000000, 0.000000000000000000 ) ) ;
#11797 = CARTESIAN_POINT ( 'NONE',  ( 8.556015491674958895, -24.84887822174851024, 44.89939803569725285 ) ) ;
#11798 = CARTESIAN_POINT ( 'NONE',  ( 23.48902902575126106, 23.31625887490740823, -42.82177761400715355 ) ) ;
#11799 = CARTESIAN_POINT ( 'NONE',  ( 199.0069392139017168, 4.538005534962026744, -19.47646040276416457 ) ) ;
#11800 = LINE ( 'NONE', #1704, #8330 ) ;
#11801 = CARTESIAN_POINT ( 'NONE',  ( 151.7948205124836250, 1.439163438361279259E-13, -33.23291073765553705 ) ) ;
#11802 = CARTESIAN_POINT ( 'NONE',  ( -135.8532207217289738, -6.472252184283586729, -50.09629031063973770 ) ) ;
#11803 = CARTESIAN_POINT ( 'NONE',  ( 19.06497207195980792, -14.19242893257839988, 40.00000000000002132 ) ) ;
#11805 = CARTESIAN_POINT ( 'NONE',  ( -602.7677399305880499, 35.86505692559326519, -17.73308590989056555 ) ) ;
#11804 = CARTESIAN_POINT ( 'NONE',  ( -121.8425463771063164, 9.420908039661981093, -22.74408395512567793 ) ) ;
#11806 = CARTESIAN_POINT ( 'NONE',  ( 0.2972598230769983307, -14.33493731733933352, 0.000000000000000000 ) ) ;
#11807 = CARTESIAN_POINT ( 'NONE',  ( -213.1075012329537230, -13.71589010951915810, -40.00000000000002132 ) ) ;
#11808 = CARTESIAN_POINT ( 'NONE',  ( -198.0356074513804572, 15.37879056873067007, 0.000000000000000000 ) ) ;
#11809 = CARTESIAN_POINT ( 'NONE',  ( 151.7948205124836534, -39.99999999999992184, -6.767089262349454515 ) ) ;
#11810 = CARTESIAN_POINT ( 'NONE',  ( -208.1127848780265026, 1.189126717069624012E-13, -15.00245453012669472 ) ) ;
#11811 = CARTESIAN_POINT ( 'NONE',  ( 163.1118516004056573, 19.27778845538753316, 19.27778845538783870 ) ) ;
#11812 = VERTEX_POINT ( 'NONE', #8019 ) ;
#11813 = CARTESIAN_POINT ( 'NONE',  ( -53.37769371738608726, 27.95780717557945039, -13.65853730965343260 ) ) ;
#11814 = CARTESIAN_POINT ( 'NONE',  ( -198.0356074513804572, 10.87444709759714989, 10.87444709759722450 ) ) ;
#11815 = EDGE_CURVE ( 'NONE', #13176, #4726, #7916, .T. ) ;
#11816 = CARTESIAN_POINT ( 'NONE',  ( -100.0957100001397748, -8.517115559226354549, 20.56213589532580954 ) ) ;
#11817 = ITEM_DEFINED_TRANSFORMATION ( 'NONE', 'NONE', #18044,  #21058 ) ;
#11818 = ORIENTED_EDGE ( 'NONE', *, *, #14339, .F. ) ;
#11819 = ORIENTED_EDGE ( 'NONE', *, *, #10146, .F. ) ;
#11820 = CARTESIAN_POINT ( 'NONE',  ( 14.38125909742181818, -39.01709431150904095, -17.55144818341490165 ) ) ;
#11821 = CARTESIAN_POINT ( 'NONE',  ( 27.26078259668992843, -41.90087417143951853, -17.35591035705024510 ) ) ;
#11822 = VERTEX_POINT ( 'NONE', #24667 ) ;
#11823 = CARTESIAN_POINT ( 'NONE',  ( -213.1075012329537230, 13.71589010951907817, -40.00000000000002132 ) ) ;
#11824 = CARTESIAN_POINT ( 'NONE',  ( -102.4309680866104202, -20.43798635336410285, 8.087567261735790325 ) ) ;
#11825 = AXIS2_PLACEMENT_3D ( 'NONE', #4435, #2432, #20399 ) ;
#11826 = ORIENTED_EDGE ( 'NONE', *, *, #12006, .F. ) ;
#11827 = CARTESIAN_POINT ( 'NONE',  ( 199.9999999999998863, 18.74710533595338546, 3.118879735276928855 ) ) ;
#11828 = CARTESIAN_POINT ( 'NONE',  ( 170.0000000000133014, 17.64300463311800016, 17.64300463311827016 ) ) ;
#11829 = CARTESIAN_POINT ( 'NONE',  ( 192.4448373802100889, 14.14213562370310662, 14.14213562370312438 ) ) ;
#11830 = CARTESIAN_POINT ( 'NONE',  ( -188.2652746676668869, -46.97858116095166281, -13.82569223135941883 ) ) ;
#11831 = CARTESIAN_POINT ( 'NONE',  ( 184.8905102610680444, 1.070102760522089011E-13, -20.92133201514444352 ) ) ;
#11832 = CARTESIAN_POINT ( 'NONE',  ( 192.4448373802101173, -20.00000000003938538, 40.00000000000002132 ) ) ;
#11833 = CARTESIAN_POINT ( 'NONE',  ( -259.2033419157646676, -6.730120644402966867, -49.83842185052038332 ) ) ;
#11834 = FACE_OUTER_BOUND ( 'NONE', #23213, .T. ) ;
#11835 = CARTESIAN_POINT ( 'NONE',  ( -86.96347745069644475, 5.999880687339585546E-14, -21.75974354311649961 ) ) ;
#11836 = CARTESIAN_POINT ( 'NONE',  ( -105.3755690713226585, -40.00000000000027711, 21.75974354311608749 ) ) ;
#11837 = CARTESIAN_POINT ( 'NONE',  ( 170.0000000000000000, -3.062538285712981700, -24.95097643317001612 ) ) ;
#11838 = CARTESIAN_POINT ( 'NONE',  ( -30.26275506840322649, -29.48230279907810925, 29.48230279907778950 ) ) ;
#11839 = CARTESIAN_POINT ( 'NONE',  ( 136.1360204305621266, 35.03383547441298163, -40.00000000000002132 ) ) ;
#11840 = CARTESIAN_POINT ( 'NONE',  ( -86.96347745069643054, -41.18208027870589660, -15.38646221621809040 ) ) ;
#11841 = CARTESIAN_POINT ( 'NONE',  ( 200.0000000000000000, -40.00000000000000711, 4.898587196589418548E-15 ) ) ;
#11842 = AXIS2_PLACEMENT_3D ( 'NONE', #22695, #8583, #16694 ) ;
#11843 =( BOUNDED_CURVE ( )  B_SPLINE_CURVE ( 3, ( #5356, #13463, #21583, #20512 ),
 .UNSPECIFIED., .F., .F. ) 
 B_SPLINE_CURVE_WITH_KNOTS ( ( 4, 4 ),
 ( 0.004183487405659313055, 0.01388163287021778290 ),
 .UNSPECIFIED. ) 
 CURVE ( )  GEOMETRIC_REPRESENTATION_ITEM ( )  RATIONAL_B_SPLINE_CURVE ( ( 0.6809743333591573577, 0.7608653435686164590, 0.8672072324488973027, 1.000000000000000000 ) ) 
 REPRESENTATION_ITEM ( '' )  );
#11844 = CARTESIAN_POINT ( 'NONE',  ( 5.009865950673486168, -49.09576456953146817, 14.14399394884959804 ) ) ;
#11845 = CARTESIAN_POINT ( 'NONE',  ( 136.1360204305621266, 24.77266263493104148, 24.77266263493145004 ) ) ;
#11846 = CARTESIAN_POINT ( 'NONE',  ( -30.26275506840324070, -40.00000000000003553, 1.694272468446120117 ) ) ;
#11847 = CARTESIAN_POINT ( 'NONE',  ( 151.7948205124836534, 33.06932595376365924, -23.49921654116018743 ) ) ;
#11848 = CARTESIAN_POINT ( 'NONE',  ( -114.6854600082618276, 12.16985185534088920, 18.38493165714585231 ) ) ;
#11849 = CARTESIAN_POINT ( 'NONE',  ( -189.1288815661498006, -13.87115472123443283, -47.28031329127929183 ) ) ;
#11850 = CARTESIAN_POINT ( 'NONE',  ( -200.0000000000000000, 66.50000000000009948, 66.50000000000005684 ) ) ;
#11851 = EDGE_LOOP ( 'NONE', ( #13099, #5813 ) ) ;
#11852 = CIRCLE ( 'NONE', #398, 5.000000000000039080 ) ;
#11853 = CARTESIAN_POINT ( 'NONE',  ( 91.82158438592158234, -40.45024623143936537, -16.11829626348475131 ) ) ;
#11854 = CARTESIAN_POINT ( 'NONE',  ( 184.8905102610680444, 14.79361573936396113, -14.79361573936377461 ) ) ;
#11855 = CARTESIAN_POINT ( 'NONE',  ( -259.2033419157646676, 9.517827891722582478, -40.00000000000002132 ) ) ;
#11856 = DIRECTION ( 'NONE',  ( -1.000000000000000000, 0.000000000000000000, 0.000000000000000000 ) ) ;
#11857 = CARTESIAN_POINT ( 'NONE',  ( 184.8905102610680444, -43.07788698682556827, -13.49065550809859104 ) ) ;
#11858 = CARTESIAN_POINT ( 'NONE',  ( -87.13361725327072804, 21.49321519333427233, -1.448021113139547951E-30 ) ) ;
#11859 = ORIENTED_EDGE ( 'NONE', *, *, #7759, .F. ) ;
#11860 = CARTESIAN_POINT ( 'NONE',  ( 199.9999999999999432, 11.06651829421018896, 15.46448801036256349 ) ) ;
#11861 = CARTESIAN_POINT ( 'NONE',  ( 35.93702930655396699, -12.87541766444613778, -42.26928858172315273 ) ) ;
#11862 = CARTESIAN_POINT ( 'NONE',  ( -3.449394506063832466, 17.93655106166724522, 43.30266483527507404 ) ) ;
#11863 = ORIENTED_EDGE ( 'NONE', *, *, #737, .F. ) ;
#11864 = ORIENTED_EDGE ( 'NONE', *, *, #2341, .F. ) ;
#11865 = CARTESIAN_POINT ( 'NONE',  ( -56.48582580120559271, -9.153146818113595984, 0.000000000000000000 ) ) ;
#11866 = CARTESIAN_POINT ( 'NONE',  ( 199.0069392139017168, 4.538005534962026744, -19.47646040276416457 ) ) ;
#11867 = CARTESIAN_POINT ( 'NONE',  ( -77.90255099906769942, -8.644468104261466834, -20.04994828523962980 ) ) ;
#11868 = CARTESIAN_POINT ( 'NONE',  ( -94.58360650941212100, -20.91945674511385533, -8.190527749482289011 ) ) ;
#11869 = DIRECTION ( 'NONE',  ( 1.000000000000000000, 1.836970198721030181E-16, 0.000000000000000000 ) ) ;
#11870 = AXIS2_PLACEMENT_3D ( 'NONE', #4780, #8888, #25134 ) ;
#11871 = CARTESIAN_POINT ( 'NONE',  ( -30.26275506840324070, 1.218738420030236455E-14, -1.694272468446259783 ) ) ;
#11872 = DIRECTION ( 'NONE',  ( 1.000000000000000000, 1.836970198721030427E-16, -0.000000000000000000 ) ) ;
#11873 = CARTESIAN_POINT ( 'NONE',  ( -351.0000000000000568, -4.857225732735059864E-14, 0.000000000000000000 ) ) ;
#11874 = DIRECTION ( 'NONE',  ( -1.000000000000000000, -0.000000000000000000, -0.000000000000000000 ) ) ;
#11875 = CARTESIAN_POINT ( 'NONE',  ( 199.0202951899208017, 7.027923415129357032, 18.72965638665138144 ) ) ;
#11876 = CARTESIAN_POINT ( 'NONE',  ( -114.4364955367310586, 8.064892380842531239, 20.29001642038765141 ) ) ;
#11877 = CARTESIAN_POINT ( 'NONE',  ( -3.449394506061945531, -17.93655106166727720, -43.30266483527577037 ) ) ;
#11878 = CARTESIAN_POINT ( 'NONE',  ( -162.0762913951020607, -57.76657433537922515, -1.198031840455874963 ) ) ;
#11879 = CARTESIAN_POINT ( 'NONE',  ( 146.6084372240433993, -24.48358557860353457, 24.48358557860296258 ) ) ;
#11880 = CARTESIAN_POINT ( 'NONE',  ( -91.56559293963834989, -12.25131212657492874, 12.25131212657477953 ) ) ;
#11881 = CARTESIAN_POINT ( 'NONE',  ( -56.48582580120558561, -40.00000000000012790, 9.153146818113166105 ) ) ;
#11882 = FACE_OUTER_BOUND ( 'NONE', #9305, .T. ) ;
#11883 = CARTESIAN_POINT ( 'NONE',  ( 199.9999999999999432, 14.14213562373093680, 14.14213562373114641 ) ) ;
#11884 = CARTESIAN_POINT ( 'NONE',  ( -30.26275506840322649, -41.69427246844630019, -2.449293598294708485E-15 ) ) ;
#11885 = CARTESIAN_POINT ( 'NONE',  ( 189.9999999999999716, 82.50000000000008527, 52.49999999999977973 ) ) ;
#11886 = CARTESIAN_POINT ( 'NONE',  ( 57.59792236341148453, -37.56421063658185489, -2.449293598294708485E-15 ) ) ;
#11887 = CARTESIAN_POINT ( 'NONE',  ( -114.7852463542949124, 14.79002490267117054, 16.52851182054974188 ) ) ;
#11888 = VECTOR ( 'NONE', #15189, 1000.000000000000000 ) ;
#11889 = CARTESIAN_POINT ( 'NONE',  ( -114.7284988330193443, 21.83722598071101828, -3.361565411871531683 ) ) ;
#11890 = CARTESIAN_POINT ( 'NONE',  ( -208.1127848780265026, 10.60833733269537049, 10.60833733269544510 ) ) ;
#11891 = CARTESIAN_POINT ( 'NONE',  ( -259.2033419157646676, -9.517827891722680178, -40.00000000000002132 ) ) ;
#11892 = VERTEX_POINT ( 'NONE', #14144 ) ;
#11893 = CIRCLE ( 'NONE', #21255, 30.00000000000000355 ) ;
#11894 = CARTESIAN_POINT ( 'NONE',  ( 37.15749683985864493, -38.58455518503008363, 20.52531616262464098 ) ) ;
#11895 = CARTESIAN_POINT ( 'NONE',  ( 98.29820294272414571, 7.653668647302724892, 18.47759065022804137 ) ) ;
#11896 = EDGE_CURVE ( 'NONE', #20612, #23081, #15872, .T. ) ;
#11897 = CARTESIAN_POINT ( 'NONE',  ( 14.38125909742180397, 67.30136555895953165, 10.73282306403583242 ) ) ;
#11898 = CARTESIAN_POINT ( 'NONE',  ( 136.1360204305621551, -40.00000000000001421, 4.966164525586921563 ) ) ;
#11899 = CARTESIAN_POINT ( 'NONE',  ( 184.8905102610680444, -14.79361573936399665, 14.79361573936367158 ) ) ;
#11900 = EDGE_CURVE ( 'NONE', #19485, #3139, #14400, .T. ) ;
#11901 = CARTESIAN_POINT ( 'NONE',  ( -213.1075012329537230, 13.71589010951907817, 40.00000000000002132 ) ) ;
#11902 = CARTESIAN_POINT ( 'NONE',  ( 19.06497207195980792, 54.19242893257844429, -40.00000000000002132 ) ) ;
#11903 = DIRECTION ( 'NONE',  ( -1.000000000000000000, -0.000000000000000000, -0.000000000000000000 ) ) ;
#11904 = CARTESIAN_POINT ( 'NONE',  ( 199.9999999999996874, 18.36026428565764945, 4.938082948735277533 ) ) ;
#11905 = EDGE_CURVE ( 'NONE', #5362, #21371, #848, .T. ) ;
#11906 = EDGE_CURVE ( 'NONE', #23636, #22079, #21327, .T. ) ;
#11907 = CARTESIAN_POINT ( 'NONE',  ( 199.9999999999999147, -18.99732930369138728, -0.7780015511921255511 ) ) ;
#11908 = CARTESIAN_POINT ( 'NONE',  ( -238.4067589809705794, 57.25054294065799354, -0.6820004457334954973 ) ) ;
#11909 = CARTESIAN_POINT ( 'NONE',  ( -238.4067589809705794, -28.96627169325352469, 27.60227080167035041 ) ) ;
#11910 = AXIS2_PLACEMENT_3D ( 'NONE', #23918, #16066, #1850 ) ;
#11911 = CARTESIAN_POINT ( 'NONE',  ( 184.8905102610680444, 14.79361573936396113, -14.79361573936377461 ) ) ;
#11912 = CARTESIAN_POINT ( 'NONE',  ( -82.24297220888476545, 15.98176361809532331, -12.40742895870143059 ) ) ;
#11913 = CARTESIAN_POINT ( 'NONE',  ( 130.8568914410475088, -4.207082182990058428, 52.36146031193416661 ) ) ;
#11915 = CYLINDRICAL_SURFACE ( 'NONE', #3654, 9.999999999999994671 ) ;
#11914 = CARTESIAN_POINT ( 'NONE',  ( 192.4448373802100889, -14.14213562370293431, -14.14213562370322030 ) ) ;
#11916 = CARTESIAN_POINT ( 'NONE',  ( 57.59792236341147031, -1.722363176414363206, -54.84617931850881689 ) ) ;
#11917 = CARTESIAN_POINT ( 'NONE',  ( -105.3755690713226727, 15.38646221621793231, -15.38646221621779020 ) ) ;
#11918 = CARTESIAN_POINT ( 'NONE',  ( 199.0227866802457584, 1.475801328052707806, 19.95124150608079105 ) ) ;
#11920 = CARTESIAN_POINT ( 'NONE',  ( -192.9588430854690273, -40.00000000000024158, 54.46834944101708231 ) ) ;
#11919 = CARTESIAN_POINT ( 'NONE',  ( -280.0000000000000568, 42.42640687119265408, 14.14213562373147504 ) ) ;
#11921 = CARTESIAN_POINT ( 'NONE',  ( -213.1075012329537230, -9.698598906450557777, 9.698598906450415669 ) ) ;
#11922 = CARTESIAN_POINT ( 'NONE',  ( -105.3755690713226585, -21.75974354311652448, 40.00000000000002132 ) ) ;
#11923 = ORIENTED_EDGE ( 'NONE', *, *, #190, .T. ) ;
#11924 = CARTESIAN_POINT ( 'NONE',  ( 19.06497207195980792, 10.03556273973433299, 10.03556273973436319 ) ) ;
#11925 = CARTESIAN_POINT ( 'NONE',  ( -4.119579890815007417, 42.21781124616257586, 17.48718999186797873 ) ) ;
#11926 = CARTESIAN_POINT ( 'NONE',  ( 67.79414719530582545, 10.30785037361446044, 30.31905270965464538 ) ) ;
#11927 = CARTESIAN_POINT ( 'NONE',  ( -135.8532207217289738, -9.153146818113595984, 0.000000000000000000 ) ) ;
#11928 = ORIENTED_EDGE ( 'NONE', *, *, #17606, .F. ) ;
#11929 = CARTESIAN_POINT ( 'NONE',  ( -198.9234529670461598, -49.24835336344875714, 14.16707775654302459 ) ) ;
#11930 = CARTESIAN_POINT ( 'NONE',  ( 199.9999999999998579, -17.31468161508541570, -7.846489601088847188 ) ) ;
#11931 = CARTESIAN_POINT ( 'NONE',  ( 2.692156443725823411, -18.42752958146757436, 44.48799183655690825 ) ) ;
#11932 = CARTESIAN_POINT ( 'NONE',  ( 13.28449813596364848, 24.75673736218053023, -44.77439867187970179 ) ) ;
#11933 = CARTESIAN_POINT ( 'NONE',  ( 199.0176767632675023, -16.26464645690579758, -11.64139296301337190 ) ) ;
#11934 = AXIS2_PLACEMENT_3D ( 'NONE', #7500, #23869, #14025 ) ;
#11935 = CARTESIAN_POINT ( 'NONE',  ( 140.2235668266257278, -30.42137084504314615, 12.60094438999813704 ) ) ;
#11936 = CARTESIAN_POINT ( 'NONE',  ( 146.6084372240433993, 1.478241399363601114E-13, -34.62501878078305850 ) ) ;
#11937 = CARTESIAN_POINT ( 'NONE',  ( 192.4448373802101173, 42.42640687116487896, 14.14213562375934075 ) ) ;
#11938 = CARTESIAN_POINT ( 'NONE',  ( 91.82158438592159655, -22.79471317813468900, 40.00000000000002132 ) ) ;
#11939 = CIRCLE ( 'NONE', #493, 60.00000000000011369 ) ;
#11941 = CARTESIAN_POINT ( 'NONE',  ( -259.2033419157646676, -6.730120644403663199, 6.730120644403451813 ) ) ;
#11940 = CARTESIAN_POINT ( 'NONE',  ( -188.3392995398626510, 13.83024151208869235, -47.00482667599663955 ) ) ;
#11942 = CARTESIAN_POINT ( 'NONE',  ( 98.29820294267410929, -15.89413956777455539, -12.20973600806684622 ) ) ;
#11943 = CARTESIAN_POINT ( 'NONE',  ( -91.56559293963836410, 22.67402823373190301, -40.00000000000002132 ) ) ;
#11944 = AXIS2_PLACEMENT_3D ( 'NONE', #17185, #24797, #6549 ) ;
#11945 = CARTESIAN_POINT ( 'NONE',  ( -208.1127848780264742, 15.00245453012665742, 40.00000000000002132 ) ) ;
#11946 = CARTESIAN_POINT ( 'NONE',  ( 91.82158438592158234, 2.580785920671402147E-13, -22.79471317813470321 ) ) ;
#11947 = CARTESIAN_POINT ( 'NONE',  ( 19.06497207195981147, 38.31983398719620482, 38.31983398719633271 ) ) ;
#11948 = CARTESIAN_POINT ( 'NONE',  ( 146.6084372240433993, -3.357462877844280890E-13, 34.62501878078305850 ) ) ;
#11949 = CARTESIAN_POINT ( 'NONE',  ( 91.82158438592156813, 40.45024623143973486, -16.11829626348390931 ) ) ;
#11950 = ORIENTED_EDGE ( 'NONE', *, *, #18331, .F. ) ;
#11951 = LINE ( 'NONE', #9430, #15777 ) ;
#11952 = DIRECTION ( 'NONE',  ( 0.000000000000000000, -1.000000000000000000, 0.000000000000000000 ) ) ;
#11953 = CARTESIAN_POINT ( 'NONE',  ( -94.58360650944290171, -8.190527749669946900, 20.91945674502963826 ) ) ;
#11954 = APPLICATION_PROTOCOL_DEFINITION ( 'draft international standard', 'automotive_design', 1998, #7971 ) ;
#11955 = ORIENTED_EDGE ( 'NONE', *, *, #21670, .T. ) ;
#11956 = ORIENTED_EDGE ( 'NONE', *, *, #8591, .F. ) ;
#11957 = CARTESIAN_POINT ( 'NONE',  ( -192.9588430854690273, -66.79921049724377724, 10.23066800231950069 ) ) ;
#11958 = CARTESIAN_POINT ( 'NONE',  ( 27.79909650602947835, -41.49206490658383473, -22.43832426412121350 ) ) ;
#11959 = ORIENTED_EDGE ( 'NONE', *, *, #16442, .T. ) ;
#11960 = CARTESIAN_POINT ( 'NONE',  ( 136.1360204305621551, -35.03383547441293899, -40.00000000000002132 ) ) ;
#11961 = CARTESIAN_POINT ( 'NONE',  ( -4.039451493210490796, -23.44932283416679297, 43.00522595894000943 ) ) ;
#11962 = ORIENTED_EDGE ( 'NONE', *, *, #16617, .F. ) ;
#11963 = CARTESIAN_POINT ( 'NONE',  ( 200.0000000000001137, 4.308913765035643273, 18.51575813813059668 ) ) ;
#11964 = AXIS2_PLACEMENT_3D ( 'NONE', #128, #22089, #10366 ) ;
#11965 = LINE ( 'NONE', #16350, #22181 ) ;
#11966 = CARTESIAN_POINT ( 'NONE',  ( -105.3755690713226585, 12.89780903124410472, -43.67073346367977393 ) ) ;
#11967 = CARTESIAN_POINT ( 'NONE',  ( -151.4802930569763362, -31.86309827676129558, -16.17241674347988578 ) ) ;
#11968 = CARTESIAN_POINT ( 'NONE',  ( 4.995406935893297984, -40.00000000000007816, 15.24977328854818914 ) ) ;
#11969 = CARTESIAN_POINT ( 'NONE',  ( -100.7734535825088500, -22.67402823373193499, 40.00000000000002132 ) ) ;
#11970 = CARTESIAN_POINT ( 'NONE',  ( -100.7734535825088358, 12.25131212657497848, -12.25131212657469604 ) ) ;
#11971 = CARTESIAN_POINT ( 'NONE',  ( 199.0261966595921592, -11.26051109717869458, 16.53566845662597729 ) ) ;
#11972 = CARTESIAN_POINT ( 'NONE',  ( 163.1118516004056573, -39.99999999999990052, -27.26290988616886679 ) ) ;
#11973 = CARTESIAN_POINT ( 'NONE',  ( -56.48582580120558561, -40.00000000000012790, 9.153146818113166105 ) ) ;
#11974 = ADVANCED_FACE ( 'NONE', ( #6947 ), #17052, .F. ) ;
#11975 = CARTESIAN_POINT ( 'NONE',  ( -199.9999999999998863, -44.86878812508856385, -24.82633483071075986 ) ) ;
#11976 = CARTESIAN_POINT ( 'NONE',  ( 130.8568914410475088, -32.49135343045460900, -24.07718906446924478 ) ) ;
#11977 = CARTESIAN_POINT ( 'NONE',  ( -198.0356074513804572, -15.37879056873074290, -40.00000000000002132 ) ) ;
#11978 = CARTESIAN_POINT ( 'NONE',  ( 192.4448373802101173, -42.42640687116490028, -14.14213562375904942 ) ) ;
#11979 = LINE ( 'NONE', #21964, #23243 ) ;
#11980 = CARTESIAN_POINT ( 'NONE',  ( -716.9846540392142060, -52.49999999999991473, 82.49999999999998579 ) ) ;
#11981 = CARTESIAN_POINT ( 'NONE',  ( 170.0000000000133014, 17.64300463311800016, 17.64300463311827016 ) ) ;
#11982 = CARTESIAN_POINT ( 'NONE',  ( -213.1075012329537230, -8.703598725189323045E-14, 13.71589010951911902 ) ) ;
#11983 = CARTESIAN_POINT ( 'NONE',  ( -86.96347745069644475, 12.89780903124410472, -43.67073346367977393 ) ) ;
#11984 = CIRCLE ( 'NONE', #6877, 28.79780246617542616 ) ;
#11985 = FACE_BOUND ( 'NONE', #25425, .T. ) ;
#11986 = CARTESIAN_POINT ( 'NONE',  ( -188.4702232936901396, -23.48628015403117431, -43.05505437950768766 ) ) ;
#11987 = CARTESIAN_POINT ( 'NONE',  ( -726.9846540392142060, 0.000000000000000000, -39.99999999999991473 ) ) ;
#11988 = ORIENTED_EDGE ( 'NONE', *, *, #3013, .T. ) ;
#11989 = CARTESIAN_POINT ( 'NONE',  ( 200.0000000000000000, -14.14213562373046784, -42.42640687119298804 ) ) ;
#11990 = CARTESIAN_POINT ( 'NONE',  ( -77.92915424793434909, 20.15198149301296482, 8.347224043097730473 ) ) ;
#11991 = CARTESIAN_POINT ( 'NONE',  ( -162.0762913951020892, -1.198031840385783919, 1.198031840385741731 ) ) ;
#11992 = FACE_OUTER_BOUND ( 'NONE', #23429, .T. ) ;
#11993 = CARTESIAN_POINT ( 'NONE',  ( 85.88462074443611982, 10.32536233759628708, 22.72792765570313023 ) ) ;
#11994 = CARTESIAN_POINT ( 'NONE',  ( 151.7948205124836534, -51.78348778862529400, -4.785054706299085581 ) ) ;
#11995 = CARTESIAN_POINT ( 'NONE',  ( 85.88462074442188054, -22.72792765587123398, 10.32536233720564667 ) ) ;
#11996 = ORIENTED_EDGE ( 'NONE', *, *, #9622, .T. ) ;
#11997 = CARTESIAN_POINT ( 'NONE',  ( 199.9999999999999716, 16.45620519018019579, 9.525122676133902289 ) ) ;
#11998 = DIRECTION ( 'NONE',  ( -1.000000000000000000, 0.000000000000000000, 0.000000000000000000 ) ) ;
#11999 = EDGE_CURVE ( 'NONE', #19714, #2455, #7676, .T. ) ;
#12000 = CARTESIAN_POINT ( 'NONE',  ( -4.260882601032770722, 13.81249720866915709, 46.91379881627262449 ) ) ;
#12001 = ORIENTED_EDGE ( 'NONE', *, *, #20689, .F. ) ;
#12002 = ORIENTED_EDGE ( 'NONE', *, *, #17510, .T. ) ;
#12003 = CARTESIAN_POINT ( 'NONE',  ( 14.38125909742180752, 10.73282306404720465, 10.73282306404724018 ) ) ;
#12004 = CARTESIAN_POINT ( 'NONE',  ( 199.0073806320087613, 3.093635517344801578, -19.75563546371214230 ) ) ;
#12005 = CARTESIAN_POINT ( 'NONE',  ( -110.1017833366170748, 9.974944988646792322E-14, -20.19517362627950874 ) ) ;
#12006 = EDGE_CURVE ( 'NONE', #17304, #17170, #7661, .T. ) ;
#12007 = DIRECTION ( 'NONE',  ( -0.01051738777842040756, -0.3995761382618722712, -0.9166396752737944187 ) ) ;
#12008 = CARTESIAN_POINT ( 'NONE',  ( 22.27781863259630768, 43.19367102554032556, -23.58928354771935076 ) ) ;
#12009 = EDGE_CURVE ( 'NONE', #22947, #151, #475, .T. ) ;
#12010 = CARTESIAN_POINT ( 'NONE',  ( 35.93765736440253278, 20.78447772034747842, -38.99300256376233875 ) ) ;
#12011 = CARTESIAN_POINT ( 'NONE',  ( 199.9999999999999147, -17.05087848619496782, 8.411269650559694000 ) ) ;
#12012 = CARTESIAN_POINT ( 'NONE',  ( -650.6015225192315938, 35.46186828486367659, -18.52428024556027353 ) ) ;
#12013 = CARTESIAN_POINT ( 'NONE',  ( -53.37686176745753386, -13.65870576116508239, 27.95807077219537717 ) ) ;
#12014 = CARTESIAN_POINT ( 'NONE',  ( 199.0166590359707754, 13.17187519532568984, 15.05399639075651130 ) ) ;
#12015 = CARTESIAN_POINT ( 'NONE',  ( -163.7067538432321783, 35.82971521589534092, 14.84115397836969485 ) ) ;
#12016 = CARTESIAN_POINT ( 'NONE',  ( -4.558244102846352064, -13.79151199599447963, -46.81081390833299594 ) ) ;
#12017 = CARTESIAN_POINT ( 'NONE',  ( -30.26275506840322294, -57.76657404653985139, -1.198031551616531853 ) ) ;
#12018 = CARTESIAN_POINT ( 'NONE',  ( -105.3174728402264151, 5.408230752242470629, -20.76733781320130490 ) ) ;
#12019 = CARTESIAN_POINT ( 'NONE',  ( -100.7734535825088358, -12.25131212657493052, 12.25131212657478130 ) ) ;
#12020 = CARTESIAN_POINT ( 'NONE',  ( -238.4067589809705794, -40.00000000000005684, -0.9644942799830014124 ) ) ;
#12021 = DIRECTION ( 'NONE',  ( -1.303213150798907793E-16, 1.000000000000000000, -1.682156097916904081E-16 ) ) ;
#12022 = CARTESIAN_POINT ( 'NONE',  ( 184.8905102610680444, -19.07866798485554938, 40.00000000000002132 ) ) ;
#12023 = CARTESIAN_POINT ( 'NONE',  ( 136.1360204305621266, 24.77266263493138965, -24.77266263493110188 ) ) ;
#12024 = CARTESIAN_POINT ( 'NONE',  ( -91.56559293963834989, -17.32597176626812896, 40.00000000000002132 ) ) ;
#12025 = CARTESIAN_POINT ( 'NONE',  ( -110.0996815860078328, 15.29816958059242538, 13.19859759219660766 ) ) ;
#12026 = CARTESIAN_POINT ( 'NONE',  ( 57.59792236341147031, 40.00000000000042633, -37.56421063658144277 ) ) ;
#12027 = CARTESIAN_POINT ( 'NONE',  ( -192.9588430854690273, 38.51493924976939098, -18.05360324515436687 ) ) ;
#12028 = CARTESIAN_POINT ( 'NONE',  ( -105.3755690713226585, -21.75974354311652448, -40.00000000000002132 ) ) ;
#12029 = ORIENTED_EDGE ( 'NONE', *, *, #13374, .F. ) ;
#12030 = CARTESIAN_POINT ( 'NONE',  ( -259.2033419157646676, -9.517827891722680178, 40.00000000000002132 ) ) ;
#12031 = DIRECTION ( 'NONE',  ( -1.000000000000000000, 0.000000000000000000, 0.000000000000000000 ) ) ;
#12032 = CARTESIAN_POINT ( 'NONE',  ( -192.9588430854690273, 66.79921049721887982, 10.23066800229522677 ) ) ;
#12033 = CARTESIAN_POINT ( 'NONE',  ( -198.0356074513804572, -2.321818583541004323E-13, 55.37879056873073580 ) ) ;
#12034 = CARTESIAN_POINT ( 'NONE',  ( 163.1118516004056573, 9.006482792073693844, 47.56205970284970164 ) ) ;
#12035 = CARTESIAN_POINT ( 'NONE',  ( 184.8905102610680444, -1.851754852062639767E-13, 20.92133201514444352 ) ) ;
#12036 = CARTESIAN_POINT ( 'NONE',  ( -199.9999999999998863, -44.86878812508856385, -24.82633483071075986 ) ) ;
#12037 = CARTESIAN_POINT ( 'NONE',  ( -138.9613193423055861, -27.95779829447855747, -13.65853114841838334 ) ) ;
#12038 = CARTESIAN_POINT ( 'NONE',  ( 199.9999999999998295, 13.96930097052764097, 12.88701297307445159 ) ) ;
#12039 = CARTESIAN_POINT ( 'NONE',  ( 200.0000000000000284, -15.63578675875477941, -10.80997969227835043 ) ) ;
#12040 = CARTESIAN_POINT ( 'NONE',  ( 130.8568914410475372, 4.207082182992923691, -4.207082182992794017 ) ) ;
#12041 = CARTESIAN_POINT ( 'NONE',  ( -213.1075012329537230, -66.26714140136188291, -9.698598906438677503 ) ) ;
#12042 = CARTESIAN_POINT ( 'NONE',  ( -105.3382940165702166, 20.63437339945704352, 5.722104500121528048 ) ) ;
#12043 = CARTESIAN_POINT ( 'NONE',  ( -208.1127848780265026, 1.189126717069624012E-13, -15.00245453012669472 ) ) ;
#12044 = CARTESIAN_POINT ( 'NONE',  ( -56.48582580120558561, -50.09629031063971638, 6.472252184283745713 ) ) ;
#12045 = CARTESIAN_POINT ( 'NONE',  ( -200.0000000000000000, -61.50000000000001421, -66.50000000000005684 ) ) ;
#12046 = CARTESIAN_POINT ( 'NONE',  ( -259.2033419157646676, -6.730120644403663199, 6.730120644403451813 ) ) ;
#12047 = CARTESIAN_POINT ( 'NONE',  ( 136.1360204305621266, -3.511608612530379592, -53.05693388239318153 ) ) ;
#12048 = CARTESIAN_POINT ( 'NONE',  ( 199.0248586838703773, -4.674415065593815477, 19.46161178335769293 ) ) ;
#12049 = EDGE_CURVE ( 'NONE', #2955, #17072, #51, .T. ) ;
#12051 = CARTESIAN_POINT ( 'NONE',  ( 91.82158438592158234, 7.693928927950222250E-14, -17.20528682183300262 ) ) ;
#12050 = CARTESIAN_POINT ( 'NONE',  ( 0.2972598230769907257, 66.70487387989869887, -10.13633138497392494 ) ) ;
#12052 = CARTESIAN_POINT ( 'NONE',  ( -213.1075012329537230, -9.698598906450422774, -9.698598906450550672 ) ) ;
#12053 = CARTESIAN_POINT ( 'NONE',  ( 9.006212071497149196, 44.90541342374627476, -24.85331907610142821 ) ) ;
#12054 = CARTESIAN_POINT ( 'NONE',  ( -259.2033419157646676, 30.48217210827735713, -40.00000000000002132 ) ) ;
#12055 = ORIENTED_EDGE ( 'NONE', *, *, #23092, .T. ) ;
#12056 = CARTESIAN_POINT ( 'NONE',  ( 12.01676469546555559, -24.84032989753396237, -44.88780742856565809 ) ) ;
#12057 = EDGE_CURVE ( 'NONE', #16316, #7090, #25110, .T. ) ;
#12058 = CARTESIAN_POINT ( 'NONE',  ( 23.10131000537883850, 42.18277622344346867, 17.47267801029965284 ) ) ;
#12059 = CARTESIAN_POINT ( 'NONE',  ( -362.0709805440841365, -4.605747634845933236E-14, -20.53474504356812247 ) ) ;
#12060 =( REPRESENTATION_RELATIONSHIP ('NONE','NONE', #23888, #3691 ) REPRESENTATION_RELATIONSHIP_WITH_TRANSFORMATION ( #3576 )SHAPE_REPRESENTATION_RELATIONSHIP( ) );
#12061 = CARTESIAN_POINT ( 'NONE',  ( 146.6084372240433993, -34.62501878078303008, 0.000000000000000000 ) ) ;
#12062 = EDGE_CURVE ( 'NONE', #1963, #14258, #14664, .T. ) ;
#12063 = ORIENTED_EDGE ( 'NONE', *, *, #24937, .F. ) ;
#12064 = CARTESIAN_POINT ( 'NONE',  ( -188.6889827002227094, -47.12918603174894372, 13.84869468767960576 ) ) ;
#12065 = CARTESIAN_POINT ( 'NONE',  ( 199.9999999999996874, -18.99916535394237727, -0.6249076428296399532 ) ) ;
#12066 = CARTESIAN_POINT ( 'NONE',  ( 3.869409319520470625, -24.63759630011287172, 44.61273074174902575 ) ) ;
#12067 = CARTESIAN_POINT ( 'NONE',  ( 23.13330272892167727, 17.84165608060106223, -43.07356808498627032 ) ) ;
#12068 = CARTESIAN_POINT ( 'NONE',  ( 199.0134806391063194, -10.42534412885540185, -17.06722571675988931 ) ) ;
#12069 = FACE_BOUND ( 'NONE', #22519, .T. ) ;
#12070 = CARTESIAN_POINT ( 'NONE',  ( -187.3037411062135504, -13.75782484034011510, 46.64555264107092825 ) ) ;
#12071 = CARTESIAN_POINT ( 'NONE',  ( 91.82158438592158234, 44.40256751092319121, 12.16597498400105515 ) ) ;
#12072 = CARTESIAN_POINT ( 'NONE',  ( -238.4067589809705794, -0.9644942799826262680, 0.000000000000000000 ) ) ;
#12074 = CARTESIAN_POINT ( 'NONE',  ( 57.59792236341147031, -1.722363176415055985, 1.722363176415024677 ) ) ;
#12073 = CARTESIAN_POINT ( 'NONE',  ( -188.2507053402893860, 23.43979243030716830, -42.99082124348435485 ) ) ;
#12075 = DIRECTION ( 'NONE',  ( -1.000000000000000000, 0.000000000000000000, 0.000000000000000000 ) ) ;
#12076 = CARTESIAN_POINT ( 'NONE',  ( -86.96347745069645896, 21.75974354311648895, -40.00000000000002132 ) ) ;
#12077 = CARTESIAN_POINT ( 'NONE',  ( 184.8905102610680444, 19.07866798485562043, 2.449293598294708485E-15 ) ) ;
#12078 = CARTESIAN_POINT ( 'NONE',  ( -198.0356074513804572, 5.461327841961909642E-13, -55.37879056873073580 ) ) ;
#12079 = CARTESIAN_POINT ( 'NONE',  ( -105.3755690713226727, 12.89780903124400879, 12.89780903124407452 ) ) ;
#12080 = CARTESIAN_POINT ( 'NONE',  ( 200.0000000000000000, -40.00000000000019185, 19.99999999999968381 ) ) ;
#12081 = PRODUCT_DEFINITION_SHAPE ( 'NONE', 'NONE',  #26358 ) ;
#12082 = CARTESIAN_POINT ( 'NONE',  ( -91.56559293963836410, 44.31723036834908669, -12.25131212657445801 ) ) ;
#12083 = B_SPLINE_CURVE_WITH_KNOTS ( 'NONE', 3,
 ( #2095, #10600, #22455, #18712, #496, #8603 ),
 .UNSPECIFIED., .F., .F.,
 ( 4, 2, 4 ),
 ( -5.998616629415296830E-08, 0.005995031700373161000, 0.01199012338691261489 ),
 .UNSPECIFIED. ) ;
#12084 = ORIENTED_EDGE ( 'NONE', *, *, #9630, .F. ) ;
#12085 = CARTESIAN_POINT ( 'NONE',  ( 136.1360204305621266, -24.77266263493116583, -24.77266263493127951 ) ) ;
#12086 = DIRECTION ( 'NONE',  ( 0.000000000000000000, 0.000000000000000000, 1.000000000000000000 ) ) ;
#12087 = CONTEXT_DEPENDENT_SHAPE_REPRESENTATION ( #18870, #1903 ) ;
#12088 = ORIENTED_EDGE ( 'NONE', *, *, #12837, .T. ) ;
#12089 = EDGE_LOOP ( 'NONE', ( #16775, #8839, #14481, #11061, #23419, #25681, #7066, #22524 ) ) ;
#12090 = CARTESIAN_POINT ( 'NONE',  ( 192.4448373802101173, -42.42640687116490028, -14.14213562375904942 ) ) ;
#12091 = CARTESIAN_POINT ( 'NONE',  ( 23.25494099740648934, -43.03927110441365755, -17.82744980610230456 ) ) ;
#12092 = EDGE_CURVE ( 'NONE', #23789, #23087, #978, .T. ) ;
#12093 = ORIENTED_EDGE ( 'NONE', *, *, #13669, .F. ) ;
#12094 = CARTESIAN_POINT ( 'NONE',  ( 91.82158438592158234, 22.79471317813472453, -40.00000000000002132 ) ) ;
#12095 = ORIENTED_EDGE ( 'NONE', *, *, #25498, .T. ) ;
#12096 = CARTESIAN_POINT ( 'NONE',  ( 199.9999999999996589, 6.678198862535981384, 17.79829383751451388 ) ) ;
#12097 = FACE_OUTER_BOUND ( 'NONE', #10389, .T. ) ;
#12098 = CARTESIAN_POINT ( 'NONE',  ( 136.1360204305621551, 3.511608612530801032, -53.05693388239316022 ) ) ;
#12099 = CARTESIAN_POINT ( 'NONE',  ( -187.7699188114776234, -46.80708926512986778, -13.79076593537901552 ) ) ;
#12100 = CARTESIAN_POINT ( 'NONE',  ( 184.8905102610680444, -39.99999999999991473, -20.92133201514458207 ) ) ;
#12101 = CARTESIAN_POINT ( 'NONE',  ( -192.9588430854690273, 14.46834944099966336, 40.00000000000002132 ) ) ;
#12102 = CARTESIAN_POINT ( 'NONE',  ( 91.82158438592158234, -12.16597498399995203, -44.40256751092347542 ) ) ;
#12103 = CARTESIAN_POINT ( 'NONE',  ( 199.0219179450577371, 3.573952992290374109, 19.68174087806957573 ) ) ;
#12104 = CARTESIAN_POINT ( 'NONE',  ( 4.995406935893290878, -5.232665749138292703E-14, 15.24977328854832592 ) ) ;
#12105 = CARTESIAN_POINT ( 'NONE',  ( 4.995406935893298872, -1.944352046434030652E-13, 55.24977328854835434 ) ) ;
#12106 = CARTESIAN_POINT ( 'NONE',  ( 192.4448373802101173, -40.00000000000019185, 20.00000000003900524 ) ) ;
#12107 = CARTESIAN_POINT ( 'NONE',  ( -162.0762913951021176, 39.99999999999998579, 1.694272876828463614 ) ) ;
#12108 = CARTESIAN_POINT ( 'NONE',  ( -238.4067589809705794, -0.9644942799826262680, 0.000000000000000000 ) ) ;
#12109 = CARTESIAN_POINT ( 'NONE',  ( 163.1118516004056573, -37.29075403953139300, -19.27778845539249630 ) ) ;
#12110 = CARTESIAN_POINT ( 'NONE',  ( 19.06497207195980792, -14.19242893257839988, -40.00000000000002132 ) ) ;
#12111 = CARTESIAN_POINT ( 'NONE',  ( -135.8532207217289738, -50.09629031063965243, -6.472252184284438492 ) ) ;
#12112 = FACE_BOUND ( 'NONE', #7272, .T. ) ;
#12113 = B_SPLINE_CURVE_WITH_KNOTS ( 'NONE', 3,
 ( #22075, #26075, #5444, #13677, #13422, #11543 ),
 .UNSPECIFIED., .F., .F.,
 ( 4, 2, 4 ),
 ( 1.430489624538199204E-17, 0.03937634048170810669, 0.07875268096341619950 ),
 .UNSPECIFIED. ) ;
#12114 = FACE_OUTER_BOUND ( 'NONE', #7659, .T. ) ;
#12115 = CARTESIAN_POINT ( 'NONE',  ( -105.3755690713226727, -2.472783935621397949E-13, 21.75974354311649961 ) ) ;
#12116 = CARTESIAN_POINT ( 'NONE',  ( 151.7948205124836534, -40.00000000000001421, 6.767089262348889633 ) ) ;
#12117 = CARTESIAN_POINT ( 'NONE',  ( 146.6084372240433993, 3.800685668858676980, 3.800685668858667210 ) ) ;
#12118 = CARTESIAN_POINT ( 'NONE',  ( -114.6692722883742164, 11.86629262262099083, 18.56554616133607993 ) ) ;
#12119 = CARTESIAN_POINT ( 'NONE',  ( -188.2871287166142338, -13.82723289751134743, -46.98614659774170121 ) ) ;
#12120 = CARTESIAN_POINT ( 'NONE',  ( -280.0000000000000000, 14.14213562373098299, -14.14213562373088706 ) ) ;
#12121 = VERTEX_POINT ( 'NONE', #21200 ) ;
#12122 = CARTESIAN_POINT ( 'NONE',  ( 136.1360204305621551, -24.77266263493081766, -31.79587985999290112 ) ) ;
#12123 = DIRECTION ( 'NONE',  ( 0.000000000000000000, 0.000000000000000000, 1.000000000000000000 ) ) ;
#12124 = CARTESIAN_POINT ( 'NONE',  ( 199.9999999999999432, 20.00000000000013856, 0.000000000000000000 ) ) ;
#12125 = CARTESIAN_POINT ( 'NONE',  ( 136.1360204305621551, -24.77266263493081766, -31.79587985999290112 ) ) ;
#12126 = B_SPLINE_CURVE_WITH_KNOTS ( 'NONE', 3,
 ( #17852, #24257, #6158, #14267, #5893, #14137, #10152, #26002 ),
 .UNSPECIFIED., .F., .F.,
 ( 4, 2, 2, 4 ),
 ( -5.298247996675143094E-05, 0.001923793760056806803, 0.003900570000080365307, 0.007854122480127481015 ),
 .UNSPECIFIED. ) ;
#12127 = CARTESIAN_POINT ( 'NONE',  ( -82.26531528649849179, 5.040628272941656718, 19.58553546192279882 ) ) ;
#12128 =( GEOMETRIC_REPRESENTATION_CONTEXT ( 3 ) GLOBAL_UNCERTAINTY_ASSIGNED_CONTEXT ( ( #17779 ) ) GLOBAL_UNIT_ASSIGNED_CONTEXT ( ( #18682, #16685, #14424 ) ) REPRESENTATION_CONTEXT ( 'NONE', 'WORKASPACE' ) );
#12129 = ORIENTED_EDGE ( 'NONE', *, *, #25739, .T. ) ;
#12130 = AXIS2_PLACEMENT_3D ( 'NONE', #12539, #12679, #586 ) ;
#12131 = CARTESIAN_POINT ( 'NONE',  ( 199.9999999999999432, 13.20576333637327693, 13.67145050352531399 ) ) ;
#12132 = LINE ( 'NONE', #17974, #20022 ) ;
#12133 = CARTESIAN_POINT ( 'NONE',  ( -8.197988474478083987, 17.40147972966425627, 42.01088836873465482 ) ) ;
#12134 = ORIENTED_EDGE ( 'NONE', *, *, #21670, .F. ) ;
#12135 = VERTEX_POINT ( 'NONE', #21065 ) ;
#12136 = CARTESIAN_POINT ( 'NONE',  ( 19.06497207195980792, 14.19242893257840876, 0.000000000000000000 ) ) ;
#12137 = CARTESIAN_POINT ( 'NONE',  ( 199.0127284201194300, -9.139505923766694906, -17.79079187713806220 ) ) ;
#12138 = CARTESIAN_POINT ( 'NONE',  ( -110.0738147261103848, -5.034922404819302422, -19.58739231805851588 ) ) ;
#12139 = PRODUCT_DEFINITION_FORMATION_WITH_SPECIFIED_SOURCE ( 'ANY', '', #24865, .NOT_KNOWN. ) ;
#12140 = CARTESIAN_POINT ( 'NONE',  ( 12.01676469546554493, 44.88780742856572203, -24.84032989753405474 ) ) ;
#12141 = CARTESIAN_POINT ( 'NONE',  ( -56.48582580120560692, 39.99999999999991473, 9.153146818114004546 ) ) ;
#12142 = CARTESIAN_POINT ( 'NONE',  ( 199.9999999999999716, -17.31617203886849410, 7.850475485701642775 ) ) ;
#12143 = AXIS2_PLACEMENT_3D ( 'NONE', #437, #6027, #4177 ) ;
#12144 = CARTESIAN_POINT ( 'NONE',  ( -632.0909954410809632, 26.92861902581830691, -29.57939079808245353 ) ) ;
#12145 = CIRCLE ( 'NONE', #694, 74.99999999999995737 ) ;
#12146 = LINE ( 'NONE', #22406, #2604 ) ;
#12147 = CARTESIAN_POINT ( 'NONE',  ( 199.0235930299571123, -0.6679962965002699260, 20.00321896753086648 ) ) ;
#12148 = CYLINDRICAL_SURFACE ( 'NONE', #20273, 5.000000000000004441 ) ;
#12149 = CARTESIAN_POINT ( 'NONE',  ( 3.468680970034179634, -14.11592159092460719, -48.91035688726502428 ) ) ;
#12150 = CARTESIAN_POINT ( 'NONE',  ( 14.38125909742182529, -39.01709431150879936, -39.01709431150948859 ) ) ;
#12151 = CARTESIAN_POINT ( 'NONE',  ( -110.0738128639248288, 5.035098269363941448, -19.58735130876181785 ) ) ;
#12152 = CARTESIAN_POINT ( 'NONE',  ( 4.995406935893297984, -39.06748935135182421, -17.50105314357212549 ) ) ;
#12153 = CARTESIAN_POINT ( 'NONE',  ( -162.0762913951020892, -1.202636532414034422E-14, -1.694272876828323948 ) ) ;
#12154 = CARTESIAN_POINT ( 'NONE',  ( 4.995406935893293543, -10.78321810388990265, -10.78321810389009272 ) ) ;
#12155 = CARTESIAN_POINT ( 'NONE',  ( -280.0000000000000568, 19.99999999999996092, 40.00000000000002132 ) ) ;
#12156 = AXIS2_PLACEMENT_3D ( 'NONE', #2102, #10211, #14329 ) ;
#12157 = DIRECTION ( 'NONE',  ( 0.000000000000000000, 0.000000000000000000, 1.000000000000000000 ) ) ;
#12158 = CARTESIAN_POINT ( 'NONE',  ( 163.1118516004056573, -12.73709011382472234, -2.449293598294708485E-15 ) ) ;
#12159 = CARTESIAN_POINT ( 'NONE',  ( -114.6701221307682914, 11.88156715851604339, 18.55671387348713353 ) ) ;
#12160 = CARTESIAN_POINT ( 'NONE',  ( 200.0000000000000000, 40.00000000000026290, -19.99999999999950617 ) ) ;
#12161 = CARTESIAN_POINT ( 'NONE',  ( 170.2234770963711128, 39.20704971665398375, -17.36149277826984871 ) ) ;
#12162 = CARTESIAN_POINT ( 'NONE',  ( 136.1360204305621266, -35.03383547441293899, 0.000000000000000000 ) ) ;
#12163 = ORIENTED_EDGE ( 'NONE', *, *, #17902, .T. ) ;
#12165 = VERTEX_POINT ( 'NONE', #20807 ) ;
#12164 = EDGE_CURVE ( 'NONE', #525, #10974, #5706, .T. ) ;
#12166 = CARTESIAN_POINT ( 'NONE',  ( 184.8905102610680444, -20.92133201514440799, 40.00000000000002132 ) ) ;
#12167 = VECTOR ( 'NONE', #16128, 1000.000000000000000 ) ;
#12168 = DIRECTION ( 'NONE',  ( -1.000000000000000000, 0.000000000000000000, 0.000000000000000000 ) ) ;
#12169 = SHAPE_REPRESENTATION ( 'Discharge flange', ( #21058 ), #7428 ) ;
#12170 = CARTESIAN_POINT ( 'NONE',  ( 151.7948205124836534, -39.99999999999987921, -33.23291073765567916 ) ) ;
#12171 = CARTESIAN_POINT ( 'NONE',  ( 170.2234770963711128, 39.20704971665372796, 17.36149277827039583 ) ) ;
#12172 = CARTESIAN_POINT ( 'NONE',  ( 184.8905102610680444, -20.92133201514440799, 0.000000000000000000 ) ) ;
#12173 = PLANE ( 'NONE',  #5348 ) ;
#12174 = CARTESIAN_POINT ( 'NONE',  ( -87.02146317964809441, 5.408180612257909914, -20.76663852858110815 ) ) ;
#12175 = CARTESIAN_POINT ( 'NONE',  ( 200.0000000000002558, 14.28373528157942829, 12.54030857537068755 ) ) ;
#12176 = CARTESIAN_POINT ( 'NONE',  ( 199.9999999999998863, -13.00209652640642943, -13.87527625954625954 ) ) ;
#12177 = CARTESIAN_POINT ( 'NONE',  ( 199.9999999999999432, 14.14213562373110911, -14.14213562373072364 ) ) ;
#12178 = CARTESIAN_POINT ( 'NONE',  ( -198.0356074513804572, -39.15871834505931304, 17.40982414986437377 ) ) ;
#12179 = CARTESIAN_POINT ( 'NONE',  ( -105.3073921447119261, 20.83275309902035843, 5.041689060256491217 ) ) ;
#12180 = CARTESIAN_POINT ( 'NONE',  ( -82.29192131161018153, 18.26745044306171550, -8.580784324595091661 ) ) ;
#12181 = CARTESIAN_POINT ( 'NONE',  ( 199.9999999999999432, -14.14213562373073607, -14.14213562373102206 ) ) ;
#12182 = CARTESIAN_POINT ( 'NONE',  ( 136.1360204305621266, -24.77266263493151044, 24.77266263493093135 ) ) ;
#12183 = CARTESIAN_POINT ( 'NONE',  ( 14.38125909742180752, 10.73282306404720465, 10.73282306404724018 ) ) ;
#12184 = CARTESIAN_POINT ( 'NONE',  ( -86.96347745069645896, -12.89780903124382938, -43.67073346367985920 ) ) ;
#12185 = CARTESIAN_POINT ( 'NONE',  ( 199.0263771353515949, -14.14574067859894413, 14.14574067859863682 ) ) ;
#12187 = CARTESIAN_POINT ( 'NONE',  ( -213.1075012329537230, 39.99999999999979394, 53.71589010950180665 ) ) ;
#12186 = CARTESIAN_POINT ( 'NONE',  ( 163.1118516004056573, 9.006482792069759213, -9.006482792069505194 ) ) ;
#12188 = CARTESIAN_POINT ( 'NONE',  ( 151.7948205124836534, 4.785054706297857230, 51.78348778862544322 ) ) ;
#12189 = CARTESIAN_POINT ( 'NONE',  ( 22.89778847645106907, 43.13990468001224343, -17.86913359794376532 ) ) ;
#12190 = CARTESIAN_POINT ( 'NONE',  ( -238.4067589809705794, 0.9644942799825385604, -40.00000000000002132 ) ) ;
#12191 = ORIENTED_EDGE ( 'NONE', *, *, #6239, .F. ) ;
#12192 = CARTESIAN_POINT ( 'NONE',  ( 0.4289717129526320338, -24.25042218720239262, -44.08776571100859343 ) ) ;
#12193 = AXIS2_PLACEMENT_3D ( 'NONE', #2049, #24396, #40 ) ;
#12194 = CARTESIAN_POINT ( 'NONE',  ( -8.720657192108198785, -45.36528685022982899, 13.49580954686996925 ) ) ;
#12195 = CARTESIAN_POINT ( 'NONE',  ( -162.0762913951021176, 1.694272876828294194, 40.00000000000002132 ) ) ;
#12196 = ORIENTED_EDGE ( 'NONE', *, *, #3372, .F. ) ;
#12197 = CARTESIAN_POINT ( 'NONE',  ( 21.15138808362603839, 23.80076113581877806, -43.47948264999411805 ) ) ;
#12198 = CARTESIAN_POINT ( 'NONE',  ( 199.9999999999998295, -19.00894346483091724, 0.1575548292166454312 ) ) ;
#12199 = CARTESIAN_POINT ( 'NONE',  ( 4.155455573144507753, -18.49472242009463230, 44.65020969902027304 ) ) ;
#12200 = EDGE_CURVE ( 'NONE', #18548, #17450, #19195, .T. ) ;
#12201 = CARTESIAN_POINT ( 'NONE',  ( 20.38198589867913668, 18.12553405621813596, -43.75891014376608013 ) ) ;
#12202 = CARTESIAN_POINT ( 'NONE',  ( 199.0116000645839449, -7.055149577161559549, -18.71482085160166875 ) ) ;
#12203 = CARTESIAN_POINT ( 'NONE',  ( 19.06497207195981147, 1.521599808664285085E-13, -14.19242893257840521 ) ) ;
#12204 = CARTESIAN_POINT ( 'NONE',  ( 156.1979191798868385, -27.38417834433187892, 11.34289806466571982 ) ) ;
#12205 = CARTESIAN_POINT ( 'NONE',  ( 170.2234770963711128, 1.169953928977015745E-13, -24.55285855007187124 ) ) ;
#12206 = CARTESIAN_POINT ( 'NONE',  ( -135.8532207217289738, 50.09629031063956006, 6.472252184284782217 ) ) ;
#12207 = CARTESIAN_POINT ( 'NONE',  ( -105.2054292635175869, 15.19799821370233062, -15.19799821370219206 ) ) ;
#12209 = CARTESIAN_POINT ( 'NONE',  ( -100.7734535825088500, 12.25131212657428748, 44.31723036834913643 ) ) ;
#12208 = CARTESIAN_POINT ( 'NONE',  ( -188.2652746676487254, 23.44263257803753575, -42.99511404081827948 ) ) ;
#12210 = CARTESIAN_POINT ( 'NONE',  ( 136.1360204305621551, -4.966164525587036138, -40.00000000000002132 ) ) ;
#12211 = CARTESIAN_POINT ( 'NONE',  ( -86.96347745069644475, 18.24025645688350750, 40.00000000000002132 ) ) ;
#12212 = CARTESIAN_POINT ( 'NONE',  ( -135.8532207217289738, 3.005970985514575011E-13, -30.84685318188645553 ) ) ;
#12213 = CARTESIAN_POINT ( 'NONE',  ( -30.26275506840325136, 57.76657404653985139, 1.198031551616126178 ) ) ;
#12214 = CARTESIAN_POINT ( 'NONE',  ( -102.4309680865773373, 20.17061239842026765, -8.733065089982426699 ) ) ;
#12215 = CARTESIAN_POINT ( 'NONE',  ( 163.1118516004056573, -9.006482792069506971, -9.006482792069697041 ) ) ;
#12216 = VERTEX_POINT ( 'NONE', #10692 ) ;
#12217 = CARTESIAN_POINT ( 'NONE',  ( 199.9999999999999432, -14.14213562373096345, -14.14213562373104871 ) ) ;
#12218 = CARTESIAN_POINT ( 'NONE',  ( -102.4309680865808616, 8.087567261658067608, 20.43798635340267111 ) ) ;
#12219 = ITEM_DEFINED_TRANSFORMATION ( 'NONE', 'NONE', #7023,  #21058 ) ;
#12220 = ORIENTED_EDGE ( 'NONE', *, *, #11815, .F. ) ;
#12221 = VERTEX_POINT ( 'NONE', #8691 ) ;
#12222 = CARTESIAN_POINT ( 'NONE',  ( -100.7734535825088500, -12.25131212657462498, -44.31723036834905827 ) ) ;
#12223 = CARTESIAN_POINT ( 'NONE',  ( 23.36927571439211704, -42.85861222363623568, -23.34061495561072519 ) ) ;
#12224 = ORIENTED_EDGE ( 'NONE', *, *, #2653, .F. ) ;
#12225 = CARTESIAN_POINT ( 'NONE',  ( -56.48582580120559982, -9.153146818113595984, -40.00000000000002132 ) ) ;
#12226 = CARTESIAN_POINT ( 'NONE',  ( -83.21262154144231715, 13.72187187063211233, 33.12752917117668972 ) ) ;
#12227 = ORIENTED_EDGE ( 'NONE', *, *, #16108, .F. ) ;
#12228 = CARTESIAN_POINT ( 'NONE',  ( 199.9999999999998863, 12.86276811643300810, 13.99220397845184749 ) ) ;
#12229 = FACE_OUTER_BOUND ( 'NONE', #6958, .T. ) ;
#12230 = CARTESIAN_POINT ( 'NONE',  ( -198.0356074513804572, 39.15871834505912119, -17.40982414986464377 ) ) ;
#12231 = CARTESIAN_POINT ( 'NONE',  ( -188.3066136396865318, -43.00728998844432738, -23.45085387054221115 ) ) ;
#12232 = ADVANCED_FACE ( 'NONE', ( #24939 ), #15320, .T. ) ;
#12233 = CARTESIAN_POINT ( 'NONE',  ( -259.2033419157646676, -40.00000000000017764, 30.48217210827725054 ) ) ;
#12234 = CARTESIAN_POINT ( 'NONE',  ( -208.1127848780264742, 55.00245453014418473, 40.00000000000002132 ) ) ;
#12235 = CARTESIAN_POINT ( 'NONE',  ( 170.2234770963711128, 10.92277846919216522, -10.92277846919186501 ) ) ;
#12236 = CARTESIAN_POINT ( 'NONE',  ( 199.0260481038674811, -10.14773143618404383, 17.24088832081764622 ) ) ;
#12237 = ADVANCED_FACE ( 'NONE', ( #13453 ), #17825, .T. ) ;
#12238 = CARTESIAN_POINT ( 'NONE',  ( 130.8568914410475088, -39.99999999999988631, -34.05028731879802706 ) ) ;
#12239 = CARTESIAN_POINT ( 'NONE',  ( 163.1118516004056573, -39.99999999999990052, -27.26290988616886679 ) ) ;
#12240 = CARTESIAN_POINT ( 'NONE',  ( -100.7734535825088358, 6.065416334915073333E-14, -22.67402823373191723 ) ) ;
#12241 = CARTESIAN_POINT ( 'NONE',  ( -162.0762913951020892, -1.694272876828353702, 0.000000000000000000 ) ) ;
#12242 = CARTESIAN_POINT ( 'NONE',  ( -198.0356074513804572, -10.87444709760996986, 67.44298959253333692 ) ) ;
#12243 = ADVANCED_FACE ( 'NONE', ( #25703 ), #21572, .T. ) ;
#12244 = CARTESIAN_POINT ( 'NONE',  ( 192.4448373802101173, 20.00000000003945644, -40.00000000000002132 ) ) ;
#12245 = EDGE_CURVE ( 'NONE', #18072, #4824, #23569, .T. ) ;
#12246 = CARTESIAN_POINT ( 'NONE',  ( -86.96347745069644475, -12.89780903124413491, 12.89780903124398037 ) ) ;
#12247 = DIRECTION ( 'NONE',  ( 1.357111460130037815E-16, -0.7387770694782697101, 0.6739498806388349861 ) ) ;
#12248 = DIRECTION ( 'NONE',  ( -1.000000000000000000, 0.000000000000000000, 0.000000000000000000 ) ) ;
#12249 = CARTESIAN_POINT ( 'NONE',  ( 4.995406935893283773, 40.00000000000017764, -15.24977328854790848 ) ) ;
#12250 = CARTESIAN_POINT ( 'NONE',  ( -162.0762913951020892, -1.777970010055771463E-13, 41.69427287682835015 ) ) ;
#12251 = CARTESIAN_POINT ( 'NONE',  ( -135.8532207217289738, 50.09629031063965243, -6.472252184284084109 ) ) ;
#12252 = CARTESIAN_POINT ( 'NONE',  ( 19.06497207195981147, -10.03556273973425483, -10.03556273973443247 ) ) ;
#12253 = CARTESIAN_POINT ( 'NONE',  ( -188.2957210513887674, -23.44847782072339371, -43.00408675155699001 ) ) ;
#12254 = CARTESIAN_POINT ( 'NONE',  ( -208.1127848780265026, -10.60833733269551971, 10.60833733269537049 ) ) ;
#12255 = ORIENTED_EDGE ( 'NONE', *, *, #631, .F. ) ;
#12256 = CARTESIAN_POINT ( 'NONE',  ( -105.3755690713226585, -43.67073346367964604, -12.89780903124457545 ) ) ;
#12257 = DIRECTION ( 'NONE',  ( 1.000000000000000000, -0.000000000000000000, -0.000000000000000000 ) ) ;
#12258 = CARTESIAN_POINT ( 'NONE',  ( -238.4067589809705794, -0.9644942799826262680, 0.000000000000000000 ) ) ;
#12259 = CARTESIAN_POINT ( 'NONE',  ( 19.06497207195980792, -18.24870850772710540, -38.31983398719647482 ) ) ;
#12260 = CARTESIAN_POINT ( 'NONE',  ( -200.0000000000000000, 2.362121657692426575E-30, 0.000000000000000000 ) ) ;
#12261 = VERTEX_POINT ( 'NONE', #9209 ) ;
#12262 = ORIENTED_EDGE ( 'NONE', *, *, #12062, .F. ) ;
#12263 = CARTESIAN_POINT ( 'NONE',  ( 200.0000000000000000, 13.86690804110605590, 13.01115396687990433 ) ) ;
#12264 = CARTESIAN_POINT ( 'NONE',  ( 20.59039453120230334, -23.90179120638647703, 43.61606461192731388 ) ) ;
#12265 = CARTESIAN_POINT ( 'NONE',  ( 3.468680970031514210, 24.60338114559333889, 44.56630890487709706 ) ) ;
#12266 = ORIENTED_EDGE ( 'NONE', *, *, #13619, .F. ) ;
#12267 = VERTEX_POINT ( 'NONE', #17443 ) ;
#12268 = CARTESIAN_POINT ( 'NONE',  ( 163.1118516004056573, -27.26290988616869626, -40.00000000000002132 ) ) ;
#12269 = CARTESIAN_POINT ( 'NONE',  ( 199.0089689370622352, -1.315408825438062257, -19.96384840600867960 ) ) ;
#12270 = CARTESIAN_POINT ( 'NONE',  ( -105.4741150117381636, -7.943527260753955765, -19.77569912954965758 ) ) ;
#12271 = CARTESIAN_POINT ( 'NONE',  ( 0.2972598230769938343, 10.13633138497472252, 10.13633138497475628 ) ) ;
#12272 = CARTESIAN_POINT ( 'NONE',  ( 0.4289717129525671413, 44.08776571100865027, -24.25042218720249920 ) ) ;
#12273 = CARTESIAN_POINT ( 'NONE',  ( -280.0000000000000000, 1.605030083646939673E-13, -20.00000000000001421 ) ) ;
#12274 = CARTESIAN_POINT ( 'NONE',  ( 199.9999999999996874, -18.85616045826023779, 2.487226269395955480 ) ) ;
#12275 =( BOUNDED_SURFACE ( )  B_SPLINE_SURFACE ( 3, 3, ( 
 ( #19894, #22172, #3946, #5658, #12043, #20163, #9784, #18159, #26305, #17756, #24299, #6067, #10185, #4079, #19757, #20301, #2078, #75, #5529, #13635, #1546, #7638, #4741, #22438, #16834, #16695, #14829, #8446, #14566, #10450 ),
 ( #14304, #2211, #16565, #12437, #10320, #24425, #8717, #748, #18563, #24695, #24828, #6191, #6581, #2336, #18427, #6715, #18830, #6317, #204, #14700, #22961, #24968, #6450, #22832, #20833, #24562, #22696, #4609, #20964, #8852 ),
 ( #12705, #4215, #2608, #342, #8313, #12848, #610, #14437, #16436, #10721, #2745, #10849, #4471, #18968, #12305, #20432, #12570, #18695, #20703, #22566, #4345, #20565, #2469, #10579, #479, #8584, #1258, #3377, #14966, #21099 ),
 ( #9242, #11109, #1005, #17472, #2879, #17349, #10987, #13483, #25485, #15354, #19225, #19096, #17093, #8989, #16962, #7234, #877, #5004, #23599, #12976, #3251, #25225, #6978, #23354, #15092, #23101, #7359, #23226, #25614, #23478 ),
 ( #11355, #25357, #1138, #5250, #13354, #15470, #9108, #5378, #11476, #5131, #6849, #13109, #19471, #21476, #9362, #1390, #4872, #21230, #21604, #7112, #15223, #19604, #3003, #17218, #13236, #21359, #3128, #11231, #19349, #25100 ),
 ( #1519, #13875, #12020, #5504, #15728, #9759, #20276, #13605, #3640, #14011, #3778, #5903, #22008, #11881, #20001, #1918, #20140, #25869, #26010, #11747, #7746, #22278, #7487, #25735, #21734, #1650, #26282, #19865, #15858, #21864 ),
 ( #15598, #3510, #17859, #23853, #11610, #9491, #10023, #12153, #23987, #5766, #1787, #17596, #9891, #13738, #19732, #18133, #3921, #17729, #9625, #17994, #8021, #16137, #26140, #7884, #22140, #23723, #16005, #24131, #24267, #6041 ) ),
 .UNSPECIFIED., .T., .F., .F. ) 
 B_SPLINE_SURFACE_WITH_KNOTS ( ( 4, 3, 4 ),
 ( 4, 2, 2, 2, 2, 2, 2, 2, 2, 2, 2, 2, 2, 2, 4 ),
 ( 0.000000000000000000, 0.5000000000000000000, 1.000000000000000000 ),
 ( 0.000000000000000000, 0.1357259735107005372, 0.1651108541090157700, 0.1944957347073310028, 0.3598804999793158710, 0.3867117631979620773, 0.4135430264166082281, 0.5789277916885930964, 0.6062785021374117456, 0.6336292125862302838, 0.8508620842112317728, 0.8814014469398914198, 0.9119408096685510667, 0.9559704048342755334, 1.000000000000000000 ),
 .UNSPECIFIED. ) 
 GEOMETRIC_REPRESENTATION_ITEM ( )  RATIONAL_B_SPLINE_SURFACE ( (
 ( 1.000000000000000000, 1.000000000000000000, 1.000000000000000000, 1.000000000000000000, 1.000000000000000000, 1.000000000000000000, 1.000000000000000000, 1.000000000000000000, 1.000000000000000000, 1.000000000000000000, 1.000000000000000000, 1.000000000000000000, 1.000000000000000000, 1.000000000000000000, 1.000000000000000000, 1.000000000000000000, 1.000000000000000000, 1.000000000000000000, 1.000000000000000000, 1.000000000000000000, 1.000000000000000000, 1.000000000000000000, 1.000000000000000000, 1.000000000000000000, 1.000000000000000000, 1.000000000000000000, 1.000000000000000000, 1.000000000000000000, 1.000000000000000000, 1.000000000000000000),
 ( 0.3333333333333333703, 0.3333333333333333703, 0.3333333333333333703, 0.3333333333333333703, 0.3333333333333333703, 0.3333333333333333703, 0.3333333333333333703, 0.3333333333333333703, 0.3333333333333333703, 0.3333333333333333703, 0.3333333333333333703, 0.3333333333333333703, 0.3333333333333333703, 0.3333333333333333703, 0.3333333333333333703, 0.3333333333333333703, 0.3333333333333333703, 0.3333333333333333703, 0.3333333333333333703, 0.3333333333333333703, 0.3333333333333333703, 0.3333333333333333703, 0.3333333333333333703, 0.3333333333333333703, 0.3333333333333333703, 0.3333333333333333703, 0.3333333333333333703, 0.3333333333333333703, 0.3333333333333333703, 0.3333333333333333703),
 ( 0.3333333333333333703, 0.3333333333333333703, 0.3333333333333333703, 0.3333333333333333703, 0.3333333333333333703, 0.3333333333333333703, 0.3333333333333333703, 0.3333333333333333703, 0.3333333333333333703, 0.3333333333333333703, 0.3333333333333333703, 0.3333333333333333703, 0.3333333333333333703, 0.3333333333333333703, 0.3333333333333333703, 0.3333333333333333703, 0.3333333333333333703, 0.3333333333333333703, 0.3333333333333333703, 0.3333333333333333703, 0.3333333333333333703, 0.3333333333333333703, 0.3333333333333333703, 0.3333333333333333703, 0.3333333333333333703, 0.3333333333333333703, 0.3333333333333333703, 0.3333333333333333703, 0.3333333333333333703, 0.3333333333333333703),
 ( 1.000000000000000000, 1.000000000000000000, 1.000000000000000000, 1.000000000000000000, 1.000000000000000000, 1.000000000000000000, 1.000000000000000000, 1.000000000000000000, 1.000000000000000000, 1.000000000000000000, 1.000000000000000000, 1.000000000000000000, 1.000000000000000000, 1.000000000000000000, 1.000000000000000000, 1.000000000000000000, 1.000000000000000000, 1.000000000000000000, 1.000000000000000000, 1.000000000000000000, 1.000000000000000000, 1.000000000000000000, 1.000000000000000000, 1.000000000000000000, 1.000000000000000000, 1.000000000000000000, 1.000000000000000000, 1.000000000000000000, 1.000000000000000000, 1.000000000000000000),
 ( 0.3333333333333333703, 0.3333333333333333703, 0.3333333333333333703, 0.3333333333333333703, 0.3333333333333333703, 0.3333333333333333703, 0.3333333333333333703, 0.3333333333333333703, 0.3333333333333333703, 0.3333333333333333703, 0.3333333333333333703, 0.3333333333333333703, 0.3333333333333333703, 0.3333333333333333703, 0.3333333333333333703, 0.3333333333333333703, 0.3333333333333333703, 0.3333333333333333703, 0.3333333333333333703, 0.3333333333333333703, 0.3333333333333333703, 0.3333333333333333703, 0.3333333333333333703, 0.3333333333333333703, 0.3333333333333333703, 0.3333333333333333703, 0.3333333333333333703, 0.3333333333333333703, 0.3333333333333333703, 0.3333333333333333703),
 ( 0.3333333333333333703, 0.3333333333333333703, 0.3333333333333333703, 0.3333333333333333703, 0.3333333333333333703, 0.3333333333333333703, 0.3333333333333333703, 0.3333333333333333703, 0.3333333333333333703, 0.3333333333333333703, 0.3333333333333333703, 0.3333333333333333703, 0.3333333333333333703, 0.3333333333333333703, 0.3333333333333333703, 0.3333333333333333703, 0.3333333333333333703, 0.3333333333333333703, 0.3333333333333333703, 0.3333333333333333703, 0.3333333333333333703, 0.3333333333333333703, 0.3333333333333333703, 0.3333333333333333703, 0.3333333333333333703, 0.3333333333333333703, 0.3333333333333333703, 0.3333333333333333703, 0.3333333333333333703, 0.3333333333333333703),
 ( 1.000000000000000000, 1.000000000000000000, 1.000000000000000000, 1.000000000000000000, 1.000000000000000000, 1.000000000000000000, 1.000000000000000000, 1.000000000000000000, 1.000000000000000000, 1.000000000000000000, 1.000000000000000000, 1.000000000000000000, 1.000000000000000000, 1.000000000000000000, 1.000000000000000000, 1.000000000000000000, 1.000000000000000000, 1.000000000000000000, 1.000000000000000000, 1.000000000000000000, 1.000000000000000000, 1.000000000000000000, 1.000000000000000000, 1.000000000000000000, 1.000000000000000000, 1.000000000000000000, 1.000000000000000000, 1.000000000000000000, 1.000000000000000000, 1.000000000000000000) ) ) 
 REPRESENTATION_ITEM ( '' )  SURFACE ( )  );
#12276 = CARTESIAN_POINT ( 'NONE',  ( -632.1051217044982877, 26.93102622738082630, 29.57723565074837069 ) ) ;
#12277 = CARTESIAN_POINT ( 'NONE',  ( 190.0000000000000000, 7.164183775012017527E-14, 0.000000000000000000 ) ) ;
#12278 = CARTESIAN_POINT ( 'NONE',  ( 199.0191753821509622, 9.128090787448098098, 17.79799345705162139 ) ) ;
#12279 = CARTESIAN_POINT ( 'NONE',  ( -114.4098922876147384, 20.15198150140922451, 8.347224046571190215 ) ) ;
#12280 = CARTESIAN_POINT ( 'NONE',  ( -1.087763065926164341, -24.03018639663240918, -43.78960619332526960 ) ) ;
#12281 = CARTESIAN_POINT ( 'NONE',  ( 19.06497207195982568, -38.31983398719592770, -38.31983398719660272 ) ) ;
#12282 = CARTESIAN_POINT ( 'NONE',  ( -114.4364955367319396, 8.064892380839246755, -20.29001642038913644 ) ) ;
#12283 = CARTESIAN_POINT ( 'NONE',  ( 163.1118516004056573, -9.006482792073960297, -47.56205970284963769 ) ) ;
#12284 = CARTESIAN_POINT ( 'NONE',  ( 184.8905102610680444, 20.92133201514447549, 0.000000000000000000 ) ) ;
#12285 = CARTESIAN_POINT ( 'NONE',  ( -105.3755690713226727, -18.24025645688354302, -2.449293598294708485E-15 ) ) ;
#12286 = CARTESIAN_POINT ( 'NONE',  ( 130.8568914410475372, 24.07718906447243867, -24.07718906447216156 ) ) ;
#12287 = CARTESIAN_POINT ( 'NONE',  ( 4.995406935893309530, -55.24977328856464709, 40.00000000000002132 ) ) ;
#12288 = CARTESIAN_POINT ( 'NONE',  ( -100.0753760173604405, 20.72827493166397161, -8.149786832858799457 ) ) ;
#12289 = CARTESIAN_POINT ( 'NONE',  ( -105.3755690713226585, 39.99999999999977263, 21.75974354311691883 ) ) ;
#12290 = CARTESIAN_POINT ( 'NONE',  ( -162.0762913951021176, 29.48230308784768638, -27.08623940707612121 ) ) ;
#12291 = CARTESIAN_POINT ( 'NONE',  ( 184.8905102610680444, -20.92133201514440799, -40.00000000000002132 ) ) ;
#12292 = ORIENTED_EDGE ( 'NONE', *, *, #13997, .F. ) ;
#12293 = EDGE_LOOP ( 'NONE', ( #15926, #7527, #23971, #11819 ) ) ;
#12294 = AXIS2_PLACEMENT_3D ( 'NONE', #24193, #5966, #14077 ) ;
#12295 = CARTESIAN_POINT ( 'NONE',  ( -93.02511667906878756, -8.169918093965518935, -20.82219708225685295 ) ) ;
#12296 = CARTESIAN_POINT ( 'NONE',  ( 184.8905102610680444, 41.77492675555983936, 14.79361573936436081 ) ) ;
#12297 = CARTESIAN_POINT ( 'NONE',  ( -265.0000000000000000, -10.00000000000004796, -6.532754371361504014E-30 ) ) ;
#12298 = DIRECTION ( 'NONE',  ( 0.000000000000000000, 0.000000000000000000, -1.000000000000000000 ) ) ;
#12299 = DIRECTION ( 'NONE',  ( 0.000000000000000000, 0.000000000000000000, -1.000000000000000000 ) ) ;
#12300 = CARTESIAN_POINT ( 'NONE',  ( 199.9999999999998295, 18.60987205011830881, -3.837998380785754726 ) ) ;
#12301 = CARTESIAN_POINT ( 'NONE',  ( 199.9999999999998863, -19.00899821966885028, 0.6240211523505900804 ) ) ;
#12302 = CARTESIAN_POINT ( 'NONE',  ( 192.4448373802100889, 14.14213562370330379, -14.14213562370292365 ) ) ;
#12303 = CARTESIAN_POINT ( 'NONE',  ( -30.26275506840324070, -29.48230279907817675, 27.08623969584564151 ) ) ;
#12304 = CARTESIAN_POINT ( 'NONE',  ( -110.0763310915540529, 19.64189236472208933, 4.694460244226943857 ) ) ;
#12305 = CARTESIAN_POINT ( 'NONE',  ( -30.26275506840324425, 40.00000000000044764, -41.69427246844585255 ) ) ;
#12306 = CARTESIAN_POINT ( 'NONE',  ( -86.96347745069643054, -41.18208027870611687, 15.38646221621750954 ) ) ;
#12307 = EDGE_CURVE ( 'NONE', #15838, #5421, #19317, .T. ) ;
#12308 = DIRECTION ( 'NONE',  ( 1.000000000000000000, 1.836970198721030427E-16, -0.000000000000000000 ) ) ;
#12309 = CARTESIAN_POINT ( 'NONE',  ( -100.7734535825088500, -44.31723036834903695, 12.25131212657476709 ) ) ;
#12310 = CARTESIAN_POINT ( 'NONE',  ( 184.8905102610680444, -13.49065550809780412, -43.07788698682583828 ) ) ;
#12311 = CARTESIAN_POINT ( 'NONE',  ( 199.0164216790778084, 13.51997225171141892, 14.76318892796115811 ) ) ;
#12312 = VECTOR ( 'NONE', #18232, 1000.000000000000000 ) ;
#12314 = CARTESIAN_POINT ( 'NONE',  ( -100.7734535825088358, -8.145438380286941744E-14, 17.32597176626811120 ) ) ;
#12313 = CARTESIAN_POINT ( 'NONE',  ( -162.0762913951020892, 1.198031840456041497, -57.76657433537918251 ) ) ;
#12315 = CARTESIAN_POINT ( 'NONE',  ( -105.3755690713226585, 41.18208027870575449, 15.38646221621837107 ) ) ;
#12316 = CARTESIAN_POINT ( 'NONE',  ( 23.49666234703815704, 42.81942870555077008, -23.31470603676260467 ) ) ;
#12317 = CARTESIAN_POINT ( 'NONE',  ( 151.7948205124836250, 6.767089262349059275, 2.449293598294708485E-15 ) ) ;
#12318 = CARTESIAN_POINT ( 'NONE',  ( -30.26275506840324070, 1.694272468446254232, 0.000000000000000000 ) ) ;
#12319 =( BOUNDED_SURFACE ( )  B_SPLINE_SURFACE ( 3, 3, ( 
 ( #25894, #5273, #23878, #11134, #17618, #15493, #9129, #23623, #17244, #3401, #1280, #25636, #9388, #3530, #1543, #11254, #5403, #15621, #3277, #5525, #11375, #19627, #15750, #17495, #25382, #7134, #5655, #13378, #13760, #19249 ),
 ( #15376, #23499, #21887, #21505, #13503, #19496, #1160, #1412, #21625, #9648, #15247, #9513, #25763, #7513, #23744, #23378, #9264, #13632, #5153, #21757, #11631, #19753, #13258, #21381, #7258, #3153, #19373, #17371, #14434, #16433 ),
 ( #19891, #10049, #11908, #15884, #20429, #1809, #3943, #17883, #14301, #24559, #1676, #7769, #18423, #6314, #22299, #10182, #9912, #16026, #1941, #18018, #72, #24010, #201, #26167, #18286, #16298, #9781, #8309, #18155, #24422 ),
 ( #14035, #6187, #2208, #22031, #20031, #26302, #3664, #22435, #26032, #7907, #5790, #20160, #13898, #24151, #3804, #8181, #11772, #10317, #4212, #5928, #22169, #12040, #8045, #16161, #24296, #6064, #14166, #4075, #12302, #12177 ),
 ( #20298, #2075, #18560, #25097, #14963, #12434, #339, #8443, #8984, #12973, #2466, #20830, #16562, #24825, #17090, #745, #8849, #16830, #16959, #25222, #4606, #4737, #20700, #6975, #21096, #22693, #10984, #16692, #22563, #22829 ),
 ( #2605, #24692, #6578, #4342, #6845, #23098, #24965, #12702, #6447, #607, #20961, #10576, #19094, #874, #4869, #14563, #2876, #4469, #2742, #12566, #8714, #10846, #476, #8581, #20562, #14697, #6712, #10718, #18691, #12845 ),
 ( #18827, #14826, #22958, #2333, #18965, #10447, #13106, #25611, #25866, #3507, #9239, #15595, #23720, #21227, #19222, #5001, #17469, #7231, #23596, #23351, #17346, #17725, #21473, #3248, #2999, #19346, #1002, #15089, #13234, #23475 ) ),
 .UNSPECIFIED., .T., .F., .F. ) 
 B_SPLINE_SURFACE_WITH_KNOTS ( ( 4, 3, 4 ),
 ( 4, 2, 2, 2, 2, 2, 2, 2, 2, 2, 2, 2, 2, 2, 4 ),
 ( 0.000000000000000000, 0.5000000000000000000, 1.000000000000000000 ),
 ( 0.000000000000000000, 0.1357259735107005372, 0.1651108541090157700, 0.1944957347073310028, 0.3598804999793158710, 0.3867117631979620773, 0.4135430264166082281, 0.5789277916885930964, 0.6062785021374117456, 0.6336292125862302838, 0.8508620842112317728, 0.8814014469398914198, 0.9119408096685510667, 0.9559704048342755334, 1.000000000000000000 ),
 .UNSPECIFIED. ) 
 GEOMETRIC_REPRESENTATION_ITEM ( )  RATIONAL_B_SPLINE_SURFACE ( (
 ( 1.000000000000000000, 1.000000000000000000, 1.000000000000000000, 1.000000000000000000, 1.000000000000000000, 1.000000000000000000, 1.000000000000000000, 1.000000000000000000, 1.000000000000000000, 1.000000000000000000, 1.000000000000000000, 1.000000000000000000, 1.000000000000000000, 1.000000000000000000, 1.000000000000000000, 1.000000000000000000, 1.000000000000000000, 1.000000000000000000, 1.000000000000000000, 1.000000000000000000, 1.000000000000000000, 1.000000000000000000, 1.000000000000000000, 1.000000000000000000, 1.000000000000000000, 1.000000000000000000, 1.000000000000000000, 1.000000000000000000, 1.000000000000000000, 1.000000000000000000),
 ( 0.3333333333333333703, 0.3333333333333333703, 0.3333333333333333703, 0.3333333333333333703, 0.3333333333333333703, 0.3333333333333333703, 0.3333333333333333703, 0.3333333333333333703, 0.3333333333333333703, 0.3333333333333333703, 0.3333333333333333703, 0.3333333333333333703, 0.3333333333333333703, 0.3333333333333333703, 0.3333333333333333703, 0.3333333333333333703, 0.3333333333333333703, 0.3333333333333333703, 0.3333333333333333703, 0.3333333333333333703, 0.3333333333333333703, 0.3333333333333333703, 0.3333333333333333703, 0.3333333333333333703, 0.3333333333333333703, 0.3333333333333333703, 0.3333333333333333703, 0.3333333333333333703, 0.3333333333333333703, 0.3333333333333333703),
 ( 0.3333333333333333703, 0.3333333333333333703, 0.3333333333333333703, 0.3333333333333333703, 0.3333333333333333703, 0.3333333333333333703, 0.3333333333333333703, 0.3333333333333333703, 0.3333333333333333703, 0.3333333333333333703, 0.3333333333333333703, 0.3333333333333333703, 0.3333333333333333703, 0.3333333333333333703, 0.3333333333333333703, 0.3333333333333333703, 0.3333333333333333703, 0.3333333333333333703, 0.3333333333333333703, 0.3333333333333333703, 0.3333333333333333703, 0.3333333333333333703, 0.3333333333333333703, 0.3333333333333333703, 0.3333333333333333703, 0.3333333333333333703, 0.3333333333333333703, 0.3333333333333333703, 0.3333333333333333703, 0.3333333333333333703),
 ( 1.000000000000000000, 1.000000000000000000, 1.000000000000000000, 1.000000000000000000, 1.000000000000000000, 1.000000000000000000, 1.000000000000000000, 1.000000000000000000, 1.000000000000000000, 1.000000000000000000, 1.000000000000000000, 1.000000000000000000, 1.000000000000000000, 1.000000000000000000, 1.000000000000000000, 1.000000000000000000, 1.000000000000000000, 1.000000000000000000, 1.000000000000000000, 1.000000000000000000, 1.000000000000000000, 1.000000000000000000, 1.000000000000000000, 1.000000000000000000, 1.000000000000000000, 1.000000000000000000, 1.000000000000000000, 1.000000000000000000, 1.000000000000000000, 1.000000000000000000),
 ( 0.3333333333333333703, 0.3333333333333333703, 0.3333333333333333703, 0.3333333333333333703, 0.3333333333333333703, 0.3333333333333333703, 0.3333333333333333703, 0.3333333333333333703, 0.3333333333333333703, 0.3333333333333333703, 0.3333333333333333703, 0.3333333333333333703, 0.3333333333333333703, 0.3333333333333333703, 0.3333333333333333703, 0.3333333333333333703, 0.3333333333333333703, 0.3333333333333333703, 0.3333333333333333703, 0.3333333333333333703, 0.3333333333333333703, 0.3333333333333333703, 0.3333333333333333703, 0.3333333333333333703, 0.3333333333333333703, 0.3333333333333333703, 0.3333333333333333703, 0.3333333333333333703, 0.3333333333333333703, 0.3333333333333333703),
 ( 0.3333333333333333703, 0.3333333333333333703, 0.3333333333333333703, 0.3333333333333333703, 0.3333333333333333703, 0.3333333333333333703, 0.3333333333333333703, 0.3333333333333333703, 0.3333333333333333703, 0.3333333333333333703, 0.3333333333333333703, 0.3333333333333333703, 0.3333333333333333703, 0.3333333333333333703, 0.3333333333333333703, 0.3333333333333333703, 0.3333333333333333703, 0.3333333333333333703, 0.3333333333333333703, 0.3333333333333333703, 0.3333333333333333703, 0.3333333333333333703, 0.3333333333333333703, 0.3333333333333333703, 0.3333333333333333703, 0.3333333333333333703, 0.3333333333333333703, 0.3333333333333333703, 0.3333333333333333703, 0.3333333333333333703),
 ( 1.000000000000000000, 1.000000000000000000, 1.000000000000000000, 1.000000000000000000, 1.000000000000000000, 1.000000000000000000, 1.000000000000000000, 1.000000000000000000, 1.000000000000000000, 1.000000000000000000, 1.000000000000000000, 1.000000000000000000, 1.000000000000000000, 1.000000000000000000, 1.000000000000000000, 1.000000000000000000, 1.000000000000000000, 1.000000000000000000, 1.000000000000000000, 1.000000000000000000, 1.000000000000000000, 1.000000000000000000, 1.000000000000000000, 1.000000000000000000, 1.000000000000000000, 1.000000000000000000, 1.000000000000000000, 1.000000000000000000, 1.000000000000000000, 1.000000000000000000) ) ) 
 REPRESENTATION_ITEM ( '' )  SURFACE ( )  );
#12320 = CARTESIAN_POINT ( 'NONE',  ( -5.866564133084711585, -42.46617576965135044, 23.09290806363820892 ) ) ;
#12321 = CARTESIAN_POINT ( 'NONE',  ( -91.56559293963834989, 17.32597176626809343, 2.449293598294708485E-15 ) ) ;
#12322 = ORIENTED_EDGE ( 'NONE', *, *, #13513, .T. ) ;
#12323 = CARTESIAN_POINT ( 'NONE',  ( 1.564570055219367761, 24.39611894128515956, -44.28524390194891680 ) ) ;
#12324 = CARTESIAN_POINT ( 'NONE',  ( 19.06497207195980792, -18.24870850772763475, 38.31983398719622613 ) ) ;
#12325 = CARTESIAN_POINT ( 'NONE',  ( -24.53392603772963554, -19.42583462381907822, 36.88304647106062362 ) ) ;
#12326 = EDGE_CURVE ( 'NONE', #15177, #4560, #18388, .T. ) ;
#12327 =( GEOMETRIC_REPRESENTATION_CONTEXT ( 3 ) GLOBAL_UNCERTAINTY_ASSIGNED_CONTEXT ( ( #9539 ) ) GLOBAL_UNIT_ASSIGNED_CONTEXT ( ( #1206, #15173, #5198 ) ) REPRESENTATION_CONTEXT ( 'NONE', 'WORKASPACE' ) );
#12328 = CARTESIAN_POINT ( 'NONE',  ( -3.966425590329084372, 23.46521855348175478, -43.02666064534172818 ) ) ;
#12329 = CARTESIAN_POINT ( 'NONE',  ( 199.0188446093723371, -17.48804260178791736, -9.712431339257729945 ) ) ;
#12330 = CARTESIAN_POINT ( 'NONE',  ( -220.0000000000000284, 66.50000000000001421, -66.50000000000005684 ) ) ;
#12331 = CARTESIAN_POINT ( 'NONE',  ( 98.29820294269173075, 19.99999999998819433, -2.308575297063409524E-13 ) ) ;
#12332 = CARTESIAN_POINT ( 'NONE',  ( -173.7925586253262793, -12.78856870757000763, 41.93433064647447139 ) ) ;
#12333 = CARTESIAN_POINT ( 'NONE',  ( -192.9588430854690273, 10.23066800229588758, -66.79921049721882298 ) ) ;
#12334 = CARTESIAN_POINT ( 'NONE',  ( 4.995406935893293543, -15.24977328854832592, 0.000000000000000000 ) ) ;
#12336 = CARTESIAN_POINT ( 'NONE',  ( -259.2033419157646676, 21.55415060305790931, 35.01439189186571355 ) ) ;
#12335 = CARTESIAN_POINT ( 'NONE',  ( -190.7346372395231811, 23.92885340723965726, -43.65255821759343036 ) ) ;
#12337 = CARTESIAN_POINT ( 'NONE',  ( -238.4067589809705794, 28.96627169325285678, 27.60227080167094726 ) ) ;
#12338 = CARTESIAN_POINT ( 'NONE',  ( -30.26275506840323004, -41.69427246844629309, 40.00000000000002132 ) ) ;
#12339 = CARTESIAN_POINT ( 'NONE',  ( -56.48582580120559982, 30.84685318188643421, 40.00000000000002132 ) ) ;
#12340 = CARTESIAN_POINT ( 'NONE',  ( -56.48582580120559271, -1.062504017861011783E-13, 9.153146818113587102 ) ) ;
#12341 = CARTESIAN_POINT ( 'NONE',  ( 57.59792236341147031, 26.56190807104684382, 26.56190807104692553 ) ) ;
#12342 = CARTESIAN_POINT ( 'NONE',  ( -103.9650464695150021, 20.03380587595252393, -8.298274099110376056 ) ) ;
#12343 = CARTESIAN_POINT ( 'NONE',  ( 200.0000000000000000, 42.42640687119310172, -14.14213562373052646 ) ) ;
#12344 = ORIENTED_EDGE ( 'NONE', *, *, #3474, .T. ) ;
#12345 = CARTESIAN_POINT ( 'NONE',  ( 19.06497207195980792, -18.24870850772763475, 38.31983398719622613 ) ) ;
#12346 = CARTESIAN_POINT ( 'NONE',  ( -105.4741150117389026, 7.943527260749601027, 19.77569912955131315 ) ) ;
#12347 = ORIENTED_EDGE ( 'NONE', *, *, #22794, .F. ) ;
#12348 = CARTESIAN_POINT ( 'NONE',  ( 14.38125909742183062, -67.30136555898262429, 10.73282306405838682 ) ) ;
#12349 = CARTESIAN_POINT ( 'NONE',  ( 6.202588567992542323, -44.80189419270367779, -24.77700748805923681 ) ) ;
#12350 = EDGE_LOOP ( 'NONE', ( #24342, #18102 ) ) ;
#12351 = CARTESIAN_POINT ( 'NONE',  ( 22.27434459959404478, -47.22399357554351695, -13.86259002508720073 ) ) ;
#12352 = CARTESIAN_POINT ( 'NONE',  ( -87.13361725306405958, -14.23663034390084725, -16.15936608143848474 ) ) ;
#12353 = VERTEX_POINT ( 'NONE', #19830 ) ;
#12354 = CARTESIAN_POINT ( 'NONE',  ( 199.9999999999996305, 11.56193655722446678, 15.09741884674619072 ) ) ;
#12355 = CARTESIAN_POINT ( 'NONE',  ( -105.2054292635175585, 21.49321519473984665, 5.610018989487960791E-28 ) ) ;
#12356 = CARTESIAN_POINT ( 'NONE',  ( 136.1360204305621266, -24.77266263493116583, -24.77266263493127951 ) ) ;
#12357 = CARTESIAN_POINT ( 'NONE',  ( -173.7925586252841015, -38.69493321942316300, -20.60916591006939669 ) ) ;
#12358 = CARTESIAN_POINT ( 'NONE',  ( -91.56559293963834989, -40.00000000000009948, 17.32597176626796553 ) ) ;
#12359 = CARTESIAN_POINT ( 'NONE',  ( -238.4067589809705794, 40.96449427990177128, 40.00000000000002132 ) ) ;
#12360 = CARTESIAN_POINT ( 'NONE',  ( 170.2234770963711128, -45.64576402573167258, -10.92277846919254891 ) ) ;
#12361 = CARTESIAN_POINT ( 'NONE',  ( 199.0262408397048262, -11.66336112630027877, 16.25405011469380057 ) ) ;
#12362 = VECTOR ( 'NONE', #4302, 1000.000000000000000 ) ;
#12363 = AXIS2_PLACEMENT_3D ( 'NONE', #24628, #22506, #20501 ) ;
#12364 = CARTESIAN_POINT ( 'NONE',  ( 14.38125909742181108, -5.035366881890652543E-14, 15.17850393972633682 ) ) ;
#12365 = CARTESIAN_POINT ( 'NONE',  ( 91.82158438592159655, -40.00000000000008527, 22.79471317813456110 ) ) ;
#12366 = AXIS2_PLACEMENT_3D ( 'NONE', #7832, #9324, #868 ) ;
#12367 = CARTESIAN_POINT ( 'NONE',  ( -56.48582580120559271, 2.158176344243877536E-14, -9.153146818113587102 ) ) ;
#12368 = CARTESIAN_POINT ( 'NONE',  ( -135.8532207217289738, 9.153146818113546246, -0.000000000000000000 ) ) ;
#12369 = CARTESIAN_POINT ( 'NONE',  ( -259.2033419157646676, -21.55415060305854524, 21.55415060305827524 ) ) ;
#12370 = CARTESIAN_POINT ( 'NONE',  ( 91.82158438592159655, -22.79471317813468545, -2.449293598294708485E-15 ) ) ;
#12371 = CARTESIAN_POINT ( 'NONE',  ( -259.2033419157646676, 35.01439189186528722, 21.55415060305857011 ) ) ;
#12372 = CARTESIAN_POINT ( 'NONE',  ( 132.4338126186516149, -12.33615677966328938, -29.78211700502419390 ) ) ;
#12373 = DIRECTION ( 'NONE',  ( -1.000000000000000000, 0.000000000000000000, 0.000000000000000000 ) ) ;
#12374 = CARTESIAN_POINT ( 'NONE',  ( 19.06497207195981858, 5.735870351258996432E-13, -54.19242893257843008 ) ) ;
#12375 = CARTESIAN_POINT ( 'NONE',  ( -135.8532207217289738, -1.351063376314938213E-13, 30.84685318188645553 ) ) ;
#12376 = CARTESIAN_POINT ( 'NONE',  ( -91.56559293963834989, 12.25131212657490209, -44.31723036834897300 ) ) ;
#12377 = LINE ( 'NONE', #10659, #22411 ) ;
#12378 = CARTESIAN_POINT ( 'NONE',  ( -198.0356074513804572, 10.87444709759730088, -10.87444709759707173 ) ) ;
#12379 = CARTESIAN_POINT ( 'NONE',  ( 200.0000000000000000, -14.14213562373062949, -42.42640687119301646 ) ) ;
#12380 = ORIENTED_EDGE ( 'NONE', *, *, #7828, .F. ) ;
#12381 = CARTESIAN_POINT ( 'NONE',  ( 146.6084372240433709, -24.48358557860284179, -32.08495691632087699 ) ) ;
#12382 = DIRECTION ( 'NONE',  ( -1.000000000000000000, 1.836970198721030181E-16, 0.000000000000000000 ) ) ;
#12383 = CARTESIAN_POINT ( 'NONE',  ( -238.4067589809705510, -40.96449427998265946, -2.449293598294708485E-15 ) ) ;
#12384 = EDGE_CURVE ( 'NONE', #17327, #993, #23414, .T. ) ;
#12385 = LINE ( 'NONE', #10132, #24658 ) ;
#12386 = FACE_OUTER_BOUND ( 'NONE', #9796, .T. ) ;
#12387 =( LENGTH_UNIT ( ) NAMED_UNIT ( * ) SI_UNIT ( .MILLI., .METRE. ) );
#12388 = VERTEX_POINT ( 'NONE', #15441 ) ;
#12389 = ORIENTED_EDGE ( 'NONE', *, *, #22824, .T. ) ;
#12390 = CIRCLE ( 'NONE', #5180, 5.000000000000004441 ) ;
#12391 = CARTESIAN_POINT ( 'NONE',  ( 199.9999999999998863, 17.32309309515417439, -7.829923752638988432 ) ) ;
#12392 = CARTESIAN_POINT ( 'NONE',  ( -716.9846540392142060, -66.50000000000001421, 71.50000000000005684 ) ) ;
#12393 = CARTESIAN_POINT ( 'NONE',  ( 22.17571259162583175, 13.86510691866999778, 47.24006242885730700 ) ) ;
#12394 = VERTEX_POINT ( 'NONE', #7454 ) ;
#12395 = EDGE_LOOP ( 'NONE', ( #7015, #16373, #463, #3621 ) ) ;
#12396 = CARTESIAN_POINT ( 'NONE',  ( 170.2234770963711128, -24.55285855007183926, 0.000000000000000000 ) ) ;
#12397 = CARTESIAN_POINT ( 'NONE',  ( 199.0132273568269170, -10.00203194272371476, -17.32088655864767190 ) ) ;
#12398 = CARTESIAN_POINT ( 'NONE',  ( -77.70104068030501310, -11.20636163163649535, -18.98731336402689962 ) ) ;
#12399 = ADVANCED_FACE ( 'NONE', ( #15569 ), #19569, .T. ) ;
#12400 = EDGE_CURVE ( 'NONE', #12121, #16316, #4326, .T. ) ;
#12401 = CARTESIAN_POINT ( 'NONE',  ( -135.8532207217289738, -6.472252184284190690, -6.472252184284188914 ) ) ;
#12402 = CARTESIAN_POINT ( 'NONE',  ( 98.29820294273055481, 14.14213562373424971, 14.14213562373465294 ) ) ;
#12403 = CARTESIAN_POINT ( 'NONE',  ( 136.1360204305621266, 7.947488714877270288E-14, -4.966164525587064560 ) ) ;
#12404 = CARTESIAN_POINT ( 'NONE',  ( -208.1127848780265026, 1.189126717069624012E-13, -15.00245453012669472 ) ) ;
#12405 = VECTOR ( 'NONE', #22187, 1000.000000000000000 ) ;
#12406 = CARTESIAN_POINT ( 'NONE',  ( 180.0000000000000000, -66.50000000000001421, -66.50000000000005684 ) ) ;
#12407 = CARTESIAN_POINT ( 'NONE',  ( 199.0147602753770855, 15.66021538362855381, 12.44349737331557648 ) ) ;
#12408 = CARTESIAN_POINT ( 'NONE',  ( -188.9001212172966291, 17.93766612258000848, 43.30535683045329165 ) ) ;
#12409 = CARTESIAN_POINT ( 'NONE',  ( -56.48582580120558561, -21.81201906317755146, -21.81201906317792449 ) ) ;
#12410 = CARTESIAN_POINT ( 'NONE',  ( -200.0000000000000000, 14.89048929005512001, 48.59548038928821967 ) ) ;
#12411 = CARTESIAN_POINT ( 'NONE',  ( 146.6084372240433709, 24.48358557860311180, 32.08495691632071356 ) ) ;
#12412 = CARTESIAN_POINT ( 'NONE',  ( 23.37394308801978582, -46.80823611210187352, -13.80096434448294396 ) ) ;
#12413 = CARTESIAN_POINT ( 'NONE',  ( -105.3755690713226585, 15.38646221621820764, -41.18208027870583265 ) ) ;
#12414 = CARTESIAN_POINT ( 'NONE',  ( -653.0498733801694016, 38.46191729815036808, 23.36466092414772078 ) ) ;
#12415 = CARTESIAN_POINT ( 'NONE',  ( -86.96347745069645896, 21.75974354311648895, 40.00000000000002132 ) ) ;
#12416 = CARTESIAN_POINT ( 'NONE',  ( -100.7734535825088358, -16.03295912088728770, 16.03295912088687913 ) ) ;
#12417 = CARTESIAN_POINT ( 'NONE',  ( 136.1360204305621551, -4.966164525587043244, 40.00000000000002132 ) ) ;
#12418 = CARTESIAN_POINT ( 'NONE',  ( 200.0000000000000000, -66.50000000000001421, -66.50000000000005684 ) ) ;
#12419 = CARTESIAN_POINT ( 'NONE',  ( 192.4448373802101173, 39.99999999999985079, 20.00000000003984013 ) ) ;
#12420 = CARTESIAN_POINT ( 'NONE',  ( 14.38125909742180220, 39.01709431150916885, -17.55144818341463164 ) ) ;
#12421 = CARTESIAN_POINT ( 'NONE',  ( 184.8905102610680444, -20.92133201514440799, 0.000000000000000000 ) ) ;
#12422 = ORIENTED_EDGE ( 'NONE', *, *, #20621, .F. ) ;
#12423 = ORIENTED_EDGE ( 'NONE', *, *, #13205, .F. ) ;
#12424 = FACE_OUTER_BOUND ( 'NONE', #22816, .T. ) ;
#12425 = EDGE_CURVE ( 'NONE', #6406, #14842, #3163, .T. ) ;
#12426 = FACE_OUTER_BOUND ( 'NONE', #4096, .T. ) ;
#12427 =( BOUNDED_SURFACE ( )  B_SPLINE_SURFACE ( 3, 2, ( 
 ( #10100, #14355, #124 ),
 ( #10233, #4655, #4525 ),
 ( #22616, #2386, #24610 ),
 ( #18611, #6766, #10767 ),
 ( #12352, #20611, #12623 ),
 ( #23018, #14483, #4392 ) ),
 .UNSPECIFIED., .F., .F., .F. ) 
 B_SPLINE_SURFACE_WITH_KNOTS ( ( 4, 2, 4 ),
 ( 3, 3 ),
 ( 0.04143179630788233064, 0.04845754690455064684, 0.05548329750121896997 ),
 ( 0.000000000000000000, 1.000000000000000000 ),
 .UNSPECIFIED. ) 
 GEOMETRIC_REPRESENTATION_ITEM ( )  RATIONAL_B_SPLINE_SURFACE ( (
 ( 1.000000000000000000, 0.9541700779530457588, 1.000000000000000000),
 ( 1.000000000000000000, 0.9520119187990010445, 1.000000000000000000),
 ( 1.000000000000000000, 0.9503150779442263163, 1.000000000000000000),
 ( 1.000000000000000000, 0.9480088369839682061, 1.000000000000000000),
 ( 1.000000000000000000, 0.9474362540968070956, 1.000000000000000000),
 ( 1.000000000000000000, 0.9474350314971540232, 1.000000000000000000) ) ) 
 REPRESENTATION_ITEM ( '' )  SURFACE ( )  );
#12428 = CARTESIAN_POINT ( 'NONE',  ( -238.4067589809705794, 57.25054294065799354, -0.6820004457334954973 ) ) ;
#12429 = CARTESIAN_POINT ( 'NONE',  ( -110.0368417077419707, -18.74474319002903755, -7.441767003006645176 ) ) ;
#12430 = LINE ( 'NONE', #471, #2366 ) ;
#12431 = CARTESIAN_POINT ( 'NONE',  ( -87.08883615166497805, 3.401706263181337508, -21.20174225584124272 ) ) ;
#12432 = CARTESIAN_POINT ( 'NONE',  ( 200.0000000000003126, 10.03286793820859835, -16.13825081434616493 ) ) ;
#12433 = CARTESIAN_POINT ( 'NONE',  ( 199.9999999999999716, 6.682634084700803889, -17.78923626348730735 ) ) ;
#12434 = CARTESIAN_POINT ( 'NONE',  ( -198.0356074513804572, 10.87444709761036066, -67.44298959253325165 ) ) ;
#12435 = CARTESIAN_POINT ( 'NONE',  ( 151.7948205124836534, -33.06932595376376582, 23.49921654115996006 ) ) ;
#12436 = PLANE ( 'NONE',  #13969 ) ;
#12437 = CARTESIAN_POINT ( 'NONE',  ( -213.1075012329537230, 40.00000000000012790, -13.71589010951869980 ) ) ;
#12438 = CARTESIAN_POINT ( 'NONE',  ( 57.59792236341148453, -26.56190807104663421, -26.56190807104710672 ) ) ;
#12439 = CARTESIAN_POINT ( 'NONE',  ( 14.32711937312299000, 14.14294248749819793, 49.08922911798401145 ) ) ;
#12440 = CARTESIAN_POINT ( 'NONE',  ( -126.6834156231698927, -11.16464796295173123, -24.04426801070755459 ) ) ;
#12441 = CARTESIAN_POINT ( 'NONE',  ( -30.26275506840324070, -1.198031551616032919, 1.198031551616014712 ) ) ;
#12442 = CARTESIAN_POINT ( 'NONE',  ( 199.0179910436408761, 11.13570414284889409, 16.62722890173126444 ) ) ;
#12444 = CARTESIAN_POINT ( 'NONE',  ( 146.6084372240433709, 40.00000000000003553, 5.374981219217116468 ) ) ;
#12443 = CARTESIAN_POINT ( 'NONE',  ( -208.1127848780264742, 10.60833733268383483, -67.17687982760675425 ) ) ;
#12445 = B_SPLINE_CURVE_WITH_KNOTS ( 'NONE', 3,
 ( #19165, #4817, #12920, #21036, #15170, #23420, #7173, #11174, #2819, #16768, #10928, #8660, #19039, #818, #7055, #17034 ),
 .UNSPECIFIED., .F., .F.,
 ( 4, 2, 2, 2, 2, 2, 2, 4 ),
 ( 0.0003132551799524981831, 0.004485156913506553947, 0.006571107780283581314, 0.008657058647060608680, 0.01282896038061466341, 0.01387193581400317753, 0.01491491124739169165, 0.01700086211416872509 ),
 .UNSPECIFIED. ) ;
#12446 = CARTESIAN_POINT ( 'NONE',  ( -192.9588430854690273, 38.51493924976913519, 18.05360324515490333 ) ) ;
#12447 = CARTESIAN_POINT ( 'NONE',  ( 22.31419732599935557, 43.29699898481473497, -17.93420418956763029 ) ) ;
#12448 = CARTESIAN_POINT ( 'NONE',  ( 146.6084372240433993, 5.374981219216999229, 2.449293598294708485E-15 ) ) ;
#12449 = CARTESIAN_POINT ( 'NONE',  ( 190.0000000000000000, 7.164183775012017527E-14, 0.000000000000000000 ) ) ;
#12450 = CARTESIAN_POINT ( 'NONE',  ( 130.8568914410475372, -24.07718906447222551, -24.07718906447233209 ) ) ;
#12451 = CARTESIAN_POINT ( 'NONE',  ( -4.037857402784122307, -46.99101396955040144, 13.82822410908682720 ) ) ;
#12452 = CARTESIAN_POINT ( 'NONE',  ( 14.38125909742180752, 55.17850393972636880, 2.449293598294708485E-15 ) ) ;
#12453 = EDGE_LOOP ( 'NONE', ( #24436, #13212, #5310, #3361 ) ) ;
#12454 = B_SPLINE_CURVE_WITH_KNOTS ( 'NONE', 3,
 ( #10336, #498, #20849, #18583, #362, #8868 ),
 .UNSPECIFIED., .F., .F.,
 ( 4, 2, 4 ),
 ( 0.000000000000000000, 0.004324493460679611212, 0.008648986921359222424 ),
 .UNSPECIFIED. ) ;
#12455 = CARTESIAN_POINT ( 'NONE',  ( -280.0000000000000568, -42.42640687119295251, 14.14213562373088351 ) ) ;
#12456 = CARTESIAN_POINT ( 'NONE',  ( -5.859158571327203191, -13.69949429424866949, 46.35984297723813086 ) ) ;
#12457 = CARTESIAN_POINT ( 'NONE',  ( -4.121597284766315816, 13.82232031192010702, -46.96202426942429753 ) ) ;
#12458 = CARTESIAN_POINT ( 'NONE',  ( 199.0137359473271488, -10.84478214295758036, -16.80398351328055639 ) ) ;
#12459 = CARTESIAN_POINT ( 'NONE',  ( -238.4067589809705794, -3.369206980223063916E-14, -0.9644942799825824142 ) ) ;
#12460 = CARTESIAN_POINT ( 'NONE',  ( -575.0231298121466352, 90.00000000000000000, -35.00000000000203926 ) ) ;
#12461 = CARTESIAN_POINT ( 'NONE',  ( -188.8384220655403851, -17.93083973458498193, 43.28887647197261401 ) ) ;
#12462 = CARTESIAN_POINT ( 'NONE',  ( -208.1127848780265026, 10.60833733269551615, -10.60833733269529766 ) ) ;
#12463 = CARTESIAN_POINT ( 'NONE',  ( -259.2033419157646676, 9.517827891722584255, -0.000000000000000000 ) ) ;
#12465 = CARTESIAN_POINT ( 'NONE',  ( 163.1118516004056573, 9.006482792073693844, 47.56205970284970164 ) ) ;
#12464 = CARTESIAN_POINT ( 'NONE',  ( -188.9524938555910296, 23.58789616778520326, -43.19211203807366672 ) ) ;
#12466 = CARTESIAN_POINT ( 'NONE',  ( 91.82158438592158234, 16.11829626348378142, 40.45024623143977749 ) ) ;
#12467 = EDGE_CURVE ( 'NONE', #2889, #22287, #2871, .T. ) ;
#12468 = CARTESIAN_POINT ( 'NONE',  ( 184.8905102610680444, -19.07866798485553872, -40.00000000000002132 ) ) ;
#12469 = CARTESIAN_POINT ( 'NONE',  ( 184.8905102610680444, 19.07866798485561333, 40.00000000000002132 ) ) ;
#12470 = CARTESIAN_POINT ( 'NONE',  ( 19.06497207195981147, 1.521599808664285085E-13, -14.19242893257840521 ) ) ;
#12471 = CARTESIAN_POINT ( 'NONE',  ( -86.96347745069644475, -15.38646221621796073, 41.18208027870593924 ) ) ;
#12472 =( BOUNDED_CURVE ( )  B_SPLINE_CURVE ( 3, ( #15657, #3839, #13670, #18056 ),
 .UNSPECIFIED., .F., .F. ) 
 B_SPLINE_CURVE_WITH_KNOTS ( ( 4, 4 ),
 ( 0.01576650722535599680, 0.02368120503275411570 ),
 .UNSPECIFIED. ) 
 CURVE ( )  GEOMETRIC_REPRESENTATION_ITEM ( )  RATIONAL_B_SPLINE_CURVE ( ( 0.7232313460858506016, 0.6666666666666621888, 0.6208516971803421658, 0.5857864376268907547 ) ) 
 REPRESENTATION_ITEM ( '' )  );
#12473 = CARTESIAN_POINT ( 'NONE',  ( 98.29820294267490510, 4.808046699556526995E-12, 20.00000000000513722 ) ) ;
#12474 = CARTESIAN_POINT ( 'NONE',  ( -192.9588430854689705, -38.51493924976909966, -38.51493924976973915 ) ) ;
#12475 = CARTESIAN_POINT ( 'NONE',  ( 91.82158438592158234, 12.16597498397773869, -12.16597498397759303 ) ) ;
#12476 = ADVANCED_FACE ( 'NONE', ( #16503 ), #26245, .F. ) ;
#12477 = ORIENTED_EDGE ( 'NONE', *, *, #8006, .T. ) ;
#12478 = CARTESIAN_POINT ( 'NONE',  ( 57.59792236341147031, -30.00663442387700641, 26.56190807104681895 ) ) ;
#12479 = CARTESIAN_POINT ( 'NONE',  ( -88.38011430157065718, 8.298859908373991345, 20.03522014432801868 ) ) ;
#12480 = CARTESIAN_POINT ( 'NONE',  ( 136.1360204305621551, 24.77266263493108411, 31.79587985999273769 ) ) ;
#12481 = CARTESIAN_POINT ( 'NONE',  ( 19.66474694218199915, -43.90629905112487563, -18.18658454056792451 ) ) ;
#12482 = ADVANCED_FACE ( 'NONE', ( #24366, #24499, #20370, #18493, #8248, #3739 ), #15964, .F. ) ;
#12483 = ORIENTED_EDGE ( 'NONE', *, *, #3076, .T. ) ;
#12484 = CARTESIAN_POINT ( 'NONE',  ( 91.82158438592158234, -17.20528682183298486, 0.000000000000000000 ) ) ;
#12485 = FACE_OUTER_BOUND ( 'NONE', #14952, .T. ) ;
#12487 = ORIENTED_EDGE ( 'NONE', *, *, #20689, .T. ) ;
#12486 = ADVANCED_FACE ( 'NONE', ( #19965 ), #22239, .T. ) ;
#12488 = CARTESIAN_POINT ( 'NONE',  ( 199.9999999999999432, 15.63063699308155030, -10.80328371702407786 ) ) ;
#12489 = CARTESIAN_POINT ( 'NONE',  ( -215.0000000000000284, 75.52305771588336825, -68.47933392563552957 ) ) ;
#12490 = CARTESIAN_POINT ( 'NONE',  ( -190.0144721488272523, -43.47822244620601140, -23.79987203024255749 ) ) ;
#12491 = CARTESIAN_POINT ( 'NONE',  ( 0.2972598230770030492, -1.921041075453695163E-13, 54.33493731733936016 ) ) ;
#12492 = CARTESIAN_POINT ( 'NONE',  ( -105.3755690713226585, 18.24025645688350750, -40.00000000000002132 ) ) ;
#12493 = CARTESIAN_POINT ( 'NONE',  ( -86.96347745069644475, -15.38646221621807442, 15.38646221621768184 ) ) ;
#12494 = CARTESIAN_POINT ( 'NONE',  ( 199.0238195103507053, -1.318470765087343954, 19.97100952642404437 ) ) ;
#12495 = CARTESIAN_POINT ( 'NONE',  ( 91.82158438592159655, -40.00000000000008527, 22.79471317813456110 ) ) ;
#12496 = CARTESIAN_POINT ( 'NONE',  ( 136.1360204305621551, 40.00000000000017053, -35.03383547441281820 ) ) ;
#12497 = CARTESIAN_POINT ( 'NONE',  ( -199.9999999999999716, 82.50000000000008527, 52.49999999999977973 ) ) ;
#12498 = CARTESIAN_POINT ( 'NONE',  ( -86.96347745069645896, 21.75974354311648895, -0.000000000000000000 ) ) ;
#12499 = CARTESIAN_POINT ( 'NONE',  ( 57.59792236341148453, -37.56421063658185489, -2.449293598294708485E-15 ) ) ;
#12500 = CARTESIAN_POINT ( 'NONE',  ( -56.48582580120558561, 6.472252184283903809, 50.09629031063968796 ) ) ;
#12501 = CARTESIAN_POINT ( 'NONE',  ( 135.5356265174576720, -12.51227922893876787, -30.20731421070351530 ) ) ;
#12502 = DIRECTION ( 'NONE',  ( 1.000000000000000000, 1.836970198721030427E-16, -0.000000000000000000 ) ) ;
#12503 = CARTESIAN_POINT ( 'NONE',  ( -208.1127848780265026, 5.403397259664334602E-13, -55.00245453012672670 ) ) ;
#12504 = CARTESIAN_POINT ( 'NONE',  ( 19.06497207195981858, -1.881589693694111225E-13, 54.19242893257843008 ) ) ;
#12505 = CARTESIAN_POINT ( 'NONE',  ( -135.8532207217289738, -6.472252184284190690, -6.472252184284188914 ) ) ;
#12506 = CARTESIAN_POINT ( 'NONE',  ( 98.29820294273281434, -7.653668647304240125, 18.47759065023114644 ) ) ;
#12507 = DIRECTION ( 'NONE',  ( 4.657398277317547006E-32, -1.682156097916904081E-16, -1.000000000000000000 ) ) ;
#12508 = CARTESIAN_POINT ( 'NONE',  ( 19.06497207195982924, -66.60410523465823474, 10.03556273973400081 ) ) ;
#12509 = ORIENTED_EDGE ( 'NONE', *, *, #8329, .F. ) ;
#12510 = CARTESIAN_POINT ( 'NONE',  ( -47.65341557546879869, 29.74088027398482481, -14.80716566708708370 ) ) ;
#12511 = CARTESIAN_POINT ( 'NONE',  ( -626.9846540392142060, 90.00000000000000000, 0.000000000000000000 ) ) ;
#12512 = CARTESIAN_POINT ( 'NONE',  ( 151.7948205124836534, -6.767089262349000656, -40.00000000000002132 ) ) ;
#12513 = CARTESIAN_POINT ( 'NONE',  ( -87.11162894489362429, -2.713946817493684271, -21.34897934681563569 ) ) ;
#12514 = CARTESIAN_POINT ( 'NONE',  ( 4.995406935893289102, 10.78321810389013002, -10.78321810388986712 ) ) ;
#12515 = VERTEX_POINT ( 'NONE', #14373 ) ;
#12516 = ORIENTED_EDGE ( 'NONE', *, *, #21493, .F. ) ;
#12517 = CARTESIAN_POINT ( 'NONE',  ( 199.9999999999999716, -4.021883954748531664, 18.58191672459730981 ) ) ;
#12518 = CARTESIAN_POINT ( 'NONE',  ( -96.94449363886847948, 8.590991631032748543, -20.74048850978392977 ) ) ;
#12519 = CARTESIAN_POINT ( 'NONE',  ( 6.615221834194239925, 24.79576599682247107, 44.82734842560557809 ) ) ;
#12520 = VERTEX_POINT ( 'NONE', #8381 ) ;
#12521 = EDGE_LOOP ( 'NONE', ( #17543, #5577, #16782, #13977 ) ) ;
#12522 = CARTESIAN_POINT ( 'NONE',  ( -208.1127848780264742, 10.60833733270764867, 67.17687982763166588 ) ) ;
#12523 = CARTESIAN_POINT ( 'NONE',  ( 199.0256572979843099, -18.35487425740099354, 7.962169344204487409 ) ) ;
#12524 = CARTESIAN_POINT ( 'NONE',  ( -114.7827252410166778, 0.6830184494088376024, 22.13181612764241279 ) ) ;
#12525 = CARTESIAN_POINT ( 'NONE',  ( 85.88498484981873560, 23.37206192909128433, -8.769905300753718436 ) ) ;
#12526 = CARTESIAN_POINT ( 'NONE',  ( -100.7734535825088500, 40.53558337403677569, -16.03295912088699993 ) ) ;
#12527 = CARTESIAN_POINT ( 'NONE',  ( -199.9999999999999147, -14.17215463606695280, 49.28189405767609088 ) ) ;
#12528 = ADVANCED_FACE ( 'NONE', ( #12114 ), #14237, .T. ) ;
#12529 = CARTESIAN_POINT ( 'NONE',  ( 8.517493242715987734, 44.90626920808433198, -24.85395068094640081 ) ) ;
#12530 = CARTESIAN_POINT ( 'NONE',  ( -208.1127848780265026, 5.403397259664334602E-13, -55.00245453012672670 ) ) ;
#12531 = CARTESIAN_POINT ( 'NONE',  ( -208.1127848780264742, 40.00000000000014211, -15.00245453012627728 ) ) ;
#12532 = CARTESIAN_POINT ( 'NONE',  ( 170.0000000000000000, 3.062538285713190422, -24.95097643316999481 ) ) ;
#12533 = CARTESIAN_POINT ( 'NONE',  ( -211.2619052429883482, 0.000000000000000000, 0.000000000000000000 ) ) ;
#12534 = CARTESIAN_POINT ( 'NONE',  ( 199.0097993503064515, 19.72850438885342328, 3.281923459752313921 ) ) ;
#12535 = CARTESIAN_POINT ( 'NONE',  ( -187.7698581930736452, 13.79076165501289708, 46.80706826624406602 ) ) ;
#12536 = CARTESIAN_POINT ( 'NONE',  ( 163.1118516004056573, 19.27778845538753316, 19.27778845538783870 ) ) ;
#12537 = CARTESIAN_POINT ( 'NONE',  ( -200.0000000000000000, 16.05666331275189762, 47.66874763508933910 ) ) ;
#12538 = CARTESIAN_POINT ( 'NONE',  ( -208.1127848780264742, 17.67593391476624021, 38.89260858015742883 ) ) ;
#12539 = CARTESIAN_POINT ( 'NONE',  ( -210.0000000000000568, 82.50000000000008527, 52.49999999999980105 ) ) ;
#12540 = VECTOR ( 'NONE', #12031, 1000.000000000000000 ) ;
#12541 = AXIS2_PLACEMENT_3D ( 'NONE', #10694, #8284, #20538 ) ;
#12542 = CARTESIAN_POINT ( 'NONE',  ( -162.0762913951020892, -1.198031840315659124, -57.76657433523998009 ) ) ;
#12543 = CARTESIAN_POINT ( 'NONE',  ( 190.0000000000000000, -52.49999999999972289, -82.49999999999998579 ) ) ;
#12544 = CARTESIAN_POINT ( 'NONE',  ( 200.0000000000000000, 20.00000000000013856, 40.00000000000002132 ) ) ;
#12545 = EDGE_CURVE ( 'NONE', #7420, #4513, #2019, .T. ) ;
#12546 = CARTESIAN_POINT ( 'NONE',  ( -56.48582580120559271, -6.472252184284276844, 6.472252184284108978 ) ) ;
#12547 = CARTESIAN_POINT ( 'NONE',  ( 4.995406935893294431, -15.24977328854832415, 40.00000000000002132 ) ) ;
#12548 = CARTESIAN_POINT ( 'NONE',  ( -592.3028590817393706, 44.75291643641201489, 4.747045580819023947 ) ) ;
#12549 = CARTESIAN_POINT ( 'NONE',  ( 136.1360204305621266, 7.947488714877270288E-14, -4.966164525587064560 ) ) ;
#12550 = CARTESIAN_POINT ( 'NONE',  ( 199.0081457482208691, 0.8493142590133723191, -19.97879119992165187 ) ) ;
#12551 = CARTESIAN_POINT ( 'NONE',  ( 155.4809970915716519, -11.45899766888376448, 27.66446758342024737 ) ) ;
#12552 = ORIENTED_EDGE ( 'NONE', *, *, #3436, .T. ) ;
#12553 = ORIENTED_EDGE ( 'NONE', *, *, #17029, .F. ) ;
#12554 = CARTESIAN_POINT ( 'NONE',  ( -238.4067589809705794, 0.9644942799825385604, 40.00000000000002132 ) ) ;
#12555 = CIRCLE ( 'NONE', #5317, 30.00000000000005329 ) ;
#12556 = AXIS2_PLACEMENT_3D ( 'NONE', #24418, #18686, #6443 ) ;
#12557 = CARTESIAN_POINT ( 'NONE',  ( 19.06497207195981147, 38.31983398719673772, -38.31983398719579981 ) ) ;
#12558 = CARTESIAN_POINT ( 'NONE',  ( -726.9846540392142060, 66.50000000000009948, -71.50000000000005684 ) ) ;
#12559 = B_SPLINE_CURVE_WITH_KNOTS ( 'NONE', 3,
 ( #21244, #11368, #25114, #7246, #23368, #5144, #2761, #23491 ),
 .UNSPECIFIED., .F., .F.,
 ( 4, 2, 2, 4 ),
 ( 0.0002282271112605023934, 0.004312542793973171001, 0.006354700635329504736, 0.008396858476685838471 ),
 .UNSPECIFIED. ) ;
#12560 = ADVANCED_FACE ( 'NONE', ( #4284 ), #2273, .T. ) ;
#12561 = CARTESIAN_POINT ( 'NONE',  ( -189.4799804244524637, -43.33513910317152096, -23.69387126430435586 ) ) ;
#12562 = CARTESIAN_POINT ( 'NONE',  ( -210.0000000000000284, -71.50000000000002842, -66.50000000000005684 ) ) ;
#12563 = CARTESIAN_POINT ( 'NONE',  ( 199.9999999999998863, 3.552885321105354599, -18.66644157592937248 ) ) ;
#12564 = CIRCLE ( 'NONE', #7043, 14.99999999999999822 ) ;
#12565 = CARTESIAN_POINT ( 'NONE',  ( 199.9999999999999716, -4.928604136524651125, -18.35504861699862289 ) ) ;
#12566 = CARTESIAN_POINT ( 'NONE',  ( 57.59792236341147031, -30.00663442387662627, -26.56190807104723461 ) ) ;
#12567 = CARTESIAN_POINT ( 'NONE',  ( -198.0356074513804572, -10.87444709759714634, -10.87444709759729911 ) ) ;
#12568 = PRODUCT_DEFINITION_FORMATION_WITH_SPECIFIED_SOURCE ( 'ANY', '', #195, .NOT_KNOWN. ) ;
#12569 = DIRECTION ( 'NONE',  ( 1.000000000000000000, 0.000000000000000000, 0.000000000000000000 ) ) ;
#12570 = CARTESIAN_POINT ( 'NONE',  ( 4.995406935893291767, 40.00000000000059686, -55.24977328853165659 ) ) ;
#12571 = CIRCLE ( 'NONE', #9176, 29.99999999999999289 ) ;
#12572 = CARTESIAN_POINT ( 'NONE',  ( -86.86493150571114086, -7.943527260496002107, 19.77569912839178912 ) ) ;
#12573 = CARTESIAN_POINT ( 'NONE',  ( 163.1118516004056573, 27.26290988616875310, 0.000000000000000000 ) ) ;
#12574 = CARTESIAN_POINT ( 'NONE',  ( -280.0000000000000000, -14.14213562373098831, -14.14213562373098654 ) ) ;
#12575 = ADVANCED_FACE ( 'NONE', ( #10121 ), #14502, .T. ) ;
#12576 = EDGE_CURVE ( 'NONE', #1336, #16348, #3880, .T. ) ;
#12577 = CARTESIAN_POINT ( 'NONE',  ( 146.6084372240433993, 24.48358557860341733, -24.48358557860313311 ) ) ;
#12578 = CARTESIAN_POINT ( 'NONE',  ( -105.3755690713226869, 21.75974354311648540, -0.000000000000000000 ) ) ;
#12580 = CARTESIAN_POINT ( 'NONE',  ( -280.0000000000000000, -1.237140859393462838E-13, 20.00000000000001421 ) ) ;
#12579 = CARTESIAN_POINT ( 'NONE',  ( -259.2033419157646676, -6.730120644402966867, -49.83842185052038332 ) ) ;
#12581 = CARTESIAN_POINT ( 'NONE',  ( 130.8568914410475088, 4.207082182989012153, 52.36146031193425188 ) ) ;
#12582 = CIRCLE ( 'NONE', #1129, 14.99999999999999467 ) ;
#12583 = CARTESIAN_POINT ( 'NONE',  ( 19.44355705749545393, 43.94967286772826043, -18.20455056366577651 ) ) ;
#12584 = CARTESIAN_POINT ( 'NONE',  ( -86.96347745069644475, 18.24025645688351105, 2.449293598294708485E-15 ) ) ;
#12585 = CARTESIAN_POINT ( 'NONE',  ( -100.7734535825088500, -44.31723036834903695, 12.25131212657476709 ) ) ;
#12586 = CARTESIAN_POINT ( 'NONE',  ( -135.8532207217289738, -9.153146818113595984, 40.00000000000002132 ) ) ;
#12587 = CARTESIAN_POINT ( 'NONE',  ( -47.50817905880760605, -30.33575659740361274, 12.56548180749028987 ) ) ;
#12588 = CARTESIAN_POINT ( 'NONE',  ( 4.995406935893288214, 55.24977328853207581, 40.00000000000002132 ) ) ;
#12589 = AXIS2_PLACEMENT_3D ( 'NONE', #2362, #10476, #26331 ) ;
#12590 = EDGE_LOOP ( 'NONE', ( #11275, #948 ) ) ;
#12591 = CARTESIAN_POINT ( 'NONE',  ( 22.26816181513974158, 23.58015273002503420, -43.18156009806470763 ) ) ;
#12592 = CARTESIAN_POINT ( 'NONE',  ( -86.96347745069644475, -43.67073346367983788, 12.89780903124397149 ) ) ;
#12593 = DIRECTION ( 'NONE',  ( 0.000000000000000000, 0.000000000000000000, -1.000000000000000000 ) ) ;
#12594 = CARTESIAN_POINT ( 'NONE',  ( 6.202588567996412117, 24.77700748806132580, -44.80189419270392648 ) ) ;
#12595 = CARTESIAN_POINT ( 'NONE',  ( 199.0239263494850093, -19.93905678827826122, 1.642264957757122890 ) ) ;
#12596 = CIRCLE ( 'NONE', #17269, 19.53474504356807273 ) ;
#12597 = CARTESIAN_POINT ( 'NONE',  ( 151.7948205124836250, -23.49921654116371883, 23.49921654116317526 ) ) ;
#12598 = CARTESIAN_POINT ( 'NONE',  ( -86.86493150571114086, 7.943527260496203724, -19.77569912839170030 ) ) ;
#12599 = FILL_AREA_STYLE ('',( #16589 ) ) ;
#12600 = CARTESIAN_POINT ( 'NONE',  ( -188.2652746676664606, -13.82569223135940994, 46.97858116095157754 ) ) ;
#12601 = CARTESIAN_POINT ( 'NONE',  ( -86.96347745069644475, 15.38646221621772092, 15.38646221621800336 ) ) ;
#12602 = CARTESIAN_POINT ( 'NONE',  ( 57.59792236341147031, -1.722363176414363206, -54.84617931850881689 ) ) ;
#12603 = CARTESIAN_POINT ( 'NONE',  ( 169.9999999999999432, 22.62041470344884075, 9.369682556672378482 ) ) ;
#12605 = CARTESIAN_POINT ( 'NONE',  ( 91.82158438592158234, 44.40256751092319121, 12.16597498400105515 ) ) ;
#12604 = CARTESIAN_POINT ( 'NONE',  ( 190.0000000000001137, 30.00000000000007461, 0.000000000000000000 ) ) ;
#12606 = CARTESIAN_POINT ( 'NONE',  ( 0.2972598230769938343, 10.13633138497486286, -10.13633138497461594 ) ) ;
#12607 = CARTESIAN_POINT ( 'NONE',  ( 192.4448373802100889, -19.99999999996057198, -2.449293598294708485E-15 ) ) ;
#12608 = CARTESIAN_POINT ( 'NONE',  ( -105.3755690713226727, 18.24025645688350750, 2.449293598294708485E-15 ) ) ;
#12609 = CARTESIAN_POINT ( 'NONE',  ( -135.8532207217289738, -40.00000000000014211, 9.153146818113153671 ) ) ;
#12610 = CARTESIAN_POINT ( 'NONE',  ( -259.2033419157646676, -6.730120644403570829, -6.730120644403545960 ) ) ;
#12611 = AXIS2_PLACEMENT_3D ( 'NONE', #14272, #2180, #3635 ) ;
#12612 = CARTESIAN_POINT ( 'NONE',  ( -96.94449363889108895, 20.74048850978782710, -8.590991631004159856 ) ) ;
#12613 = CARTESIAN_POINT ( 'NONE',  ( 130.8568914410475088, 24.07718906446937623, -32.49135343045455215 ) ) ;
#12614 = CARTESIAN_POINT ( 'NONE',  ( -114.7823189589617812, -1.412059986362322217, 22.12960287296340667 ) ) ;
#12615 = VERTEX_POINT ( 'NONE', #1881 ) ;
#12616 = CARTESIAN_POINT ( 'NONE',  ( 4.995406935893297096, 10.78321810387837232, 67.35176059880234334 ) ) ;
#12617 = CARTESIAN_POINT ( 'NONE',  ( -86.86578273022415431, 8.153770686794796774, 19.68494377654078420 ) ) ;
#12618 = ITEM_DEFINED_TRANSFORMATION ( 'NONE', 'NONE', #19338,  #21058 ) ;
#12619 = CARTESIAN_POINT ( 'NONE',  ( 200.0000000000000000, 14.14213562373083022, 42.42640687119289566 ) ) ;
#12620 = CARTESIAN_POINT ( 'NONE',  ( -0.1993645192445167580, -44.04158448242537105, -18.24262160100613883 ) ) ;
#12621 = ORIENTED_EDGE ( 'NONE', *, *, #6054, .F. ) ;
#12622 = DIRECTION ( 'NONE',  ( -1.000000000000000000, 0.000000000000000000, 0.000000000000000000 ) ) ;
#12623 = CARTESIAN_POINT ( 'NONE',  ( -77.55640685889153474, -14.66973468135498493, -16.62872065403529476 ) ) ;
#12624 = ORIENTED_EDGE ( 'NONE', *, *, #22583, .F. ) ;
#12625 = CARTESIAN_POINT ( 'NONE',  ( 199.9999999999997726, 13.87428525677396607, -12.99608892921076198 ) ) ;
#12626 = FACE_OUTER_BOUND ( 'NONE', #18244, .T. ) ;
#12627 = CIRCLE ( 'NONE', #19367, 30.00000000000000355 ) ;
#12628 = CARTESIAN_POINT ( 'NONE',  ( -162.0762913951020892, 41.69427287682832173, 2.449293598294708485E-15 ) ) ;
#12629 = CARTESIAN_POINT ( 'NONE',  ( 151.7948205124836534, -51.78348778862529400, -4.785054706299085581 ) ) ;
#12630 = CARTESIAN_POINT ( 'NONE',  ( 199.0186810464772691, 9.993108295904475469, 17.32680936265314386 ) ) ;
#12631 = CARTESIAN_POINT ( 'NONE',  ( -213.1075012329537230, -66.26714140136188291, -9.698598906438677503 ) ) ;
#12632 = CARTESIAN_POINT ( 'NONE',  ( 0.2972598230770103767, -40.00000000000021316, 54.33493731733921805 ) ) ;
#12633 = CARTESIAN_POINT ( 'NONE',  ( -198.0356074513804572, 39.99999999999979394, 55.37879056874835726 ) ) ;
#12634 = DIRECTION ( 'NONE',  ( 0.7071067811865500152, 0.000000000000000000, -0.7071067811865451302 ) ) ;
#12635 = CARTESIAN_POINT ( 'NONE',  ( -238.4067589809705794, -0.9644942799826263791, -40.00000000000002132 ) ) ;
#12636 = CARTESIAN_POINT ( 'NONE',  ( -162.0762913951020892, -1.198031840385783919, 1.198031840385741731 ) ) ;
#12637 = CARTESIAN_POINT ( 'NONE',  ( 163.1118516004056573, -12.73709011382471878, -40.00000000000002132 ) ) ;
#12638 = CARTESIAN_POINT ( 'NONE',  ( -162.0762913951020892, -29.48230308784785692, 29.48230308784751230 ) ) ;
#12639 = B_SPLINE_CURVE_WITH_KNOTS ( 'NONE', 3,
 ( #5469, #1358, #17187, #25451, #6945, #21325 ),
 .UNSPECIFIED., .F., .F.,
 ( 4, 2, 4 ),
 ( 5.976737427190428336E-15, 0.03937685942888527468, 0.07875371885776458192 ),
 .UNSPECIFIED. ) ;
#12640 = CARTESIAN_POINT ( 'NONE',  ( 0.2972598230769957217, 1.502051041545559470E-13, -14.33493731733933352 ) ) ;
#12641 = EDGE_CURVE ( 'NONE', #17673, #12135, #9985, .T. ) ;
#12642 = CARTESIAN_POINT ( 'NONE',  ( -114.6821015619858315, 12.10555619829009899, -18.42370988051194658 ) ) ;
#12643 = CARTESIAN_POINT ( 'NONE',  ( -30.26275506840324425, 40.00000000000044764, -41.69427246844585255 ) ) ;
#12644 = CARTESIAN_POINT ( 'NONE',  ( 0.2972598230770103767, -40.00000000000021316, 54.33493731733921805 ) ) ;
#12645 = CARTESIAN_POINT ( 'NONE',  ( 57.59792236341147031, 26.56190807104693619, -30.00663442387692115 ) ) ;
#12646 = DIRECTION ( 'NONE',  ( 1.303213150798907793E-16, -1.000000000000000000, 0.000000000000000000 ) ) ;
#12647 = CARTESIAN_POINT ( 'NONE',  ( -114.7756899093965615, -16.59394837943032286, 14.65087933327505532 ) ) ;
#12648 = CARTESIAN_POINT ( 'NONE',  ( 136.1360204305621266, -3.511608612530379592, -53.05693388239318153 ) ) ;
#12649 = VERTEX_POINT ( 'NONE', #22633 ) ;
#12650 = CARTESIAN_POINT ( 'NONE',  ( -190.6721700386037810, 23.91541588165695842, -43.63442057298694721 ) ) ;
#12651 = DIRECTION ( 'NONE',  ( 0.000000000000000000, 0.000000000000000000, -1.000000000000000000 ) ) ;
#12652 = CARTESIAN_POINT ( 'NONE',  ( -105.3755690713226585, -18.24025645688353947, -40.00000000000002132 ) ) ;
#12653 = PLANE ( 'NONE',  #16150 ) ;
#12654 = CARTESIAN_POINT ( 'NONE',  ( 57.59792236341147031, -1.722363176415055985, 1.722363176415024677 ) ) ;
#12655 = VERTEX_POINT ( 'NONE', #18897 ) ;
#12656 = EDGE_LOOP ( 'NONE', ( #2990, #22978, #2115, #157 ) ) ;
#12657 = CARTESIAN_POINT ( 'NONE',  ( 199.9999999999999716, 0.6068915371250974689, 19.00166003603166587 ) ) ;
#12658 = DIRECTION ( 'NONE',  ( 1.000000000000000000, 1.836970198721030427E-16, -0.000000000000000000 ) ) ;
#12659 = CARTESIAN_POINT ( 'NONE',  ( 20.69615274311149378, 23.88537831998787908, 43.59383154590214815 ) ) ;
#12660 = ORIENTED_EDGE ( 'NONE', *, *, #17278, .F. ) ;
#12661 = VERTEX_POINT ( 'NONE', #676 ) ;
#12662 = CARTESIAN_POINT ( 'NONE',  ( 184.8905102610680444, -14.79361573936379415, -14.79361573936387941 ) ) ;
#12663 = CARTESIAN_POINT ( 'NONE',  ( 199.0183492910935286, -16.99256592298258184, -10.55490704374186883 ) ) ;
#12664 = CARTESIAN_POINT ( 'NONE',  ( -105.2333497863349550, 2.723647965520585856, 21.31134136414152991 ) ) ;
#12665 = CARTESIAN_POINT ( 'NONE',  ( 130.8568914410475088, -52.36146031193419503, 4.207082182989537955 ) ) ;
#12666 = CARTESIAN_POINT ( 'NONE',  ( -314.0000000000000568, -4.857225732735059864E-14, 20.53474504356812247 ) ) ;
#12667 = CARTESIAN_POINT ( 'NONE',  ( 91.82158438592156813, 40.00000000000009948, -17.20528682183286051 ) ) ;
#12668 = CARTESIAN_POINT ( 'NONE',  ( -210.0000000000000284, 8.572527594031471415E-15, 69.99999999999998579 ) ) ;
#12669 = FACE_OUTER_BOUND ( 'NONE', #18204, .T. ) ;
#12670 = CARTESIAN_POINT ( 'NONE',  ( 57.59792236341147031, 40.00000000000042633, -37.56421063658144277 ) ) ;
#12671 = CARTESIAN_POINT ( 'NONE',  ( -238.4067589809705794, 40.00000000000040501, -40.96449427990138759 ) ) ;
#12672 = CARTESIAN_POINT ( 'NONE',  ( -645.3052477932169495, 32.15456146116790848, 23.83018875450695617 ) ) ;
#12673 = CARTESIAN_POINT ( 'NONE',  ( -86.86493150571114086, -19.60045294882784717, -8.366608963953355627 ) ) ;
#12674 = CARTESIAN_POINT ( 'NONE',  ( 199.0062091525825849, 18.60380424647159003, -7.335505861489442836 ) ) ;
#12675 = CARTESIAN_POINT ( 'NONE',  ( -188.3508614409168445, 17.87647389380673246, 43.15762572182556767 ) ) ;
#12676 = CARTESIAN_POINT ( 'NONE',  ( 4.995406935893293543, -10.78321810388990265, -10.78321810389009272 ) ) ;
#12677 = CARTESIAN_POINT ( 'NONE',  ( -199.9999999999999716, -49.28189405767602693, 14.17215463606940595 ) ) ;
#12678 = CARTESIAN_POINT ( 'NONE',  ( -91.56559293963834989, 16.03295912088683650, 40.53558337403684675 ) ) ;
#12679 = DIRECTION ( 'NONE',  ( 1.836970198721030427E-16, -1.000000000000000000, 0.000000000000000000 ) ) ;
#12680 = CARTESIAN_POINT ( 'NONE',  ( -213.1075012329537230, -9.698598906462304825, -66.26714140138675191 ) ) ;
#12681 = CARTESIAN_POINT ( 'NONE',  ( -678.9461782662772293, 75.00000000000000000, 35.00000000000159162 ) ) ;
#12682 = CARTESIAN_POINT ( 'NONE',  ( 14.38125909742181285, -15.17850393972633505, 0.000000000000000000 ) ) ;
#12683 = CARTESIAN_POINT ( 'NONE',  ( -280.0000000000000568, 14.14213562373038968, 42.42640687119305198 ) ) ;
#12684 = CARTESIAN_POINT ( 'NONE',  ( 130.8568914410475372, 34.05028731879791337, 0.000000000000000000 ) ) ;
#12685 = CARTESIAN_POINT ( 'NONE',  ( -593.9199682435015575, 43.50753815682832482, 11.70952539979739804 ) ) ;
#12686 = ORIENTED_EDGE ( 'NONE', *, *, #17354, .F. ) ;
#12687 = CARTESIAN_POINT ( 'NONE',  ( 192.4448373802101173, -39.99999999999977973, -19.99999999996102673 ) ) ;
#12688 = CARTESIAN_POINT ( 'NONE',  ( 199.0123610602811652, -8.481086321338421996, -18.11865150390393708 ) ) ;
#12689 = CARTESIAN_POINT ( 'NONE',  ( 190.0000000000000000, 2.476104986517924766E-14, -82.49999999999998579 ) ) ;
#12690 = EDGE_LOOP ( 'NONE', ( #25181, #3990, #20917, #24205 ) ) ;
#12691 = ORIENTED_EDGE ( 'NONE', *, *, #6370, .T. ) ;
#12692 = VERTEX_POINT ( 'NONE', #20902 ) ;
#12693 = CARTESIAN_POINT ( 'NONE',  ( -208.1127848780265026, 55.00245453012668406, 2.449293598294708485E-15 ) ) ;
#12694 = B_SPLINE_CURVE_WITH_KNOTS ( 'NONE', 3,
 ( #11738, #12010, #7737, #19723, #22130, #17851 ),
 .UNSPECIFIED., .F., .F.,
 ( 4, 2, 4 ),
 ( -6.000000002804640696E-08, 0.04017169238941901283, 0.08034344477883806346 ),
 .UNSPECIFIED. ) ;
#12695 = AXIS2_PLACEMENT_3D ( 'NONE', #10449, #12569, #478 ) ;
#12696 = CARTESIAN_POINT ( 'NONE',  ( 146.6084372240433993, 3.800685668858732935, -3.800685668858610367 ) ) ;
#12697 = CARTESIAN_POINT ( 'NONE',  ( -114.7827252410749281, -22.13181612766661743, 0.6830184494021483976 ) ) ;
#12698 = CARTESIAN_POINT ( 'NONE',  ( 130.8568914410475372, -24.07718906447222551, -24.07718906447233209 ) ) ;
#12699 = CARTESIAN_POINT ( 'NONE',  ( -192.1131556193064682, 14.00853984552929354, -48.19965519933749931 ) ) ;
#12700 = CARTESIAN_POINT ( 'NONE',  ( 200.0000000000001990, 8.399020763088516972, -17.04381686846133803 ) ) ;
#12701 = CARTESIAN_POINT ( 'NONE',  ( 199.9999999999999432, 11.80293207093641961, -14.89258308846490664 ) ) ;
#12702 = CARTESIAN_POINT ( 'NONE',  ( -162.0762913951021176, -27.08623940707584055, -29.48230308784799547 ) ) ;
#12703 = CARTESIAN_POINT ( 'NONE',  ( 130.8568914410475088, -4.207082182990058428, 52.36146031193416661 ) ) ;
#12704 = CARTESIAN_POINT ( 'NONE',  ( -96.94835807405050332, 20.73599944956087882, 8.589132201369160668 ) ) ;
#12705 = CARTESIAN_POINT ( 'NONE',  ( -280.0000000000000568, 40.00000000000017764, -19.99999999999959144 ) ) ;
#12706 = CARTESIAN_POINT ( 'NONE',  ( -280.0000000000000000, 14.14213562373078581, 14.14213562373108424 ) ) ;
#12707 = CARTESIAN_POINT ( 'NONE',  ( 7.340276806054787606, 14.17250878947608861, 49.28408872342590286 ) ) ;
#12708 = CARTESIAN_POINT ( 'NONE',  ( 19.06497207195980792, 10.03556273973433299, 10.03556273973436319 ) ) ;
#12709 = CARTESIAN_POINT ( 'NONE',  ( 136.1360204305621551, -31.79587985999244282, -24.77266263493140386 ) ) ;
#12710 = CARTESIAN_POINT ( 'NONE',  ( -208.1127848780265026, -15.00245453012673202, 0.000000000000000000 ) ) ;
#12712 = CARTESIAN_POINT ( 'NONE',  ( 19.06497207195980792, 39.99999999999983658, 54.19242893257857929 ) ) ;
#12711 = CARTESIAN_POINT ( 'NONE',  ( 184.8905102610680444, -43.07788698682556827, -13.49065550809859104 ) ) ;
#12713 = CARTESIAN_POINT ( 'NONE',  ( 37.15749683989281493, 41.79699086507442019, -12.76981037570198296 ) ) ;
#12714 = CARTESIAN_POINT ( 'NONE',  ( -198.0356074513804572, 15.37879056873067007, 0.000000000000000000 ) ) ;
#12715 = CARTESIAN_POINT ( 'NONE',  ( 151.7948205124836534, -51.78348778862535795, 4.785054706298367044 ) ) ;
#12716 = CARTESIAN_POINT ( 'NONE',  ( 19.06497207195980792, 54.19242893257844429, 40.00000000000002132 ) ) ;
#12717 = AXIS2_PLACEMENT_3D ( 'NONE', #1604, #3588, #25957 ) ;
#12718 = B_SPLINE_CURVE_WITH_KNOTS ( 'NONE', 3,
 ( #12572, #611, #6582, #19226, #10580, #23227, #4873, #1006, #14830, #2746, #18969, #17219 ),
 .UNSPECIFIED., .F., .F.,
 ( 4, 2, 2, 2, 2, 4 ),
 ( 9.771591248311271618E-17, 0.004680202113613741305, 0.009360404227227383731, 0.01170050528403420408, 0.01404060634084102616, 0.01872080845445462868 ),
 .UNSPECIFIED. ) ;
#12719 = EDGE_CURVE ( 'NONE', #12515, #9554, #4132, .T. ) ;
#12720 = CARTESIAN_POINT ( 'NONE',  ( -7.769366557096847536, -45.69637362127787839, 13.56374645827445136 ) ) ;
#12721 = CARTESIAN_POINT ( 'NONE',  ( 192.4448373802101173, -20.00000000003938538, 40.00000000000002132 ) ) ;
#12722 = EDGE_CURVE ( 'NONE', #14871, #20514, #10245, .T. ) ;
#12723 = ORIENTED_EDGE ( 'NONE', *, *, #10770, .T. ) ;
#12724 = CARTESIAN_POINT ( 'NONE',  ( 73.43374752932638216, -12.96823637283634234, -26.88866000080070862 ) ) ;
#12725 = B_SPLINE_CURVE_WITH_KNOTS ( 'NONE', 3,
 ( #13613, #23994, #3386, #11889, #5386, #9250, #19739, #13491, #21485, #9766, #21871, #9371, #5260, #1527, #17867, #19875 ),
 .UNSPECIFIED., .F., .F.,
 ( 4, 2, 2, 2, 2, 2, 2, 4 ),
 ( 0.0003132551814621161888, 0.004563509514629761864, 0.006688636681213585081, 0.007751200264505497123, 0.008813763847797409165, 0.01306401818096505907, 0.01518914534754888489, 0.01731427251413270724 ),
 .UNSPECIFIED. ) ;
#12726 = CARTESIAN_POINT ( 'NONE',  ( -30.26275506840324070, -27.08623969584595770, 29.48230279907789608 ) ) ;
#12727 = CARTESIAN_POINT ( 'NONE',  ( -3.564770973659789455, -17.92368662243711697, 43.27160733161164075 ) ) ;
#12728 = EDGE_CURVE ( 'NONE', #2983, #18109, #19157, .T. ) ;
#12729 = EDGE_CURVE ( 'NONE', #495, #18845, #811, .T. ) ;
#12730 = CARTESIAN_POINT ( 'NONE',  ( -0.6848998192584003775, 13.98809697771244309, -48.06291537635669897 ) ) ;
#12731 = CARTESIAN_POINT ( 'NONE',  ( 199.0244488197511998, -19.74721217248383809, 3.261676333419620821 ) ) ;
#12732 = CARTESIAN_POINT ( 'NONE',  ( -56.48582580120559982, 21.81201906317729922, 34.75652343174635917 ) ) ;
#12733 = LINE ( 'NONE', #8610, #18754 ) ;
#12734 = CARTESIAN_POINT ( 'NONE',  ( -87.13361725327075646, 0.6860286134974562522, 21.49321519333430786 ) ) ;
#12735 = CARTESIAN_POINT ( 'NONE',  ( -188.3120606736142406, -13.82878088495403546, 46.99497558484350179 ) ) ;
#12736 = CARTESIAN_POINT ( 'NONE',  ( -30.26275506840324070, -1.198031551616016266, -1.198031551616031587 ) ) ;
#12737 = CIRCLE ( 'NONE', #5100, 5.000000000000095035 ) ;
#12738 = CARTESIAN_POINT ( 'NONE',  ( -30.26275506840324070, -27.08623969584554558, -29.48230279907826912 ) ) ;
#12739 = CARTESIAN_POINT ( 'NONE',  ( 57.59792236341147031, 1.722363176415040886, 1.722363176415060426 ) ) ;
#12741 = CARTESIAN_POINT ( 'NONE',  ( -280.0000000000000568, -14.14213562373049449, -42.42640687119305198 ) ) ;
#12740 = CARTESIAN_POINT ( 'NONE',  ( -280.0000000000000568, 42.42640687119294540, -14.14213562373059041 ) ) ;
#12742 = CARTESIAN_POINT ( 'NONE',  ( -135.8532207217289738, 21.81201906317729566, 34.75652343174635917 ) ) ;
#12743 = CARTESIAN_POINT ( 'NONE',  ( -259.2033419157646676, -30.48217210827744950, 40.00000000000002132 ) ) ;
#12744 = CARTESIAN_POINT ( 'NONE',  ( -30.26275506840324425, 1.694272468446254232, -40.00000000000002132 ) ) ;
#12745 = CARTESIAN_POINT ( 'NONE',  ( 130.8568914410475088, -40.00000000000036238, 34.05028731879746573 ) ) ;
#12746 = CARTESIAN_POINT ( 'NONE',  ( 14.38125909742180752, 10.73282306404720465, 10.73282306404724018 ) ) ;
#12747 = CARTESIAN_POINT ( 'NONE',  ( -89.91646883266047041, 20.29783361045703316, -8.407637967992551253 ) ) ;
#12748 = PRODUCT ( 'Bolt', 'Bolt', '', ( #26078 ) ) ;
#12749 = CARTESIAN_POINT ( 'NONE',  ( 151.7948205124836250, -4.785054706301600902, -4.785054706301715477 ) ) ;
#12750 = CARTESIAN_POINT ( 'NONE',  ( -188.2652133075157224, 46.97855991888798854, -13.82568790539414572 ) ) ;
#12751 = ORIENTED_EDGE ( 'NONE', *, *, #4541, .T. ) ;
#12752 = CARTESIAN_POINT ( 'NONE',  ( 151.7948205124836534, -23.49921654116027980, 33.06932595376354556 ) ) ;
#12753 = CARTESIAN_POINT ( 'NONE',  ( 200.0000000000000000, 52.49999999999987210, 82.49999999999998579 ) ) ;
#12754 = CARTESIAN_POINT ( 'NONE',  ( -238.4067589809705794, -28.96627169325343942, 28.96627169325309126 ) ) ;
#12755 = CARTESIAN_POINT ( 'NONE',  ( -3.473570583883275109, -43.29615835920788669, -17.93385599103721972 ) ) ;
#12756 = EDGE_LOOP ( 'NONE', ( #6435, #3326, #2557, #5642, #22848, #8497, #16119, #18500 ) ) ;
#12757 = CARTESIAN_POINT ( 'NONE',  ( 170.2234770963711128, -24.55285855007183926, 0.000000000000000000 ) ) ;
#12758 = CARTESIAN_POINT ( 'NONE',  ( -110.0368417077420844, -7.992411109433259497, -18.51665893310629940 ) ) ;
#12759 = CIRCLE ( 'NONE', #3008, 30.00000000000000000 ) ;
#12760 = CARTESIAN_POINT ( 'NONE',  ( 199.9999999999995168, 19.00182775553472325, -0.6082061139381043091 ) ) ;
#12761 = CARTESIAN_POINT ( 'NONE',  ( 23.37394308801977161, 13.80096434448334186, -46.80823611210181667 ) ) ;
#12762 = CARTESIAN_POINT ( 'NONE',  ( -56.48582580120559271, 30.84685318188643066, 2.449293598294708485E-15 ) ) ;
#12763 = CARTESIAN_POINT ( 'NONE',  ( 57.59792236341147031, -1.722363176415055985, 1.722363176415024677 ) ) ;
#12764 = CARTESIAN_POINT ( 'NONE',  ( 199.0140795438509826, 16.43701665320993044, 11.39707250661459348 ) ) ;
#12765 = CARTESIAN_POINT ( 'NONE',  ( 91.82158438592159655, -44.40256751092341858, 12.16597498400012434 ) ) ;
#12766 = CARTESIAN_POINT ( 'NONE',  ( 192.4448373802101173, -40.00000000000005684, 19.99999999996046185 ) ) ;
#12767 = CARTESIAN_POINT ( 'NONE',  ( 163.1118516004056573, 40.00000000000014921, -27.26290988616858968 ) ) ;
#12768 = CARTESIAN_POINT ( 'NONE',  ( -1.818469002956051073, 47.72215409237468720, -13.93708913181252562 ) ) ;
#12769 = CARTESIAN_POINT ( 'NONE',  ( -105.3755690713226727, -18.24025645688354302, -2.449293598294708485E-15 ) ) ;
#12771 = CARTESIAN_POINT ( 'NONE',  ( -598.7225062214002946, 38.71349023310503412, 10.07489800994831697 ) ) ;
#12770 = CARTESIAN_POINT ( 'NONE',  ( 22.17571259161183050, -23.59965736305000661, -43.20787961119341247 ) ) ;
#12772 = CARTESIAN_POINT ( 'NONE',  ( -192.9588430854690273, -54.46834944101725284, -40.00000000000002132 ) ) ;
#12773 = CARTESIAN_POINT ( 'NONE',  ( 4.995406935893305977, -39.06748935135212264, 39.06748935135171763 ) ) ;
#12774 = AXIS2_PLACEMENT_3D ( 'NONE', #7324, #5597, #25322 ) ;
#12775 = CARTESIAN_POINT ( 'NONE',  ( -110.0723150831391450, 10.27950330712184623, -17.37189535805912044 ) ) ;
#12776 = CARTESIAN_POINT ( 'NONE',  ( 192.4448373802101173, 39.99999999999985079, 20.00000000003984013 ) ) ;
#12777 = CARTESIAN_POINT ( 'NONE',  ( -56.48582580120559982, 39.99999999999990763, 30.84685318188658698 ) ) ;
#12778 = CARTESIAN_POINT ( 'NONE',  ( 4.995406935893289102, 10.78321810388998081, 10.78321810389001811 ) ) ;
#12779 = CARTESIAN_POINT ( 'NONE',  ( -83.21262154144254453, -13.72187187061479818, 33.12752917118424989 ) ) ;
#12780 = CARTESIAN_POINT ( 'NONE',  ( -238.4067589809705794, 0.6820004457912851592, -0.6820004457913123597 ) ) ;
#12781 = CARTESIAN_POINT ( 'NONE',  ( -135.8532207217289738, -21.81201906317788186, 21.81201906317762962 ) ) ;
#12782 = ORIENTED_EDGE ( 'NONE', *, *, #23866, .T. ) ;
#12784 = CARTESIAN_POINT ( 'NONE',  ( -40.07203023075403792, 34.25109662815976463, -11.15662918589591079 ) ) ;
#12783 = CARTESIAN_POINT ( 'NONE',  ( 184.8905102610680444, 14.79361573936375507, 14.79361573936398067 ) ) ;
#12785 = CARTESIAN_POINT ( 'NONE',  ( 151.0853911467766864, 29.06993079631229904, -12.04115959307975992 ) ) ;
#12786 = CARTESIAN_POINT ( 'NONE',  ( -30.26275506840323004, -41.69427246844627888, -40.00000000000002132 ) ) ;
#12787 = CARTESIAN_POINT ( 'NONE',  ( -87.04503123322949421, -4.710636111839787254, -20.91882565556209883 ) ) ;
#12788 = FACE_BOUND ( 'NONE', #15795, .T. ) ;
#12789 = SHAPE_REPRESENTATION_RELATIONSHIP ( 'NONE' , 'NONE' ,  #126, #11192 ) ;
#12790 = ORIENTED_EDGE ( 'NONE', *, *, #16780, .F. ) ;
#12791 = ORIENTED_EDGE ( 'NONE', *, *, #19079, .T. ) ;
#12792 = CARTESIAN_POINT ( 'NONE',  ( -102.4068193528149777, 8.735227608997227833, -20.17396017424876220 ) ) ;
#12793 = CARTESIAN_POINT ( 'NONE',  ( -94.58414068585072698, 8.590713000660940679, -20.73981583682874685 ) ) ;
#12794 = CARTESIAN_POINT ( 'NONE',  ( 23.40652632867847061, 23.33303889678602516, 42.84715492600980014 ) ) ;
#12795 = VERTEX_POINT ( 'NONE', #20630 ) ;
#12796 = ORIENTED_EDGE ( 'NONE', *, *, #2341, .T. ) ;
#12797 = CARTESIAN_POINT ( 'NONE',  ( 200.0000000000000000, -42.42640687119293119, 14.14213562373082134 ) ) ;
#12798 = CARTESIAN_POINT ( 'NONE',  ( 199.0239263494850093, -19.93905678827826122, 1.642264957757122890 ) ) ;
#12799 = VECTOR ( 'NONE', #3455, 1000.000000000000000 ) ;
#12800 = CARTESIAN_POINT ( 'NONE',  ( -105.3239292022199152, -5.381957438726850285, 20.72686647364727364 ) ) ;
#12801 = CARTESIAN_POINT ( 'NONE',  ( 151.7948205124836534, -23.49921654116027980, 33.06932595376354556 ) ) ;
#12802 = VECTOR ( 'NONE', #12862, 1000.000000000000000 ) ;
#12803 = CIRCLE ( 'NONE', #8983, 5.000000000000004441 ) ;
#12804 = B_SPLINE_CURVE_WITH_KNOTS ( 'NONE', 3,
 ( #24788, #14650, #22789, #14918, #4830, #12935 ),
 .UNSPECIFIED., .F., .F.,
 ( 4, 2, 4 ),
 ( 0.000000000000000000, 0.004090268262613940345, 0.008180536525227880690 ),
 .UNSPECIFIED. ) ;
#12805 = DIRECTION ( 'NONE',  ( -1.000000000000000000, -0.000000000000000000, -0.000000000000000000 ) ) ;
#12806 = CARTESIAN_POINT ( 'NONE',  ( -30.26275506840325136, 40.00000000000001421, 1.694272468446399227 ) ) ;
#12807 = ADVANCED_FACE ( 'NONE', ( #14627 ), #15207, .T. ) ;
#12808 = CARTESIAN_POINT ( 'NONE',  ( -200.0000000000000000, -20.90527768611929815, 45.34857661735442491 ) ) ;
#12809 = DIRECTION ( 'NONE',  ( -1.000000000000000000, -0.000000000000000000, -0.000000000000000000 ) ) ;
#12810 = CARTESIAN_POINT ( 'NONE',  ( -192.9588430854689989, 5.375290060580374156E-13, -54.46834944099972375 ) ) ;
#12811 = CARTESIAN_POINT ( 'NONE',  ( -213.1075012329537230, 1.045191102001431893E-13, -13.71589010951911902 ) ) ;
#12812 = CARTESIAN_POINT ( 'NONE',  ( -648.4308094340339039, 34.05684324981173461, 20.98299627712672688 ) ) ;
#12813 = DIRECTION ( 'NONE',  ( 0.000000000000000000, -1.000000000000000000, 0.000000000000000000 ) ) ;
#12814 = CARTESIAN_POINT ( 'NONE',  ( 199.0079837170424923, 19.96494570524563272, -1.290871210190707608 ) ) ;
#12815 = CARTESIAN_POINT ( 'NONE',  ( -189.1288337602853460, 23.62383291543111241, 43.24060467048551715 ) ) ;
#12816 = CARTESIAN_POINT ( 'NONE',  ( -259.2033419157646676, -21.55415060305872998, 35.01439189186525880 ) ) ;
#12817 = DIRECTION ( 'NONE',  ( 0.01051738792037606486, 0.3656191332807844363, 0.9307051272719736312 ) ) ;
#12818 = CARTESIAN_POINT ( 'NONE',  ( -192.9588430854690273, -10.23066800229550388, 66.79921049721887982 ) ) ;
#12819 = FACE_OUTER_BOUND ( 'NONE', #5835, .T. ) ;
#12820 = AXIS2_PLACEMENT_3D ( 'NONE', #10397, #25049, #696 ) ;
#12821 = CARTESIAN_POINT ( 'NONE',  ( 57.59792236341148453, 1.722363176415528940, -54.84617931850878136 ) ) ;
#12822 = CARTESIAN_POINT ( 'NONE',  ( -660.1500850185274203, 43.58821494200376634, 11.19816822568961712 ) ) ;
#12823 = CARTESIAN_POINT ( 'NONE',  ( -83.21262154144251610, -13.72187187061454949, -33.12752917118435647 ) ) ;
#12824 = ADVANCED_FACE ( 'NONE', ( #21291 ), #11167, .F. ) ;
#12825 = CARTESIAN_POINT ( 'NONE',  ( -238.4067589809705794, 28.96627169325285678, 27.60227080167094726 ) ) ;
#12826 = CIRCLE ( 'NONE', #1343, 29.99999999999999289 ) ;
#12827 = CARTESIAN_POINT ( 'NONE',  ( 130.8568914410475088, -5.949712681206671405, 40.00000000000002132 ) ) ;
#12828 = CARTESIAN_POINT ( 'NONE',  ( -617.0448027493109748, 29.97558630572889271, -33.56382543646817851 ) ) ;
#12829 = VERTEX_POINT ( 'NONE', #6160 ) ;
#12830 = CARTESIAN_POINT ( 'NONE',  ( 170.2234770963711128, 1.955190573858485757E-13, -15.44714144992816074 ) ) ;
#12831 = CARTESIAN_POINT ( 'NONE',  ( -612.0709805440841365, -1.322736627157445917E-16, 0.000000000000000000 ) ) ;
#12832 = DIRECTION ( 'NONE',  ( 1.303213150798907793E-16, -1.000000000000000000, 0.000000000000000000 ) ) ;
#12833 = ORIENTED_EDGE ( 'NONE', *, *, #21024, .F. ) ;
#12834 = ORIENTED_EDGE ( 'NONE', *, *, #6452, .F. ) ;
#12835 = CARTESIAN_POINT ( 'NONE',  ( -238.4067589809705794, 40.96449427998256709, 2.449293598294708485E-15 ) ) ;
#12836 = FILL_AREA_STYLE ('',( #9232 ) ) ;
#12837 = EDGE_CURVE ( 'NONE', #15543, #18643, #14058, .T. ) ;
#12838 = AXIS2_PLACEMENT_3D ( 'NONE', #25311, #7069, #20655 ) ;
#12839 = CARTESIAN_POINT ( 'NONE',  ( -110.0471271034679575, -18.98461286763408040, -6.849398635789994749 ) ) ;
#12840 = PRODUCT ( 'MAS-348', 'MAS-348', '', ( #7060 ) ) ;
#12841 = CARTESIAN_POINT ( 'NONE',  ( -77.59212294118390219, -13.55867551895970635, 17.46520578609403174 ) ) ;
#12842 = CARTESIAN_POINT ( 'NONE',  ( 136.1360204305621551, -39.99999999999987921, -35.03383547441310242 ) ) ;
#12843 = CARTESIAN_POINT ( 'NONE',  ( 199.9999999999998295, 8.257913856993376100, -17.11264870637372226 ) ) ;
#12844 = CARTESIAN_POINT ( 'NONE',  ( 199.9999999999999147, -6.992664781673325614, -17.67258180576657267 ) ) ;
#12845 = CARTESIAN_POINT ( 'NONE',  ( 200.0000000000000000, -42.42640687119272513, -14.14213562373140753 ) ) ;
#12846 = CARTESIAN_POINT ( 'NONE',  ( -105.3755690713226727, 15.38646221621771737, 15.38646221621800514 ) ) ;
#12847 = CARTESIAN_POINT ( 'NONE',  ( -103.9707779739353839, 20.03121292026044387, 8.297200062355283734 ) ) ;
#12848 = CARTESIAN_POINT ( 'NONE',  ( -198.0356074513804572, 40.00000000000056843, -55.37879056871282302 ) ) ;
#12849 = CARTESIAN_POINT ( 'NONE',  ( -259.2033419157646676, 6.730120644403426944, 6.730120644403592145 ) ) ;
#12850 = CARTESIAN_POINT ( 'NONE',  ( -192.9588430854689989, 38.51493924976929861, 38.51493924976947625 ) ) ;
#12851 = CARTESIAN_POINT ( 'NONE',  ( 192.4448373802100889, -14.14213562370313682, 14.14213562370301958 ) ) ;
#12852 = CARTESIAN_POINT ( 'NONE',  ( 199.0084596282743803, 19.99626877350650744, -0.0005331044653283251991 ) ) ;
#12854 = CARTESIAN_POINT ( 'NONE',  ( 170.2234770963711128, 1.169953928977015745E-13, -24.55285855007187124 ) ) ;
#12853 = CARTESIAN_POINT ( 'NONE',  ( 151.7948205124836534, -23.49921654115981084, -33.06932595376387951 ) ) ;
#12855 = CARTESIAN_POINT ( 'NONE',  ( -30.26275506840324070, 1.694272468446254232, 0.000000000000000000 ) ) ;
#12856 = CARTESIAN_POINT ( 'NONE',  ( 163.1118516004056573, -19.27778845538761132, -19.27778845538770724 ) ) ;
#12857 = CARTESIAN_POINT ( 'NONE',  ( 151.7948205124836534, -33.23291073765550863, 40.00000000000002132 ) ) ;
#12858 = EDGE_LOOP ( 'NONE', ( #14220, #22124 ) ) ;
#12859 = CARTESIAN_POINT ( 'NONE',  ( 11.38508063386201385, -49.30460303387604881, 14.17561098849807166 ) ) ;
#12860 = CARTESIAN_POINT ( 'NONE',  ( 0.2972598230769930017, 54.33493731733936016, 40.00000000000002132 ) ) ;
#12861 = VERTEX_POINT ( 'NONE', #14270 ) ;
#12862 = DIRECTION ( 'NONE',  ( 1.000000000000000000, 1.836970198721030181E-16, 0.000000000000000000 ) ) ;
#12863 = CARTESIAN_POINT ( 'NONE',  ( 0.2972598230769938343, 10.13633138497472252, 10.13633138497475628 ) ) ;
#12864 = CARTESIAN_POINT ( 'NONE',  ( -47.30403195827515361, -12.59259458036005164, 30.40121262124529267 ) ) ;
#12865 = CARTESIAN_POINT ( 'NONE',  ( -213.1075012329537230, 9.698598906450410340, 9.698598906450483170 ) ) ;
#12866 = CARTESIAN_POINT ( 'NONE',  ( -4.031723327955597291, 23.45082932595568437, -43.00750292060828173 ) ) ;
#12867 = CARTESIAN_POINT ( 'NONE',  ( 199.0261122283987731, -17.00127104892409591, 10.56324628376440877 ) ) ;
#12868 = CARTESIAN_POINT ( 'NONE',  ( -30.26275506840325136, 29.48230279907760121, 27.08623969584625613 ) ) ;
#12869 = CARTESIAN_POINT ( 'NONE',  ( -82.25136756411366434, -19.89060514489998610, 3.474794711464142427 ) ) ;
#12870 = CARTESIAN_POINT ( 'NONE',  ( -575.0231298121445889, 75.00000000000000000, 29.99999999999825206 ) ) ;
#12871 = CARTESIAN_POINT ( 'NONE',  ( -194.4222169614207303, -24.44978956118232460, 44.35789444896035860 ) ) ;
#12872 = CARTESIAN_POINT ( 'NONE',  ( 170.2234770963711128, -2.259079968736224833E-13, 24.55285855007187124 ) ) ;
#12873 = EDGE_CURVE ( 'NONE', #12388, #162, #17118, .T. ) ;
#12874 = CARTESIAN_POINT ( 'NONE',  ( 19.06497207195980792, 18.24870850772737185, 38.31983398719634692 ) ) ;
#12875 = CARTESIAN_POINT ( 'NONE',  ( 192.4448373802101173, -14.14213562375826605, -42.42640687116518450 ) ) ;
#12876 = CARTESIAN_POINT ( 'NONE',  ( -162.0762913951020892, -1.198031840385767266, -1.198031840385758384 ) ) ;
#12878 = CARTESIAN_POINT ( 'NONE',  ( -192.9588430854689989, 38.51493924976983152, -38.51493924976893624 ) ) ;
#12877 = CARTESIAN_POINT ( 'NONE',  ( -162.0762913951020892, -1.198031840385767266, -1.198031840385758384 ) ) ;
#12879 = CARTESIAN_POINT ( 'NONE',  ( -162.0762913951021176, 57.76657433523994456, -1.198031840315424867 ) ) ;
#12880 = CARTESIAN_POINT ( 'NONE',  ( 130.8568914410475088, 34.05028731879790627, 40.00000000000002132 ) ) ;
#12881 = CARTESIAN_POINT ( 'NONE',  ( 200.0000000000000000, 19.99999999999996447, -40.00000000000002132 ) ) ;
#12882 = CARTESIAN_POINT ( 'NONE',  ( -259.2033419157646676, 21.55415060305839958, -35.01439189186541512 ) ) ;
#12883 = CARTESIAN_POINT ( 'NONE',  ( -259.2033419157646676, -1.438356298054549103E-14, -9.517827891722632216 ) ) ;
#12884 = CARTESIAN_POINT ( 'NONE',  ( 91.82158438592159655, -44.40256751092341858, 12.16597498400012434 ) ) ;
#12885 = ADVANCED_FACE ( 'NONE', ( #1780 ), #10411, .T. ) ;
#12886 = CARTESIAN_POINT ( 'NONE',  ( -129.2303492456006211, 25.82246949204678899, -9.309000511913200882 ) ) ;
#12887 = EDGE_LOOP ( 'NONE', ( #8841, #22397, #16381, #20343, #7561, #16282, #14475 ) ) ;
#12888 = CARTESIAN_POINT ( 'NONE',  ( 57.59792236341147031, -1.722363176415123043, 54.84617931850879557 ) ) ;
#12889 = CARTESIAN_POINT ( 'NONE',  ( -198.0012401002533124, 24.77357857137259600, 44.79720214428343894 ) ) ;
#12890 = ITEM_DEFINED_TRANSFORMATION ( 'NONE', 'NONE', #24013,  #21058 ) ;
#12891 = CARTESIAN_POINT ( 'NONE',  ( -213.1075012329537230, -9.698598906438496314, 66.26714140136188291 ) ) ;
#12892 = CARTESIAN_POINT ( 'NONE',  ( 20.91285618071585617, -47.65039156503396356, -13.92631245146007757 ) ) ;
#12893 = VERTEX_POINT ( 'NONE', #18257 ) ;
#12894 = CARTESIAN_POINT ( 'NONE',  ( -100.0753760173596874, -20.72827493166422030, 8.149786832858520569 ) ) ;
#12895 = CARTESIAN_POINT ( 'NONE',  ( -105.2054292633754784, -14.23662800545034024, -16.15936842200748202 ) ) ;
#12896 = CARTESIAN_POINT ( 'NONE',  ( 199.9999999999997442, 18.75350838795884201, -3.072479883316599381 ) ) ;
#12897 = DIRECTION ( 'NONE',  ( 0.000000000000000000, 0.000000000000000000, 1.000000000000000000 ) ) ;
#12898 = CARTESIAN_POINT ( 'NONE',  ( -213.1075012329537230, 53.71589010951910836, 2.449293598294708485E-15 ) ) ;
#12899 = CARTESIAN_POINT ( 'NONE',  ( -198.0356074513804572, 10.87444709759730088, -10.87444709759707173 ) ) ;
#12900 = CARTESIAN_POINT ( 'NONE',  ( 199.0137418305357073, 16.79925839223816197, 10.85573510210755899 ) ) ;
#12901 = CARTESIAN_POINT ( 'NONE',  ( -208.1127848780264742, -38.89260858015753541, 17.67593391476614784 ) ) ;
#12902 = CARTESIAN_POINT ( 'NONE',  ( -192.9588430854689989, -2.280704836619014309E-13, 54.46834944099972375 ) ) ;
#12903 = CARTESIAN_POINT ( 'NONE',  ( 199.9999999999999432, -3.553951640073651008E-14, 19.99999999999992539 ) ) ;
#12904 = PRODUCT_RELATED_PRODUCT_CATEGORY ( 'part', '', ( #195 ) ) ;
#12905 = DIRECTION ( 'NONE',  ( 1.000000000000000000, 0.000000000000000000, -0.000000000000000000 ) ) ;
#12906 = CARTESIAN_POINT ( 'NONE',  ( 19.06497207195982924, -54.19242893257843008, -2.449293598294708485E-15 ) ) ;
#12908 = CARTESIAN_POINT ( 'NONE',  ( -100.7734535825088500, 16.03295912088713848, -16.03295912088698927 ) ) ;
#12907 = CARTESIAN_POINT ( 'NONE',  ( 22.72189371636524768, -13.83659596078988052, -47.04833883278732998 ) ) ;
#12909 = CARTESIAN_POINT ( 'NONE',  ( -280.0000000000000568, -20.00000000000007105, 40.00000000000002132 ) ) ;
#12910 = CARTESIAN_POINT ( 'NONE',  ( 136.1360204305621266, 53.05693388239316022, 3.511608612530967566 ) ) ;
#12911 = CARTESIAN_POINT ( 'NONE',  ( -188.2995950289364373, 13.82811170417132196, 46.99046209955516673 ) ) ;
#12912 = CARTESIAN_POINT ( 'NONE',  ( -114.6375327213591362, 18.99176668988436134, -11.19832436704016487 ) ) ;
#12913 = CARTESIAN_POINT ( 'NONE',  ( -30.26275506840323359, 4.336144384597734078E-13, -41.69427246844629309 ) ) ;
#12914 = CARTESIAN_POINT ( 'NONE',  ( 136.1360204305621266, -24.77266263493116583, -24.77266263493127951 ) ) ;
#12915 = DIRECTION ( 'NONE',  ( 0.3301743741187893599, 0.000000000000000000, -0.9439199556505125654 ) ) ;
#12916 = CARTESIAN_POINT ( 'NONE',  ( -114.6679276626374815, -11.81543316368266616, 18.60595090113752548 ) ) ;
#12917 = CARTESIAN_POINT ( 'NONE',  ( -105.3755690713226585, 15.38646221621762678, 41.18208027870604582 ) ) ;
#12918 = ADVANCED_FACE ( 'NONE', ( #24531 ), #3770, .T. ) ;
#12919 = ORIENTED_EDGE ( 'NONE', *, *, #1862, .T. ) ;
#12921 = CARTESIAN_POINT ( 'NONE',  ( -192.1167141818822586, 24.15421809699839528, -43.95739236919479964 ) ) ;
#12920 = CARTESIAN_POINT ( 'NONE',  ( -77.70077460412264259, 5.497879648892802784, -21.35157292214961799 ) ) ;
#12922 = DIRECTION ( 'NONE',  ( 0.2259624730556991923, 0.9741360073267758546, 0.000000000000000000 ) ) ;
#12923 = CARTESIAN_POINT ( 'NONE',  ( -56.48582580120557850, -30.84685318188645198, -2.449293598294708485E-15 ) ) ;
#12924 = CARTESIAN_POINT ( 'NONE',  ( 170.0000000000000284, -12.70659020859091015, -21.59613885783092257 ) ) ;
#12925 = CARTESIAN_POINT ( 'NONE',  ( -195.1686598214593573, 44.46432177479810832, -24.52826087131574440 ) ) ;
#12926 = CARTESIAN_POINT ( 'NONE',  ( 0.000000000000000000, 0.000000000000000000, 0.000000000000000000 ) ) ;
#12927 = EDGE_LOOP ( 'NONE', ( #15609, #26252, #25303, #20482 ) ) ;
#12928 = ORIENTED_EDGE ( 'NONE', *, *, #8162, .F. ) ;
#12929 = CARTESIAN_POINT ( 'NONE',  ( 199.9999999999999716, 3.854709303011653709, 18.61380101728145320 ) ) ;
#12930 = CARTESIAN_POINT ( 'NONE',  ( -100.0968563617633720, 8.893120081483285588, -20.41799937591630965 ) ) ;
#12931 = ORIENTED_EDGE ( 'NONE', *, *, #19384, .T. ) ;
#12932 = VERTEX_POINT ( 'NONE', #20531 ) ;
#12933 = CARTESIAN_POINT ( 'NONE',  ( -162.0762913951021176, -27.08623940707624911, 29.48230308784761888 ) ) ;
#12934 = CARTESIAN_POINT ( 'NONE',  ( 199.0247296274817188, -19.55681251529712128, 4.220088366773818045 ) ) ;
#12935 = CARTESIAN_POINT ( 'NONE',  ( -105.4741150117379789, -19.60045294982730724, -8.366608964594114184 ) ) ;
#12936 =( REPRESENTATION_RELATIONSHIP ('NONE','NONE', #23888, #9131 ) REPRESENTATION_RELATIONSHIP_WITH_TRANSFORMATION ( #8493 )SHAPE_REPRESENTATION_RELATIONSHIP( ) );
#12937 = CARTESIAN_POINT ( 'NONE',  ( -30.26275506840324070, -27.08623969584595770, 29.48230279907789608 ) ) ;
#12938 = CARTESIAN_POINT ( 'NONE',  ( -105.2054292635177006, 21.49321519473978981, 1.401583908954727953 ) ) ;
#12939 = CARTESIAN_POINT ( 'NONE',  ( 192.4448373802100889, -3.692737725850373501E-14, 19.99999999996060751 ) ) ;
#12940 = DIRECTION ( 'NONE',  ( 1.000000000000000000, 1.836970198721030427E-16, -0.000000000000000000 ) ) ;
#12941 = CARTESIAN_POINT ( 'NONE',  ( -266.9101291198153376, 0.000000000000000000, 0.000000000000000000 ) ) ;
#12942 = CARTESIAN_POINT ( 'NONE',  ( -162.0762913951020892, -39.99999999999961631, -41.69427287692722928 ) ) ;
#12943 = CARTESIAN_POINT ( 'NONE',  ( 91.82158438592156813, 39.99999999999986500, 17.20528682183341473 ) ) ;
#12944 = CARTESIAN_POINT ( 'NONE',  ( -109.1264249741455075, -13.72187187124534802, -33.12752917268997521 ) ) ;
#12945 = CARTESIAN_POINT ( 'NONE',  ( 199.0263771353515949, -14.14574067859894413, 14.14574067859863682 ) ) ;
#12946 = CARTESIAN_POINT ( 'NONE',  ( 199.0055119247266759, 16.54204028020789252, -11.23294693469441263 ) ) ;
#12947 = CARTESIAN_POINT ( 'NONE',  ( -189.0115211946945237, 17.94954316430204599, 43.33403054566034740 ) ) ;
#12948 = CARTESIAN_POINT ( 'NONE',  ( -192.9588430854689989, -10.23066800230742501, -10.23066800230756712 ) ) ;
#12949 = CARTESIAN_POINT ( 'NONE',  ( -103.9474983245001738, 8.577167319634607878, 19.92928099173801826 ) ) ;
#12950 = CARTESIAN_POINT ( 'NONE',  ( -56.48582580120559982, 34.75652343174597547, 21.81201906317791384 ) ) ;
#12951 = CARTESIAN_POINT ( 'NONE',  ( -86.86493150571116928, -19.60045294882770861, 8.366608963953762412 ) ) ;
#12952 = CARTESIAN_POINT ( 'NONE',  ( -192.9588430854690273, -10.23066800231931239, -66.79921049724377724 ) ) ;
#12953 = CARTESIAN_POINT ( 'NONE',  ( -199.9999999999998863, 44.86667451853075050, -23.83166235904688435 ) ) ;
#12954 = CARTESIAN_POINT ( 'NONE',  ( 192.4448373802101173, 20.00000000003945644, 40.00000000000002132 ) ) ;
#12955 = CARTESIAN_POINT ( 'NONE',  ( 14.38125909742180220, 39.01709431150892016, 17.55144818341517166 ) ) ;
#12956 = CARTESIAN_POINT ( 'NONE',  ( 184.8905102610680444, -19.07866798485554938, 40.00000000000002132 ) ) ;
#12957 = DIRECTION ( 'NONE',  ( 0.2259624730536665960, 0.000000000000000000, -0.9741360073272474773 ) ) ;
#12958 = ORIENTED_EDGE ( 'NONE', *, *, #3151, .T. ) ;
#12959 = CARTESIAN_POINT ( 'NONE',  ( -192.9588430854690273, -39.99999999999948841, -54.46834944098263520 ) ) ;
#12960 = CARTESIAN_POINT ( 'NONE',  ( 199.0083509329244293, 0.2901128837469029720, -19.99442784571252929 ) ) ;
#12961 = CARTESIAN_POINT ( 'NONE',  ( 149.5797498300188977, -12.18602109748358941, 29.41965740490864079 ) ) ;
#12962 = VERTEX_POINT ( 'NONE', #20404 ) ;
#12963 = ORIENTED_EDGE ( 'NONE', *, *, #15952, .T. ) ;
#12964 = ORIENTED_EDGE ( 'NONE', *, *, #18007, .T. ) ;
#12965 = CARTESIAN_POINT ( 'NONE',  ( 19.06497207195980792, 54.19242893257843718, 2.449293598294708485E-15 ) ) ;
#12966 =( NAMED_UNIT ( * ) PLANE_ANGLE_UNIT ( ) SI_UNIT ( $, .RADIAN. ) );
#12967 = CARTESIAN_POINT ( 'NONE',  ( -105.2276882639529845, -21.34721338856009609, -2.726203881900004955 ) ) ;
#12968 = CARTESIAN_POINT ( 'NONE',  ( -199.9999999999999432, 55.16984130226870064, 6.983587721173168283 ) ) ;
#12969 = PRODUCT_RELATED_PRODUCT_CATEGORY ( 'part', '', ( #15879 ) ) ;
#12970 = LINE ( 'NONE', #13103, #16827 ) ;
#12971 = CARTESIAN_POINT ( 'NONE',  ( 200.0000000000000284, -3.097043465352568248, -18.74877632928372151 ) ) ;
#12972 = CARTESIAN_POINT ( 'NONE',  ( 199.9999999999999716, 0.6106555654018747115, -19.00184299465770366 ) ) ;
#12973 = CARTESIAN_POINT ( 'NONE',  ( -105.3755690713226585, -15.38646221621738164, -41.18208027870615240 ) ) ;
#12974 = CARTESIAN_POINT ( 'NONE',  ( -162.0762913951020892, -1.198031840385767266, -1.198031840385758384 ) ) ;
#12975 = CARTESIAN_POINT ( 'NONE',  ( -110.1017833365194321, -15.17210968201788823, -13.38817875465654517 ) ) ;
#12976 = CARTESIAN_POINT ( 'NONE',  ( 57.59792236341147742, 4.064940816252731242E-13, -37.56421063658186199 ) ) ;
#12977 = DIRECTION ( 'NONE',  ( 0.000000000000000000, -1.000000000000000000, 0.000000000000000000 ) ) ;
#12978 = CARTESIAN_POINT ( 'NONE',  ( -3.763361371728489946, 13.84281709279663808, 47.08953757622903424 ) ) ;
#12979 = CARTESIAN_POINT ( 'NONE',  ( -135.8532207217289738, 6.472252184283881604, 50.09629031063969506 ) ) ;
#12980 = FACE_OUTER_BOUND ( 'NONE', #22909, .T. ) ;
#12981 = EDGE_CURVE ( 'NONE', #25845, #23734, #1737, .T. ) ;
#12983 = CARTESIAN_POINT ( 'NONE',  ( -192.9588430854689989, -8.596193650988133061E-14, 14.46834944099969533 ) ) ;
#12982 = CARTESIAN_POINT ( 'NONE',  ( -280.0000000000000000, -14.14213562373118549, 14.14213562373078936 ) ) ;
#12984 = AXIS2_PLACEMENT_3D ( 'NONE', #7305, #17667, #1331 ) ;
#12985 = CARTESIAN_POINT ( 'NONE',  ( -210.0000000000000284, -69.99999999999998579, 8.572527594031471415E-15 ) ) ;
#12986 = CARTESIAN_POINT ( 'NONE',  ( -238.4067589809705794, 0.6820004457340470561, 57.25054294065803617 ) ) ;
#12987 = CARTESIAN_POINT ( 'NONE',  ( -192.9588430854690273, 14.46834944099966336, 40.00000000000002132 ) ) ;
#12988 = ORIENTED_EDGE ( 'NONE', *, *, #10932, .F. ) ;
#12989 = CARTESIAN_POINT ( 'NONE',  ( 21.25019396252282178, -43.56030393974950243, 18.04326867294216896 ) ) ;
#12990 =( GEOMETRIC_REPRESENTATION_CONTEXT ( 3 ) GLOBAL_UNCERTAINTY_ASSIGNED_CONTEXT ( ( #5552 ) ) GLOBAL_UNIT_ASSIGNED_CONTEXT ( ( #5889, #8144, #14398 ) ) REPRESENTATION_CONTEXT ( 'NONE', 'WORKASPACE' ) );
#12991 = AXIS2_PLACEMENT_3D ( 'NONE', #8693, #24401, #14667 ) ;
#12992 = CARTESIAN_POINT ( 'NONE',  ( 4.995406935893288214, 15.24977328854832770, -40.00000000000002132 ) ) ;
#12993 = CARTESIAN_POINT ( 'NONE',  ( -716.9846540392142060, 52.50000000000007816, 52.49999999999999289 ) ) ;
#12994 = CARTESIAN_POINT ( 'NONE',  ( -135.8532207217289738, -6.472252184284287502, 50.09629031063965243 ) ) ;
#12995 = CARTESIAN_POINT ( 'NONE',  ( 199.9999999999999432, 1.065690307512836407E-13, -20.00000000000010303 ) ) ;
#12996 = CARTESIAN_POINT ( 'NONE',  ( -82.24214707262626689, 20.09197113510544241, -2.401591935735043926 ) ) ;
#12997 = VECTOR ( 'NONE', #556, 1000.000000000000000 ) ;
#12998 = CIRCLE ( 'NONE', #4076, 14.99999999999999822 ) ;
#12999 = PRODUCT_DEFINITION_FORMATION_WITH_SPECIFIED_SOURCE ( 'ANY', '', #10623, .NOT_KNOWN. ) ;
#13000 = CARTESIAN_POINT ( 'NONE',  ( -62.69292774209460362, 11.76166271882766523, -24.97541154606644653 ) ) ;
#13001 = CARTESIAN_POINT ( 'NONE',  ( 199.0256572979843099, -18.35487425740099354, 7.962169344204487409 ) ) ;
#13002 = CARTESIAN_POINT ( 'NONE',  ( -91.56559293963834989, -16.03295912088728414, 16.03295912088688269 ) ) ;
#13003 = CARTESIAN_POINT ( 'NONE',  ( -77.70139926393163421, -21.34823270893657110, 5.508459030604740292 ) ) ;
#13004 = DIRECTION ( 'NONE',  ( 1.000000000000000000, 1.836970198721030181E-16, 0.000000000000000000 ) ) ;
#13005 = CARTESIAN_POINT ( 'NONE',  ( -188.2957210513755797, -23.44847782072233144, 43.00408675155275517 ) ) ;
#13006 = CARTESIAN_POINT ( 'NONE',  ( 4.995406935893290878, 1.606505379428369110E-13, -15.24977328854832592 ) ) ;
#13007 = CARTESIAN_POINT ( 'NONE',  ( -56.48582580120559271, 6.472252184284211118, -6.472252184284153387 ) ) ;
#13008 = CARTESIAN_POINT ( 'NONE',  ( -190.0000000000000284, -82.49999999999990052, 52.49999999999977973 ) ) ;
#13009 = CARTESIAN_POINT ( 'NONE',  ( -91.56559293963836410, 44.31723036834908669, -12.25131212657445801 ) ) ;
#13010 = AXIS2_PLACEMENT_3D ( 'NONE', #3057, #13665, #19788 ) ;
#13012 = CARTESIAN_POINT ( 'NONE',  ( 14.38125909742181108, 39.01709431150961649, -39.01709431150867147 ) ) ;
#13011 = FACE_OUTER_BOUND ( 'NONE', #20979, .T. ) ;
#13013 = CARTESIAN_POINT ( 'NONE',  ( -198.0356074513804572, 10.87444709761036066, -67.44298959253325165 ) ) ;
#13014 = CARTESIAN_POINT ( 'NONE',  ( -105.3755690713226727, -21.75974354311652093, 0.000000000000000000 ) ) ;
#13015 = B_SPLINE_CURVE_WITH_KNOTS ( 'NONE', 3,
 ( #5944, #26049, #7786, #15768, #3417, #19772, #20050, #13778, #7397, #22186, #26188, #15637, #7654, #15902, #7927, #17512, #3960, #7529, #24031, #12058, #23640, #20177, #1428, #1828, #5810, #13915, #5418, #24169, #9407, #22050, #21775, #9528, #25651, #11925, #9666, #13519, #9930, #21645, #18036, #11519, #19644, #25779, #23763, #21908, #5543, #1561 ),
 .UNSPECIFIED., .F., .F.,
 ( 4, 2, 2, 2, 2, 2, 2, 2, 2, 2, 2, 2, 2, 2, 2, 2, 2, 2, 2, 2, 2, 2, 4 ),
 ( -5.298243351209276186E-05, 0.005693729153214702014, 0.01144044073994149660, 0.02293386391339508404, 0.04592071026030229708, 0.05741413343375589146, 0.06890755660720948583, 0.07465426819393627955, 0.07752762398729966253, 0.07896430188398136096, 0.08040097978066305939, 0.08614769136738986699, 0.09189440295411666071, 0.09476775874748007145, 0.09764111454084345443, 0.1033878261275702481, 0.1062611819209336589, 0.1076978598176153573, 0.1091345377142970419, 0.1148812493010238633, 0.1378680956479311215, 0.1608549419948383796, 0.1838417883417456655 ),
 .UNSPECIFIED. ) ;
#13016 = CARTESIAN_POINT ( 'NONE',  ( 192.4448373802101173, 14.14213562370320076, -42.42640687122072762 ) ) ;
#13017 = DIRECTION ( 'NONE',  ( 0.000000000000000000, -1.000000000000000000, 0.000000000000000000 ) ) ;
#13018 = CARTESIAN_POINT ( 'NONE',  ( 57.59792236341148453, -54.84617931850879557, 1.722363176414566155 ) ) ;
#13019 = CARTESIAN_POINT ( 'NONE',  ( -188.3065677117056396, 46.99298756134918875, -13.82848612971604751 ) ) ;
#13020 = ORIENTED_EDGE ( 'NONE', *, *, #15149, .T. ) ;
#13021 = AXIS2_PLACEMENT_3D ( 'NONE', #15918, #3699, #5827 ) ;
#13022 = CARTESIAN_POINT ( 'NONE',  ( -192.9588430854689989, 38.51493924976929861, 38.51493924976947625 ) ) ;
#13023 = CARTESIAN_POINT ( 'NONE',  ( -678.9461782662789346, 75.00000000000000000, -34.99999999999845812 ) ) ;
#13024 = CARTESIAN_POINT ( 'NONE',  ( -208.1127848780264742, 17.67593391476624021, 38.89260858015742883 ) ) ;
#13025 = CARTESIAN_POINT ( 'NONE',  ( 98.29850319075929121, -18.72964005484536187, -7.044854747077215151 ) ) ;
#13026 = ORIENTED_EDGE ( 'NONE', *, *, #24745, .F. ) ;
#13027 = CARTESIAN_POINT ( 'NONE',  ( -187.3036811847654803, -46.64553187115656385, 13.75782060302593379 ) ) ;
#13028 = CARTESIAN_POINT ( 'NONE',  ( 199.9999999999999147, 16.22794370004292830, -9.883520089760141403 ) ) ;
#13029 = DIRECTION ( 'NONE',  ( 0.000000000000000000, 1.000000000000000000, 0.000000000000000000 ) ) ;
#13030 = B_SPLINE_CURVE_WITH_KNOTS ( 'NONE', 3,
 ( #12673, #14797, #20936, #22928, #714, #2574 ),
 .UNSPECIFIED., .F., .F.,
 ( 4, 2, 4 ),
 ( 0.0002283644213467581811, 0.004316914013642671882, 0.008405463605938585936 ),
 .UNSPECIFIED. ) ;
#13031 =( BOUNDED_CURVE ( )  B_SPLINE_CURVE ( 3, ( #26254, #16109, #6012, #16246 ),
 .UNSPECIFIED., .F., .T. ) 
 B_SPLINE_CURVE_WITH_KNOTS ( ( 4, 4 ),
 ( 0.007854122480103177539, 0.01576650722530729271 ),
 .UNSPECIFIED. ) 
 CURVE ( )  GEOMETRIC_REPRESENTATION_ITEM ( )  RATIONAL_B_SPLINE_CURVE ( ( 0.5857864376268384632, 0.5560595459730424128, 0.5340584217468479222, 0.5197830649482548804 ) ) 
 REPRESENTATION_ITEM ( '' )  );
#13032 = CARTESIAN_POINT ( 'NONE',  ( -259.2033419157646676, 30.48217210827735713, -40.00000000000002132 ) ) ;
#13033 = DIRECTION ( 'NONE',  ( 0.000000000000000000, 0.000000000000000000, 1.000000000000000000 ) ) ;
#13034 = CARTESIAN_POINT ( 'NONE',  ( 199.0201394418415077, 7.332745681712491859, 18.61237044096938575 ) ) ;
#13035 = CARTESIAN_POINT ( 'NONE',  ( 14.38125909742181818, -39.01709431150928253, 17.55144818341435808 ) ) ;
#13036 = CARTESIAN_POINT ( 'NONE',  ( 184.8905102610680444, -3.509827109981123710E-14, 19.07866798485558490 ) ) ;
#13037 = CARTESIAN_POINT ( 'NONE',  ( -105.3755690713226585, 39.99999999999993605, 18.24025645688366737 ) ) ;
#13038 = CARTESIAN_POINT ( 'NONE',  ( -192.1131556193065819, -24.17676952300933380, -43.98783656160069455 ) ) ;
#13039 = CARTESIAN_POINT ( 'NONE',  ( -86.96347745069643054, -18.24025645688353947, -40.00000000000002132 ) ) ;
#13041 = CARTESIAN_POINT ( 'NONE',  ( -620.4318289324395437, 27.25272540324414550, 29.27987691734877274 ) ) ;
#13040 = CARTESIAN_POINT ( 'NONE',  ( 23.17367289775620876, -23.38495170326278583, -42.91822977676284978 ) ) ;
#13042 = CARTESIAN_POINT ( 'NONE',  ( -30.26275506840323004, -41.69427246844629309, 40.00000000000002132 ) ) ;
#13043 = CARTESIAN_POINT ( 'NONE',  ( -30.26275506840325136, 27.08623969584573388, 29.48230279907808793 ) ) ;
#13044 = CARTESIAN_POINT ( 'NONE',  ( -86.96347745069645896, 39.99999999999977973, 21.75974354311691883 ) ) ;
#13045 = CARTESIAN_POINT ( 'NONE',  ( -110.0947178154681296, 15.96121929954245822, -12.38433105676308799 ) ) ;
#13046 = CARTESIAN_POINT ( 'NONE',  ( 184.8905102610680444, 2.362515690532070066E-13, -19.07866798485558490 ) ) ;
#13047 = CARTESIAN_POINT ( 'NONE',  ( -208.1127848780265026, 10.60833733269537049, 10.60833733269544510 ) ) ;
#13048 = CARTESIAN_POINT ( 'NONE',  ( 200.0000000000000000, 61.50000000000009948, -66.50000000000005684 ) ) ;
#13049 = CARTESIAN_POINT ( 'NONE',  ( 199.9999999999999432, -14.14213562373115884, 14.14213562373085153 ) ) ;
#13050 = CARTESIAN_POINT ( 'NONE',  ( 170.2234770963711128, -10.92277846919202666, 10.92277846919193962 ) ) ;
#13051 = ORIENTED_EDGE ( 'NONE', *, *, #4702, .F. ) ;
#13053 = CARTESIAN_POINT ( 'NONE',  ( -47.50817905881116587, 30.33575659741672226, -12.56548180764576905 ) ) ;
#13052 = CARTESIAN_POINT ( 'NONE',  ( -86.96347745069644475, 15.38646221621772092, 15.38646221621800336 ) ) ;
#13054 = CARTESIAN_POINT ( 'NONE',  ( 156.5537079553356818, 27.23618587942436164, -11.28159757857213208 ) ) ;
#13055 = CARTESIAN_POINT ( 'NONE',  ( 163.1118516004056573, -12.73709011382472234, -2.449293598294708485E-15 ) ) ;
#13056 = CARTESIAN_POINT ( 'NONE',  ( -114.4364955367327070, 8.644468109209567430, -20.04994829327642947 ) ) ;
#13057 = CARTESIAN_POINT ( 'NONE',  ( -188.9478457324744625, 43.31767415847507152, -17.94276812689866674 ) ) ;
#13058 = ORIENTED_EDGE ( 'NONE', *, *, #16393, .F. ) ;
#13059 = EDGE_LOOP ( 'NONE', ( #14521, #18411 ) ) ;
#13060 = DIRECTION ( 'NONE',  ( 1.000000000000000000, -1.836970198721030181E-16, -0.000000000000000000 ) ) ;
#13061 = CARTESIAN_POINT ( 'NONE',  ( 159.7744820660626317, 10.75261058663767422, -25.95909830917682370 ) ) ;
#13062 = ORIENTED_EDGE ( 'NONE', *, *, #2653, .T. ) ;
#13063 = CIRCLE ( 'NONE', #294, 14.99999999999999822 ) ;
#13064 = EDGE_CURVE ( 'NONE', #18341, #22608, #12146, .T. ) ;
#13065 = ORIENTED_EDGE ( 'NONE', *, *, #20542, .F. ) ;
#13066 = CARTESIAN_POINT ( 'NONE',  ( 199.0163032586025622, -14.59919991228128922, -13.67396374720910757 ) ) ;
#13067 = CARTESIAN_POINT ( 'NONE',  ( -110.0563856373237002, -6.246938629525583764, 19.19543633473636746 ) ) ;
#13068 = EDGE_CURVE ( 'NONE', #13433, #862, #5148, .T. ) ;
#13069 = CARTESIAN_POINT ( 'NONE',  ( -86.96347745069644475, -43.67073346367983788, 12.89780903124397149 ) ) ;
#13070 = AXIS2_PLACEMENT_3D ( 'NONE', #24442, #18581, #24578 ) ;
#13071 = CARTESIAN_POINT ( 'NONE',  ( 0.2972598230769938343, 10.13633138497472252, 10.13633138497475628 ) ) ;
#13072 = CARTESIAN_POINT ( 'NONE',  ( -56.48582580120559982, 39.99999999999990763, 30.84685318188658698 ) ) ;
#13073 = CARTESIAN_POINT ( 'NONE',  ( -200.0000000000000568, -46.38610861938602881, 18.14877749763665804 ) ) ;
#13074 = EDGE_CURVE ( 'NONE', #23831, #11213, #12803, .T. ) ;
#13075 = EDGE_CURVE ( 'NONE', #17450, #7956, #24274, .T. ) ;
#13076 = CARTESIAN_POINT ( 'NONE',  ( 4.995406935893306866, -39.99999999999944578, -55.24977328856505920 ) ) ;
#13077 = CARTESIAN_POINT ( 'NONE',  ( -162.0762913951020892, 4.094006889353306706E-13, -41.69427287682835015 ) ) ;
#13078 = CARTESIAN_POINT ( 'NONE',  ( -77.93386762624879793, 20.16917687840208373, 8.295512132613184875 ) ) ;
#13079 = CARTESIAN_POINT ( 'NONE',  ( -87.11144460387475874, 13.16696799080288294, 17.02331989627854725 ) ) ;
#13080 = CARTESIAN_POINT ( 'NONE',  ( 199.0056246187962188, 17.07746298573517052, -10.40099104823843312 ) ) ;
#13081 = CARTESIAN_POINT ( 'NONE',  ( 0.2972598230769976091, -10.13633138497479180, 10.13633138497468522 ) ) ;
#13082 = CARTESIAN_POINT ( 'NONE',  ( 128.5824617753800396, 28.96492468983269220, 11.99766463964413354 ) ) ;
#13083 = CARTESIAN_POINT ( 'NONE',  ( 160.9163046357249129, -205.7889608577475542, -49.61140153332241454 ) ) ;
#13084 = CYLINDRICAL_SURFACE ( 'NONE', #25477, 75.00000000000000000 ) ;
#13085 = CARTESIAN_POINT ( 'NONE',  ( -77.70150415250706999, -11.19846400429647559, 18.99169997607589977 ) ) ;
#13086 = CARTESIAN_POINT ( 'NONE',  ( 192.4448373802100889, -14.14213562370293431, -14.14213562370322030 ) ) ;
#13087 = CARTESIAN_POINT ( 'NONE',  ( -173.7925586252259507, -12.78856870752416697, -41.93433064649377684 ) ) ;
#13088 = CARTESIAN_POINT ( 'NONE',  ( -77.78698611455740775, 9.956332155370628101, 19.58753816231132205 ) ) ;
#13089 = ORIENTED_EDGE ( 'NONE', *, *, #23903, .F. ) ;
#13090 = CARTESIAN_POINT ( 'NONE',  ( 14.38125909742180752, 10.73282306404735387, -10.73282306404708919 ) ) ;
#13091 = CARTESIAN_POINT ( 'NONE',  ( -678.9461782662772293, 90.00000000000000000, 35.00000000000159162 ) ) ;
#13092 = CARTESIAN_POINT ( 'NONE',  ( -591.9853919005129228, 44.99942610803522314, -0.6435327916369084633 ) ) ;
#13093 = VERTEX_POINT ( 'NONE', #10154 ) ;
#13094 = CARTESIAN_POINT ( 'NONE',  ( 14.38125909742181818, 5.830552384690105017E-13, -55.17850393972636880 ) ) ;
#13095 = CARTESIAN_POINT ( 'NONE',  ( 199.0078439946754827, 1.701626800721226074, -19.92628250063794226 ) ) ;
#13096 = CARTESIAN_POINT ( 'NONE',  ( -105.4894168351564048, 19.67999904371083275, 8.151722511394638104 ) ) ;
#13097 = ORIENTED_EDGE ( 'NONE', *, *, #21816, .F. ) ;
#13098 = VERTEX_POINT ( 'NONE', #5895 ) ;
#13099 = ORIENTED_EDGE ( 'NONE', *, *, #5110, .T. ) ;
#13100 = CARTESIAN_POINT ( 'NONE',  ( 184.8905102610680444, 19.07866798485562043, 2.449293598294708485E-15 ) ) ;
#13101 =( LENGTH_UNIT ( ) NAMED_UNIT ( * ) SI_UNIT ( .MILLI., .METRE. ) );
#13102 = CARTESIAN_POINT ( 'NONE',  ( -77.79405973474285929, -19.55084590669412137, 9.945757298486981313 ) ) ;
#13103 = CARTESIAN_POINT ( 'NONE',  ( 180.0000000000000284, -135.7889608577475542, 2.284182285366599633E-14 ) ) ;
#13104 = CARTESIAN_POINT ( 'NONE',  ( 199.9999999999998579, -16.14759498898286338, -10.02975912355057453 ) ) ;
#13105 = CARTESIAN_POINT ( 'NONE',  ( 200.0000000000000000, -52.49999999999972289, -82.49999999999998579 ) ) ;
#13106 = CARTESIAN_POINT ( 'NONE',  ( -192.9588430854689989, 10.23066800230756712, -10.23066800230735396 ) ) ;
#13107 = CARTESIAN_POINT ( 'NONE',  ( 163.1118516004056573, 19.27778845538753316, 19.27778845538783870 ) ) ;
#13108 = DIRECTION ( 'NONE',  ( 1.000000000000000000, 1.836970198721030427E-16, -0.000000000000000000 ) ) ;
#13109 = CARTESIAN_POINT ( 'NONE',  ( -91.56559293963834989, -39.99999999999985789, -17.32597176626853042 ) ) ;
#13110 = CARTESIAN_POINT ( 'NONE',  ( 130.8568914410475372, 24.07718906447210472, 24.07718906447249907 ) ) ;
#13111 = CARTESIAN_POINT ( 'NONE',  ( 4.995406935893307754, -55.24977328853207581, -40.00000000000002132 ) ) ;
#13112 = CARTESIAN_POINT ( 'NONE',  ( -86.96347745069643054, 15.38646221621763210, 41.18208027870604582 ) ) ;
#13113 = CARTESIAN_POINT ( 'NONE',  ( 199.0058908291898376, 17.93471286599577397, -8.846248472678716723 ) ) ;
#13115 = CARTESIAN_POINT ( 'NONE',  ( -280.0000000000000568, 40.00000000000004263, -19.99999999999987210 ) ) ;
#13114 = CARTESIAN_POINT ( 'NONE',  ( -135.8532207217289738, -34.75652343174584757, -21.81201906317816253 ) ) ;
#13116 = CARTESIAN_POINT ( 'NONE',  ( 184.8905102610680444, -20.92133201514440799, 0.000000000000000000 ) ) ;
#13117 = CARTESIAN_POINT ( 'NONE',  ( -213.1075012329537230, 9.698598906462684965, 66.26714140138669507 ) ) ;
#13118 = CARTESIAN_POINT ( 'NONE',  ( 136.1360204305621266, -35.03383547441293899, 0.000000000000000000 ) ) ;
#13120 = ORIENTED_EDGE ( 'NONE', *, *, #7013, .F. ) ;
#13119 = AXIS2_PLACEMENT_3D ( 'NONE', #13317, #3210, #1474 ) ;
#13121 = CARTESIAN_POINT ( 'NONE',  ( 22.13784119383794291, -43.34234508276703224, 17.95298715833492764 ) ) ;
#13122 = CARTESIAN_POINT ( 'NONE',  ( 0.2972598230769930017, 14.33493731733933352, -40.00000000000002132 ) ) ;
#13123 = DIRECTION ( 'NONE',  ( 0.000000000000000000, 0.9767746502210202797, -0.2142691827715865471 ) ) ;
#13124 = CARTESIAN_POINT ( 'NONE',  ( -208.1127848780265026, 38.89260858015724409, 38.89260858015741462 ) ) ;
#13125 = CARTESIAN_POINT ( 'NONE',  ( -213.1075012329537230, -8.703598725189323045E-14, 13.71589010951911902 ) ) ;
#13126 = CARTESIAN_POINT ( 'NONE',  ( -82.28220112168970957, 19.20590466794900664, -6.216954113673384796 ) ) ;
#13127 = CARTESIAN_POINT ( 'NONE',  ( 190.0000000000000000, -61.50000000000001421, -66.50000000000005684 ) ) ;
#13128 = CARTESIAN_POINT ( 'NONE',  ( 199.9999999999999432, -11.20938440123365432, 15.35472082164171326 ) ) ;
#13129 = ADVANCED_FACE ( 'NONE', ( #14003 ), #18394, .T. ) ;
#13130 = B_SPLINE_CURVE_WITH_KNOTS ( 'NONE', 3,
 ( #4195, #14017, #9897, #12288, #22547, #22147, #20416, #1923, #4328, #13881, #6561, #25076 ),
 .UNSPECIFIED., .F., .F.,
 ( 4, 2, 2, 2, 2, 4 ),
 ( 1.723928531167631343E-15, 0.004698945756008387348, 0.007048418634011698047, 0.009397891512015008747, 0.01409683726802167178, 0.01879578302402833481 ),
 .UNSPECIFIED. ) ;
#13131 = CARTESIAN_POINT ( 'NONE',  ( 91.82158438592158234, -12.16597498397778843, 12.16597498397750954 ) ) ;
#13132 = CARTESIAN_POINT ( 'NONE',  ( -82.24889283716301236, -19.94440861092025585, 3.157952835704525896 ) ) ;
#13133 = CARTESIAN_POINT ( 'NONE',  ( 98.29820294267493352, -20.00000000000511235, 5.223721743777709619E-12 ) ) ;
#13135 = CARTESIAN_POINT ( 'NONE',  ( -200.4318156386385965, -24.83634777281915618, 44.88237417767410875 ) ) ;
#13134 = AXIS2_PLACEMENT_3D ( 'NONE', #19224, #747, #25099 ) ;
#13136 = CARTESIAN_POINT ( 'NONE',  ( 199.9999999999999432, 14.14213562373093680, 14.14213562373114641 ) ) ;
#13137 = CARTESIAN_POINT ( 'NONE',  ( -30.26275506840324070, -1.198031551616032919, 1.198031551616014712 ) ) ;
#13138 = CARTESIAN_POINT ( 'NONE',  ( -348.0000000000001137, -4.857225732735059864E-14, 0.000000000000000000 ) ) ;
#13139 = CARTESIAN_POINT ( 'NONE',  ( -100.7734535825088500, 16.03295912088691821, 16.03295912088721309 ) ) ;
#13141 = CARTESIAN_POINT ( 'NONE',  ( -208.1127848780265026, 38.89260858015777700, -38.89260858015687461 ) ) ;
#13140 = CARTESIAN_POINT ( 'NONE',  ( 170.2234770963711128, 17.36149277826980253, 17.36149277827007253 ) ) ;
#13142 = CARTESIAN_POINT ( 'NONE',  ( -56.48582580120559982, -6.472252184283581400, -50.09629031063973059 ) ) ;
#13143 = CARTESIAN_POINT ( 'NONE',  ( 136.1360204305621551, -35.03383547441293899, -40.00000000000002132 ) ) ;
#13144 = CARTESIAN_POINT ( 'NONE',  ( -91.56559293963834989, -16.03295912088706388, -16.03295912088710651 ) ) ;
#13145 = DIRECTION ( 'NONE',  ( 0.000000000000000000, 0.000000000000000000, -1.000000000000000000 ) ) ;
#13146 = CARTESIAN_POINT ( 'NONE',  ( -192.9588430854690273, -38.51493924976957572, 18.05360324515410397 ) ) ;
#13147 = CARTESIAN_POINT ( 'NONE',  ( -187.7698581930969510, 42.84913646251646924, -23.34605429453463543 ) ) ;
#13149 = EDGE_CURVE ( 'NONE', #4428, #2784, #4736, .T. ) ;
#13148 = ORIENTED_EDGE ( 'NONE', *, *, #21918, .F. ) ;
#13150 = CARTESIAN_POINT ( 'NONE',  ( 4.995406935893290878, 39.06748935135185263, 39.06748935135198764 ) ) ;
#13151 = FACE_OUTER_BOUND ( 'NONE', #20391, .T. ) ;
#13152 = CARTESIAN_POINT ( 'NONE',  ( -62.69292774223515607, -25.97703433354730862, -9.343531400732226544 ) ) ;
#13153 = ORIENTED_EDGE ( 'NONE', *, *, #190, .F. ) ;
#13154 = CARTESIAN_POINT ( 'NONE',  ( -190.0000000000000000, -66.50000000000001421, 66.50000000000005684 ) ) ;
#13155 = CARTESIAN_POINT ( 'NONE',  ( 200.0000000000001705, 1.541304384858841692, -18.93928971938424155 ) ) ;
#13156 = CARTESIAN_POINT ( 'NONE',  ( 23.35928221536310190, -23.34300348377129453, 42.86167611819467993 ) ) ;
#13157 = CARTESIAN_POINT ( 'NONE',  ( -91.56559293963834989, -22.67402823373193499, -40.00000000000002132 ) ) ;
#13158 = CARTESIAN_POINT ( 'NONE',  ( -362.0709805440841365, -4.857225732735059864E-14, 0.000000000000000000 ) ) ;
#13159 = CARTESIAN_POINT ( 'NONE',  ( 199.0085879884812243, 19.99611484057871280, 0.3390174452003563710 ) ) ;
#13160 = CARTESIAN_POINT ( 'NONE',  ( -100.7734535825088500, -40.53558337403692491, 16.03295912088671571 ) ) ;
#13161 = CARTESIAN_POINT ( 'NONE',  ( 4.995406935893283773, 39.99999999999997158, 15.24977328854846803 ) ) ;
#13162 = CARTESIAN_POINT ( 'NONE',  ( 210.0000000000000284, 60.27431767988573341, -73.32453023895050137 ) ) ;
#13163 = CARTESIAN_POINT ( 'NONE',  ( -4.039451493210481026, -46.99046209229813797, 13.82811171175447917 ) ) ;
#13164 = CARTESIAN_POINT ( 'NONE',  ( 184.8905102610680444, -19.07866798485553872, -40.00000000000002132 ) ) ;
#13166 = CARTESIAN_POINT ( 'NONE',  ( 151.7948205124836250, 23.49921654116361225, -23.49921654116333514 ) ) ;
#13165 = CARTESIAN_POINT ( 'NONE',  ( 19.94008347559031691, -24.01421467035550350, -43.76810615268311011 ) ) ;
#13167 = CARTESIAN_POINT ( 'NONE',  ( 19.06497207195980792, -14.19242893257839988, 40.00000000000002132 ) ) ;
#13168 = CARTESIAN_POINT ( 'NONE',  ( 184.8905102610680444, 14.79361573936396113, -14.79361573936377461 ) ) ;
#13169 = CARTESIAN_POINT ( 'NONE',  ( 136.1360204305621551, 39.99999999999968026, 35.03383547441337953 ) ) ;
#13170 = CARTESIAN_POINT ( 'NONE',  ( -105.4741150117381778, 8.366608964590609432, -19.60045294982858977 ) ) ;
#13171 = CARTESIAN_POINT ( 'NONE',  ( -91.56559293963834989, -39.99999999999985789, -17.32597176626853042 ) ) ;
#13172 = CARTESIAN_POINT ( 'NONE',  ( 199.0255290512018291, -7.361955815226616906, 18.60363316911454845 ) ) ;
#13173 = DIRECTION ( 'NONE',  ( -1.000000000000000000, 0.000000000000000000, 0.000000000000000000 ) ) ;
#13174 = CARTESIAN_POINT ( 'NONE',  ( -56.48582580120559271, -6.472252184284276844, 6.472252184284108978 ) ) ;
#13175 = CARTESIAN_POINT ( 'NONE',  ( -135.8532207217289738, 34.75652343174594705, 21.81201906317792449 ) ) ;
#13176 = VERTEX_POINT ( 'NONE', #20268 ) ;
#13178 = CARTESIAN_POINT ( 'NONE',  ( -4.339409867971697921, 43.06267456183267939, -17.83714383556867489 ) ) ;
#13177 = CARTESIAN_POINT ( 'NONE',  ( 199.9999999999999716, 82.50000000000008527, -52.49999999999977973 ) ) ;
#13179 = CARTESIAN_POINT ( 'NONE',  ( 136.1360204305621266, 35.03383547441298163, 40.00000000000002132 ) ) ;
#13180 = AXIS2_PLACEMENT_3D ( 'NONE', #8528, #4557, #16514 ) ;
#13181 = CARTESIAN_POINT ( 'NONE',  ( -188.4265004370346901, 47.03620155434742145, -13.83489460444945607 ) ) ;
#13182 = CARTESIAN_POINT ( 'NONE',  ( 0.000000000000000000, 0.000000000000000000, 0.000000000000000000 ) ) ;
#13183 = ORIENTED_EDGE ( 'NONE', *, *, #6868, .T. ) ;
#13184 = ORIENTED_EDGE ( 'NONE', *, *, #19486, .F. ) ;
#13185 = CARTESIAN_POINT ( 'NONE',  ( -96.93773665438806120, 9.001171854902148439, -20.58457565566403602 ) ) ;
#13186 = CARTESIAN_POINT ( 'NONE',  ( -716.9846540392142060, -82.49999999999991473, -52.49999999999977973 ) ) ;
#13187 = CARTESIAN_POINT ( 'NONE',  ( 151.7948205124836250, 1.439163438361279259E-13, -33.23291073765553705 ) ) ;
#13188 = ORIENTED_EDGE ( 'NONE', *, *, #25121, .F. ) ;
#13189 =( BOUNDED_SURFACE ( )  B_SPLINE_SURFACE ( 3, 3, ( 
 ( #18119, #8272, #16526, #10011, #10540, #16123, #22660, #2042, #12401, #6542, #10145, #18251, #22127, #16394, #33, #12271, #10280, #167, #20524, #6410, #14527, #6935, #10946, #10811, #19182, #23182, #11188, #6806, #572, #23059 ),
 ( #8944, #21314, #14919, #2563, #14651, #24922, #15053, #4831, #4962, #19053, #18922, #966, #13069, #19303, #12937, #16787, #25055, #17308, #16921, #25312, #835, #12665, #1088, #5088, #20927, #21052, #6674, #10678, #9196, #2837 ),
 ( #25440, #17051, #25186, #9070, #21186, #2958, #8677, #20792, #2706, #706, #3088, #8810, #22791, #4569, #11068, #17177, #18791, #7071, #14789, #15185, #23311, #13192, #22919, #4698, #12801, #19815, #1602, #13818, #21687, #21950 ),
 ( #3587, #5329, #13437, #23935, #3726, #23555, #19947, #7567, #15810, #17810, #7440, #5587, #11692, #13313, #19554, #19431, #9705, #25956, #13561, #1217, #5712, #21559, #15554, #21433, #7699, #1731, #5209, #11314, #11829, #9840 ),
 ( #7190, #17680, #25568, #3333, #23679, #1342, #5458, #17944, #3206, #21815, #15306, #9320, #23433, #3462, #11559, #19680, #13693, #17428, #23805, #7314, #25822, #15428, #11433, #9447, #17552, #25690, #1469, #9572, #15680, #22223 ),
 ( #3863, #2764, #14849, #22090, #26090, #12230, #16222, #13956, #3999, #11966, #8101, #10238, #129, #18349, #18079, #5985, #20354, #2130, #7826, #18207, #14223, #1998, #12098, #24074, #20090, #10367, #20486, #1869, #26230, #14359 ),
 ( #18478, #4138, #5850, #12865, #16490, #14094, #24351, #7965, #9972, #20983, #10105, #8233, #24615, #20222, #6737, #16351, #24484, #10873, #22983, #6246, #15944, #2260, #12356, #16084, #22488, #24213, #4268, #259, #6115, #22361 ) ),
 .UNSPECIFIED., .T., .F., .F. ) 
 B_SPLINE_SURFACE_WITH_KNOTS ( ( 4, 3, 4 ),
 ( 4, 2, 2, 2, 2, 2, 2, 2, 2, 2, 2, 2, 2, 2, 4 ),
 ( 0.000000000000000000, 0.5000000000000000000, 1.000000000000000000 ),
 ( 0.000000000000000000, 0.1357259735107005372, 0.1651108541090157700, 0.1944957347073310028, 0.3598804999793158710, 0.3867117631979620773, 0.4135430264166082281, 0.5789277916885930964, 0.6062785021374117456, 0.6336292125862302838, 0.8508620842112317728, 0.8814014469398914198, 0.9119408096685510667, 0.9559704048342755334, 1.000000000000000000 ),
 .UNSPECIFIED. ) 
 GEOMETRIC_REPRESENTATION_ITEM ( )  RATIONAL_B_SPLINE_SURFACE ( (
 ( 1.000000000000000000, 1.000000000000000000, 1.000000000000000000, 1.000000000000000000, 1.000000000000000000, 1.000000000000000000, 1.000000000000000000, 1.000000000000000000, 1.000000000000000000, 1.000000000000000000, 1.000000000000000000, 1.000000000000000000, 1.000000000000000000, 1.000000000000000000, 1.000000000000000000, 1.000000000000000000, 1.000000000000000000, 1.000000000000000000, 1.000000000000000000, 1.000000000000000000, 1.000000000000000000, 1.000000000000000000, 1.000000000000000000, 1.000000000000000000, 1.000000000000000000, 1.000000000000000000, 1.000000000000000000, 1.000000000000000000, 1.000000000000000000, 1.000000000000000000),
 ( 0.3333333333333333703, 0.3333333333333333703, 0.3333333333333333703, 0.3333333333333333703, 0.3333333333333333703, 0.3333333333333333703, 0.3333333333333333703, 0.3333333333333333703, 0.3333333333333333703, 0.3333333333333333703, 0.3333333333333333703, 0.3333333333333333703, 0.3333333333333333703, 0.3333333333333333703, 0.3333333333333333703, 0.3333333333333333703, 0.3333333333333333703, 0.3333333333333333703, 0.3333333333333333703, 0.3333333333333333703, 0.3333333333333333703, 0.3333333333333333703, 0.3333333333333333703, 0.3333333333333333703, 0.3333333333333333703, 0.3333333333333333703, 0.3333333333333333703, 0.3333333333333333703, 0.3333333333333333703, 0.3333333333333333703),
 ( 0.3333333333333333703, 0.3333333333333333703, 0.3333333333333333703, 0.3333333333333333703, 0.3333333333333333703, 0.3333333333333333703, 0.3333333333333333703, 0.3333333333333333703, 0.3333333333333333703, 0.3333333333333333703, 0.3333333333333333703, 0.3333333333333333703, 0.3333333333333333703, 0.3333333333333333703, 0.3333333333333333703, 0.3333333333333333703, 0.3333333333333333703, 0.3333333333333333703, 0.3333333333333333703, 0.3333333333333333703, 0.3333333333333333703, 0.3333333333333333703, 0.3333333333333333703, 0.3333333333333333703, 0.3333333333333333703, 0.3333333333333333703, 0.3333333333333333703, 0.3333333333333333703, 0.3333333333333333703, 0.3333333333333333703),
 ( 1.000000000000000000, 1.000000000000000000, 1.000000000000000000, 1.000000000000000000, 1.000000000000000000, 1.000000000000000000, 1.000000000000000000, 1.000000000000000000, 1.000000000000000000, 1.000000000000000000, 1.000000000000000000, 1.000000000000000000, 1.000000000000000000, 1.000000000000000000, 1.000000000000000000, 1.000000000000000000, 1.000000000000000000, 1.000000000000000000, 1.000000000000000000, 1.000000000000000000, 1.000000000000000000, 1.000000000000000000, 1.000000000000000000, 1.000000000000000000, 1.000000000000000000, 1.000000000000000000, 1.000000000000000000, 1.000000000000000000, 1.000000000000000000, 1.000000000000000000),
 ( 0.3333333333333333703, 0.3333333333333333703, 0.3333333333333333703, 0.3333333333333333703, 0.3333333333333333703, 0.3333333333333333703, 0.3333333333333333703, 0.3333333333333333703, 0.3333333333333333703, 0.3333333333333333703, 0.3333333333333333703, 0.3333333333333333703, 0.3333333333333333703, 0.3333333333333333703, 0.3333333333333333703, 0.3333333333333333703, 0.3333333333333333703, 0.3333333333333333703, 0.3333333333333333703, 0.3333333333333333703, 0.3333333333333333703, 0.3333333333333333703, 0.3333333333333333703, 0.3333333333333333703, 0.3333333333333333703, 0.3333333333333333703, 0.3333333333333333703, 0.3333333333333333703, 0.3333333333333333703, 0.3333333333333333703),
 ( 0.3333333333333333703, 0.3333333333333333703, 0.3333333333333333703, 0.3333333333333333703, 0.3333333333333333703, 0.3333333333333333703, 0.3333333333333333703, 0.3333333333333333703, 0.3333333333333333703, 0.3333333333333333703, 0.3333333333333333703, 0.3333333333333333703, 0.3333333333333333703, 0.3333333333333333703, 0.3333333333333333703, 0.3333333333333333703, 0.3333333333333333703, 0.3333333333333333703, 0.3333333333333333703, 0.3333333333333333703, 0.3333333333333333703, 0.3333333333333333703, 0.3333333333333333703, 0.3333333333333333703, 0.3333333333333333703, 0.3333333333333333703, 0.3333333333333333703, 0.3333333333333333703, 0.3333333333333333703, 0.3333333333333333703),
 ( 1.000000000000000000, 1.000000000000000000, 1.000000000000000000, 1.000000000000000000, 1.000000000000000000, 1.000000000000000000, 1.000000000000000000, 1.000000000000000000, 1.000000000000000000, 1.000000000000000000, 1.000000000000000000, 1.000000000000000000, 1.000000000000000000, 1.000000000000000000, 1.000000000000000000, 1.000000000000000000, 1.000000000000000000, 1.000000000000000000, 1.000000000000000000, 1.000000000000000000, 1.000000000000000000, 1.000000000000000000, 1.000000000000000000, 1.000000000000000000, 1.000000000000000000, 1.000000000000000000, 1.000000000000000000, 1.000000000000000000, 1.000000000000000000, 1.000000000000000000) ) ) 
 REPRESENTATION_ITEM ( '' )  SURFACE ( )  );
#13190 = CARTESIAN_POINT ( 'NONE',  ( 199.9999999999995737, -5.829854758272260185, 18.09651684827149865 ) ) ;
#13191 = CARTESIAN_POINT ( 'NONE',  ( -138.9613193423076325, 13.65853114841885407, -27.95779829447911169 ) ) ;
#13192 = CARTESIAN_POINT ( 'NONE',  ( 130.8568914410475088, -24.07718906446910623, 32.49135343045471558 ) ) ;
#13193 = CARTESIAN_POINT ( 'NONE',  ( -86.96347745069644475, -15.38646221621786125, -15.38646221621789856 ) ) ;
#13194 = CARTESIAN_POINT ( 'NONE',  ( 184.8905102610680444, 39.99999999999999289, 19.07866798485573057 ) ) ;
#13195 = CARTESIAN_POINT ( 'NONE',  ( 7.307793755307396388, -14.18010697691874711, 49.33439594495636982 ) ) ;
#13196 = DIRECTION ( 'NONE',  ( 0.9698969544411757404, 0.2249791741486417418, -0.09318942517865014263 ) ) ;
#13197 = AXIS2_PLACEMENT_3D ( 'NONE', #21328, #11204, #9589 ) ;
#13198 = CARTESIAN_POINT ( 'NONE',  ( 192.4448373802101173, -39.99999999999977973, -19.99999999996102673 ) ) ;
#13199 = CARTESIAN_POINT ( 'NONE',  ( -135.8532207217289738, 40.00000000000031974, -30.84685318188603986 ) ) ;
#13200 = LINE ( 'NONE', #21060, #19378 ) ;
#13201 = CARTESIAN_POINT ( 'NONE',  ( 170.2234770963711128, -10.92277846919171935, -45.64576402573189995 ) ) ;
#13202 = CARTESIAN_POINT ( 'NONE',  ( -200.0000000000000853, 24.32899771311817716, -44.86773131993646757 ) ) ;
#13203 = CARTESIAN_POINT ( 'NONE',  ( -193.3669111531647218, 18.32287347112285048, 44.23532963563830833 ) ) ;
#13204 = CARTESIAN_POINT ( 'NONE',  ( 130.8888609958234781, 29.49786752803534995, 12.21841679119730273 ) ) ;
#13205 = EDGE_CURVE ( 'NONE', #2384, #3446, #9381, .T. ) ;
#13206 = DIRECTION ( 'NONE',  ( 0.000000000000000000, 1.000000000000000000, 0.000000000000000000 ) ) ;
#13207 = CARTESIAN_POINT ( 'NONE',  ( -188.2995950289364941, -43.00522595870984333, 23.44932284465888728 ) ) ;
#13208 = CARTESIAN_POINT ( 'NONE',  ( -77.72621512577178748, 21.21705881579131514, -5.759696801490011175 ) ) ;
#13209 = CARTESIAN_POINT ( 'NONE',  ( -105.3755690713226585, -12.89780903124444578, 43.67073346367968156 ) ) ;
#13210 = DIRECTION ( 'NONE',  ( 0.000000000000000000, 0.000000000000000000, -1.000000000000000000 ) ) ;
#13211 = DIRECTION ( 'NONE',  ( 0.000000000000000000, -1.000000000000000000, 0.000000000000000000 ) ) ;
#13212 = ORIENTED_EDGE ( 'NONE', *, *, #12057, .F. ) ;
#13213 = CARTESIAN_POINT ( 'NONE',  ( -86.96347745069644475, 12.89780903124419353, -12.89780903124389333 ) ) ;
#13214 = EDGE_CURVE ( 'NONE', #3139, #19485, #19586, .T. ) ;
#13215 = CARTESIAN_POINT ( 'NONE',  ( 169.9999999999999432, 21.59613885783095810, -12.70659020859094568 ) ) ;
#13216 = EDGE_LOOP ( 'NONE', ( #13120, #11732, #22584, #18383, #598, #3072 ) ) ;
#13217 = CARTESIAN_POINT ( 'NONE',  ( -135.8532207217289738, -1.208299557080134822E-13, 9.153146818113572891 ) ) ;
#13218 = ADVANCED_FACE ( 'NONE', ( #24662 ), #22535, .F. ) ;
#13219 = CARTESIAN_POINT ( 'NONE',  ( 199.0199673144340409, -18.47600550957215759, -7.662649767945239887 ) ) ;
#13220 = ADVANCED_FACE ( 'NONE', ( #16534 ), #4439, .F. ) ;
#13221 = DIRECTION ( 'NONE',  ( 0.000000000000000000, 0.000000000000000000, 1.000000000000000000 ) ) ;
#13222 = AXIS2_PLACEMENT_3D ( 'NONE', #17985, #7876, #310 ) ;
#13223 = VERTEX_POINT ( 'NONE', #4709 ) ;
#13224 = ORIENTED_EDGE ( 'NONE', *, *, #19519, .T. ) ;
#13225 = CARTESIAN_POINT ( 'NONE',  ( -198.0356074513804572, 55.37879056873070027, 2.449293598294708485E-15 ) ) ;
#13226 = CARTESIAN_POINT ( 'NONE',  ( -99.31364972218659659, -20.79869444141380086, -8.164808577121105415 ) ) ;
#13227 = PRODUCT_DEFINITION_CONTEXT ( 'detailed design', #7971, 'design' ) ;
#13228 = DIRECTION ( 'NONE',  ( 0.000000000000000000, -1.000000000000000000, 0.000000000000000000 ) ) ;
#13229 = CARTESIAN_POINT ( 'NONE',  ( 151.7948205124836534, -39.99999999999987921, -33.23291073765567916 ) ) ;
#13230 = CARTESIAN_POINT ( 'NONE',  ( 199.9999999999997158, -17.84428681738966205, -6.548952533294360556 ) ) ;
#13231 = VECTOR ( 'NONE', #8130, 1000.000000000000000 ) ;
#13232 = CARTESIAN_POINT ( 'NONE',  ( -82.26522586992982156, 10.29063887125004939, 17.41030175917899214 ) ) ;
#13233 = AXIS2_PLACEMENT_3D ( 'NONE', #24450, #6088, #22460 ) ;
#13234 = CARTESIAN_POINT ( 'NONE',  ( 192.4448373802100889, -14.14213562375896061, 14.14213562375865330 ) ) ;
#13235 = CARTESIAN_POINT ( 'NONE',  ( -105.3755690713226585, 43.67073346367988051, -12.89780903124366418 ) ) ;
#13236 = CARTESIAN_POINT ( 'NONE',  ( 151.7948205124836534, -39.99999999999992184, -6.767089262349454515 ) ) ;
#13237 = CARTESIAN_POINT ( 'NONE',  ( -105.2054292635175585, -21.49321519473986442, -7.030298963786045751E-29 ) ) ;
#13238 = CARTESIAN_POINT ( 'NONE',  ( 192.4448373802101173, 20.00000000003945644, -40.00000000000002132 ) ) ;
#13239 = CARTESIAN_POINT ( 'NONE',  ( 192.4448373802101173, -42.42640687116490028, -14.14213562375904942 ) ) ;
#13240 = CARTESIAN_POINT ( 'NONE',  ( -105.3755690713226585, -18.24025645688353947, -40.00000000000002132 ) ) ;
#13242 = CARTESIAN_POINT ( 'NONE',  ( -86.96347745069645896, 40.00000000000008527, -21.75974354311636461 ) ) ;
#13241 = CARTESIAN_POINT ( 'NONE',  ( 23.09861257792924505, -42.94075326233385681, -23.40165480222905003 ) ) ;
#13243 = CARTESIAN_POINT ( 'NONE',  ( 57.59792236341147031, -2.435789363418150000, -40.00000000000002132 ) ) ;
#13244 = CARTESIAN_POINT ( 'NONE',  ( 192.4448373802101173, -14.14213562375886291, 42.42640687116498555 ) ) ;
#13245 = ADVANCED_FACE ( 'NONE', ( #10955 ), #20026, .T. ) ;
#13246 = CARTESIAN_POINT ( 'NONE',  ( -56.48582580120559982, 30.84685318188643777, -40.00000000000002132 ) ) ;
#13247 = VERTEX_POINT ( 'NONE', #20667 ) ;
#13248 = CARTESIAN_POINT ( 'NONE',  ( 19.94008347559386962, -47.92933869853446538, 13.96811062197253328 ) ) ;
#13249 = AXIS2_PLACEMENT_3D ( 'NONE', #6899, #6635, #15016 ) ;
#13250 = CARTESIAN_POINT ( 'NONE',  ( -105.2054292635176154, 15.67883240740060735, -14.71716402000391888 ) ) ;
#13251 = CARTESIAN_POINT ( 'NONE',  ( 136.1360204305621551, -24.77266263493126885, 31.79587985999256006 ) ) ;
#13252 = CARTESIAN_POINT ( 'NONE',  ( -86.96347745069643054, -39.99999999999995737, -21.75974354311664527 ) ) ;
#13253 = CARTESIAN_POINT ( 'NONE',  ( -77.64097821994924686, 21.67328794148362192, 4.107454262294036873 ) ) ;
#13254 = CARTESIAN_POINT ( 'NONE',  ( -70.30307074938296807, 10.20829450409786254, -22.52851052403980958 ) ) ;
#13255 = CARTESIAN_POINT ( 'NONE',  ( 199.9999999999998579, -2.486104477534099466, 18.84865669767346574 ) ) ;
#13256 = CARTESIAN_POINT ( 'NONE',  ( -628.0245654045285164, 26.47293912602897947, -29.98641569554063580 ) ) ;
#13257 = CARTESIAN_POINT ( 'NONE',  ( 190.0000000000001137, 3.490243377569959927E-14, 0.000000000000000000 ) ) ;
#13258 = CARTESIAN_POINT ( 'NONE',  ( 136.1360204305621551, 3.511608612530062512, 53.05693388239318864 ) ) ;
#13259 = CARTESIAN_POINT ( 'NONE',  ( 151.7948205124835681, 51.78348778862544322, -4.785054706298002891 ) ) ;
#13260 = CARTESIAN_POINT ( 'NONE',  ( -86.96347745069643054, 15.38646221621763210, 41.18208027870604582 ) ) ;
#13261 = DIRECTION ( 'NONE',  ( 1.053136113562458437E-14, 0.7071067811865507924, -0.7071067811865442421 ) ) ;
#13262 = CARTESIAN_POINT ( 'NONE',  ( -100.7734535825088500, 44.31723036834907958, -12.25131212657445801 ) ) ;
#13263 = VECTOR ( 'NONE', #2592, 1000.000000000000000 ) ;
#13265 = CARTESIAN_POINT ( 'NONE',  ( 0.2972598230769990524, -18.14793986248671231, -38.42060263243687501 ) ) ;
#13264 = CARTESIAN_POINT ( 'NONE',  ( 163.1118516004056573, 47.56205970284970164, -9.006482792073828847 ) ) ;
#13266 = CARTESIAN_POINT ( 'NONE',  ( 163.1118516004056573, 9.006482792069759213, -9.006482792069505194 ) ) ;
#13267 = CARTESIAN_POINT ( 'NONE',  ( -162.0762913951021176, 1.694272876828294194, -40.00000000000002132 ) ) ;
#13268 = CARTESIAN_POINT ( 'NONE',  ( 146.6084372240433993, -24.48358557860319706, -24.48358557860330720 ) ) ;
#13269 = CARTESIAN_POINT ( 'NONE',  ( -162.0762913951020892, -3.568845385355699554E-14, 1.694272876828323948 ) ) ;
#13270 = CARTESIAN_POINT ( 'NONE',  ( -30.26275506840324070, -29.48230279907817675, 27.08623969584564151 ) ) ;
#13271 = CARTESIAN_POINT ( 'NONE',  ( -183.6284948306513911, 41.87131864457176533, -17.34366805702960335 ) ) ;
#13272 = EDGE_LOOP ( 'NONE', ( #8139, #7895, #17082, #5614 ) ) ;
#13273 = CARTESIAN_POINT ( 'NONE',  ( 130.8568914410475088, 32.49135343045483637, -24.07718906446901030 ) ) ;
#13274 = CARTESIAN_POINT ( 'NONE',  ( -94.58366989427311466, -20.91926462023915079, -8.190486896679153972 ) ) ;
#13275 = CARTESIAN_POINT ( 'NONE',  ( 12.96694272570746698, 24.77464205076635295, 44.79869582452549537 ) ) ;
#13276 = CARTESIAN_POINT ( 'NONE',  ( -7.297127544325032744, -42.04314499753751022, -22.81351773421616258 ) ) ;
#13277 = ORIENTED_EDGE ( 'NONE', *, *, #7756, .F. ) ;
#13278 = CARTESIAN_POINT ( 'NONE',  ( -188.2506440019715797, -46.97351617221517017, 13.82466072834922244 ) ) ;
#13279 = CARTESIAN_POINT ( 'NONE',  ( 199.9999999999998863, -11.82502131081330887, -14.88093782183822888 ) ) ;
#13280 = CARTESIAN_POINT ( 'NONE',  ( 60.28378959949315430, -10.93033916072590372, 33.17072922783161459 ) ) ;
#13281 = CARTESIAN_POINT ( 'NONE',  ( 98.29820294267324243, 7.653668647304274764, -18.47759065023114999 ) ) ;
#13282 = CARTESIAN_POINT ( 'NONE',  ( 199.0061077845142279, 7.790749371913985755, -18.41559517569303495 ) ) ;
#13283 = EDGE_CURVE ( 'NONE', #9742, #24713, #580, .T. ) ;
#13284 = CARTESIAN_POINT ( 'NONE',  ( -77.78698619430412009, -6.810291944262315766, 20.89067062964120680 ) ) ;
#13285 = CARTESIAN_POINT ( 'NONE',  ( -91.56559293963834989, 6.234561990864368500E-14, -22.67402823373191723 ) ) ;
#13286 = CARTESIAN_POINT ( 'NONE',  ( -77.78738361196433004, -6.814606408068145882, 20.88860503098718979 ) ) ;
#13287 = CARTESIAN_POINT ( 'NONE',  ( -199.9999999999999716, -19.51623549979280980, -45.81998439131055534 ) ) ;
#13288 = CARTESIAN_POINT ( 'NONE',  ( -208.1127848780264742, -55.00245453014425578, -40.00000000000002132 ) ) ;
#13290 = DIRECTION ( 'NONE',  ( 1.000000000000000000, -1.836970198721030181E-16, -0.000000000000000000 ) ) ;
#13289 = CARTESIAN_POINT ( 'NONE',  ( 17.65190074000733844, -14.05440436230720636, -48.50354960736758159 ) ) ;
#13291 = CARTESIAN_POINT ( 'NONE',  ( -91.56559293963836410, 22.67402823373190301, 40.00000000000002132 ) ) ;
#13292 = CARTESIAN_POINT ( 'NONE',  ( 146.6084372240433993, 24.48358557860341733, -24.48358557860313311 ) ) ;
#13293 = CARTESIAN_POINT ( 'NONE',  ( 4.995406935893291767, 40.00000000000059686, -55.24977328853165659 ) ) ;
#13294 = CARTESIAN_POINT ( 'NONE',  ( 192.4448373802100889, 2.472897170449861688E-13, -19.99999999996060751 ) ) ;
#13295 = DIRECTION ( 'NONE',  ( 1.000000000000000000, 0.000000000000000000, 0.000000000000000000 ) ) ;
#13296 = EDGE_CURVE ( 'NONE', #15169, #18548, #3042, .T. ) ;
#13297 = ORIENTED_EDGE ( 'NONE', *, *, #22659, .T. ) ;
#13299 = CARTESIAN_POINT ( 'NONE',  ( 16.10036699868000554, 44.47262139758795030, -24.53427828610321271 ) ) ;
#13298 = DIRECTION ( 'NONE',  ( 1.000000000000000000, 1.836970198721030427E-16, -0.000000000000000000 ) ) ;
#13300 = CARTESIAN_POINT ( 'NONE',  ( -91.56559293963834989, -17.32597176626812896, 40.00000000000002132 ) ) ;
#13301 = EDGE_CURVE ( 'NONE', #9028, #14209, #6021, .T. ) ;
#13302 = SURFACE_STYLE_FILL_AREA ( #3194 ) ;
#13303 = CARTESIAN_POINT ( 'NONE',  ( -197.6434631109478346, 44.74794079767860921, -18.53520396667194703 ) ) ;
#13304 = DIRECTION ( 'NONE',  ( 1.000000000000000000, 1.836970198721010952E-16, -1.836970198721030181E-16 ) ) ;
#13305 = VERTEX_POINT ( 'NONE', #12945 ) ;
#13306 = ORIENTED_EDGE ( 'NONE', *, *, #3876, .T. ) ;
#13307 = CARTESIAN_POINT ( 'NONE',  ( -198.0356074513804572, -10.87444709759729911, 10.87444709759714812 ) ) ;
#13308 = DIRECTION ( 'NONE',  ( 0.000000000000000000, -1.000000000000000000, 0.000000000000000000 ) ) ;
#13309 = ORIENTED_EDGE ( 'NONE', *, *, #17423, .T. ) ;
#13310 = ORIENTED_EDGE ( 'NONE', *, *, #13921, .F. ) ;
#13311 = CARTESIAN_POINT ( 'NONE',  ( 199.9999999999998579, -2.486104477534099466, 18.84865669767346574 ) ) ;
#13312 = CARTESIAN_POINT ( 'NONE',  ( -190.0000000000000000, 66.50000000000009948, -66.50000000000005684 ) ) ;
#13313 = CARTESIAN_POINT ( 'NONE',  ( -56.48582580120559271, 21.81201906317768291, 21.81201906317777173 ) ) ;
#13314 = CARTESIAN_POINT ( 'NONE',  ( -121.8425463770985573, -22.74408395592868004, -9.420908036270656538 ) ) ;
#13315 = CARTESIAN_POINT ( 'NONE',  ( -259.2033419157646676, -40.00000000000003553, -9.517827891722768996 ) ) ;
#13316 = CARTESIAN_POINT ( 'NONE',  ( -189.2428623074475524, -23.64699222226070674, 43.27185639470918233 ) ) ;
#13317 = CARTESIAN_POINT ( 'NONE',  ( 190.0000000000000000, -66.50000000000001421, -66.50000000000005684 ) ) ;
#13318 = CARTESIAN_POINT ( 'NONE',  ( 170.2234770963711128, -39.99999999999982947, -15.44714144992858529 ) ) ;
#13319 = CARTESIAN_POINT ( 'NONE',  ( 146.6084372240433709, 40.00000000000010658, -5.374981219216549810 ) ) ;
#13320 = CARTESIAN_POINT ( 'NONE',  ( -86.93850585862767844, 19.24776704638164659, 9.367985447339783889 ) ) ;
#13321 = CARTESIAN_POINT ( 'NONE',  ( 4.995406935893293543, -10.78321810389005364, 10.78321810388994173 ) ) ;
#13322 = CARTESIAN_POINT ( 'NONE',  ( -135.8532207217289738, 7.002209520526292428E-15, -9.153146818113572891 ) ) ;
#13323 = CARTESIAN_POINT ( 'NONE',  ( -192.6562840316549341, 18.27409180090459628, 44.11756026579762846 ) ) ;
#13324 = CARTESIAN_POINT ( 'NONE',  ( 125.5832160019860737, 28.05309928653993978, 11.61997419108395846 ) ) ;
#13325 = DIRECTION ( 'NONE',  ( -1.000000000000000000, -1.836970198721030181E-16, -0.000000000000000000 ) ) ;
#13326 = CARTESIAN_POINT ( 'NONE',  ( 130.8568914410475088, 52.36146031193420924, 4.207082182989907437 ) ) ;
#13327 = CARTESIAN_POINT ( 'NONE',  ( -87.11138134867678673, -17.02212146154200312, 13.16760794720353189 ) ) ;
#13328 = CARTESIAN_POINT ( 'NONE',  ( -86.96347745069644475, -43.67073346367983788, 12.89780903124397149 ) ) ;
#13329 = CARTESIAN_POINT ( 'NONE',  ( 4.995406935893305977, -39.06748935135157552, -39.06748935135225764 ) ) ;
#13330 = FACE_OUTER_BOUND ( 'NONE', #19546, .T. ) ;
#13331 = CARTESIAN_POINT ( 'NONE',  ( -105.4741150117390021, -7.943527260764932763, -19.77569912954469800 ) ) ;
#13332 = VERTEX_POINT ( 'NONE', #21061 ) ;
#13333 = CARTESIAN_POINT ( 'NONE',  ( 14.38125909742181463, 10.73282306403652875, -67.30136555895941797 ) ) ;
#13334 = LINE ( 'NONE', #3107, #97 ) ;
#13335 =( BOUNDED_SURFACE ( )  B_SPLINE_SURFACE ( 3, 3, ( 
 ( #18505, #286, #24642, #6398, #18641, #22646, #16646, #4420, #22093, #18352, #24354, #20225, #14362, #2003, #10109, #25959, #132, #1734, #8236, #20093, #5716, #22226, #4142, #7702, #16354, #21955, #10241, #3729, #3213, #24487 ),
 ( #18210, #8104, #16225, #9843, #15948, #4002, #12101, #9708, #1872, #24217, #11969, #13959, #15813, #13821, #20358, #6249, #17813, #14097, #24079, #18083, #23939, #2133, #6118, #4271, #9975, #26234, #22492, #14226, #11832, #7968 ),
 ( #22365, #17947, #12359, #16087, #12234, #5988, #20490, #19950, #26094, #5853, #3867, #7830, #22751, #15017, #2263, #8771, #6636, #18481, #14750, #8371, #20887, #18750, #16748, #22623, #6372, #262, #14882, #4530, #533, #20755 ),
 ( #24880, #25016, #402, #12898, #4659, #23147, #2525, #12628, #25149, #22881, #16493, #10642, #8638, #12762, #2666, #20617, #17012, #10771, #23021, #18884, #662, #4398, #24618, #16619, #24752, #8902, #16885, #4919, #10371, #6770 ),
 ( #6506, #13032, #14616, #4797, #21013, #18619, #14490, #2795, #6900, #12492, #10907, #19019, #798, #2393, #10505, #8505, #19623, #1408, #11902, #9908, #11495, #7903, #21883, #3798, #5786, #21752, #19886, #17879, #927, #7507 ),
 ( #11033, #13627, #25759, #25276, #5923, #9509, #3526, #15617, #7026, #17747, #23740, #13157, #16022, #19143, #5521, #21150, #5650, #21277, #17614, #11627, #19749, #1539, #9037, #17142, #15145, #26028, #23275, #24147, #9644, #25889 ),
 ( #20027, #3397, #1805, #7631, #5051, #15745, #15878, #23874, #18014, #13755, #22027, #3660, #11768, #26162, #1670, #9778, #2924, #7765, #24006, #13893, #1937, #14031, #24290, #14429, #6182, #6310, #10313, #10178, #18556, #22559 ) ),
 .UNSPECIFIED., .T., .F., .F. ) 
 B_SPLINE_SURFACE_WITH_KNOTS ( ( 4, 3, 4 ),
 ( 4, 2, 2, 2, 2, 2, 2, 2, 2, 2, 2, 2, 2, 2, 4 ),
 ( 0.000000000000000000, 0.5000000000000000000, 1.000000000000000000 ),
 ( 0.000000000000000000, 0.1357259735107005372, 0.1651108541090157700, 0.1944957347073310028, 0.3598804999793158710, 0.3867117631979620773, 0.4135430264166082281, 0.5789277916885930964, 0.6062785021374117456, 0.6336292125862302838, 0.8508620842112317728, 0.8814014469398914198, 0.9119408096685510667, 0.9559704048342755334, 1.000000000000000000 ),
 .UNSPECIFIED. ) 
 GEOMETRIC_REPRESENTATION_ITEM ( )  RATIONAL_B_SPLINE_SURFACE ( (
 ( 1.000000000000000000, 1.000000000000000000, 1.000000000000000000, 1.000000000000000000, 1.000000000000000000, 1.000000000000000000, 1.000000000000000000, 1.000000000000000000, 1.000000000000000000, 1.000000000000000000, 1.000000000000000000, 1.000000000000000000, 1.000000000000000000, 1.000000000000000000, 1.000000000000000000, 1.000000000000000000, 1.000000000000000000, 1.000000000000000000, 1.000000000000000000, 1.000000000000000000, 1.000000000000000000, 1.000000000000000000, 1.000000000000000000, 1.000000000000000000, 1.000000000000000000, 1.000000000000000000, 1.000000000000000000, 1.000000000000000000, 1.000000000000000000, 1.000000000000000000),
 ( 0.3333333333333333703, 0.3333333333333333703, 0.3333333333333333703, 0.3333333333333333703, 0.3333333333333333703, 0.3333333333333333703, 0.3333333333333333703, 0.3333333333333333703, 0.3333333333333333703, 0.3333333333333333703, 0.3333333333333333703, 0.3333333333333333703, 0.3333333333333333703, 0.3333333333333333703, 0.3333333333333333703, 0.3333333333333333703, 0.3333333333333333703, 0.3333333333333333703, 0.3333333333333333703, 0.3333333333333333703, 0.3333333333333333703, 0.3333333333333333703, 0.3333333333333333703, 0.3333333333333333703, 0.3333333333333333703, 0.3333333333333333703, 0.3333333333333333703, 0.3333333333333333703, 0.3333333333333333703, 0.3333333333333333703),
 ( 0.3333333333333333703, 0.3333333333333333703, 0.3333333333333333703, 0.3333333333333333703, 0.3333333333333333703, 0.3333333333333333703, 0.3333333333333333703, 0.3333333333333333703, 0.3333333333333333703, 0.3333333333333333703, 0.3333333333333333703, 0.3333333333333333703, 0.3333333333333333703, 0.3333333333333333703, 0.3333333333333333703, 0.3333333333333333703, 0.3333333333333333703, 0.3333333333333333703, 0.3333333333333333703, 0.3333333333333333703, 0.3333333333333333703, 0.3333333333333333703, 0.3333333333333333703, 0.3333333333333333703, 0.3333333333333333703, 0.3333333333333333703, 0.3333333333333333703, 0.3333333333333333703, 0.3333333333333333703, 0.3333333333333333703),
 ( 1.000000000000000000, 1.000000000000000000, 1.000000000000000000, 1.000000000000000000, 1.000000000000000000, 1.000000000000000000, 1.000000000000000000, 1.000000000000000000, 1.000000000000000000, 1.000000000000000000, 1.000000000000000000, 1.000000000000000000, 1.000000000000000000, 1.000000000000000000, 1.000000000000000000, 1.000000000000000000, 1.000000000000000000, 1.000000000000000000, 1.000000000000000000, 1.000000000000000000, 1.000000000000000000, 1.000000000000000000, 1.000000000000000000, 1.000000000000000000, 1.000000000000000000, 1.000000000000000000, 1.000000000000000000, 1.000000000000000000, 1.000000000000000000, 1.000000000000000000),
 ( 0.3333333333333333703, 0.3333333333333333703, 0.3333333333333333703, 0.3333333333333333703, 0.3333333333333333703, 0.3333333333333333703, 0.3333333333333333703, 0.3333333333333333703, 0.3333333333333333703, 0.3333333333333333703, 0.3333333333333333703, 0.3333333333333333703, 0.3333333333333333703, 0.3333333333333333703, 0.3333333333333333703, 0.3333333333333333703, 0.3333333333333333703, 0.3333333333333333703, 0.3333333333333333703, 0.3333333333333333703, 0.3333333333333333703, 0.3333333333333333703, 0.3333333333333333703, 0.3333333333333333703, 0.3333333333333333703, 0.3333333333333333703, 0.3333333333333333703, 0.3333333333333333703, 0.3333333333333333703, 0.3333333333333333703),
 ( 0.3333333333333333703, 0.3333333333333333703, 0.3333333333333333703, 0.3333333333333333703, 0.3333333333333333703, 0.3333333333333333703, 0.3333333333333333703, 0.3333333333333333703, 0.3333333333333333703, 0.3333333333333333703, 0.3333333333333333703, 0.3333333333333333703, 0.3333333333333333703, 0.3333333333333333703, 0.3333333333333333703, 0.3333333333333333703, 0.3333333333333333703, 0.3333333333333333703, 0.3333333333333333703, 0.3333333333333333703, 0.3333333333333333703, 0.3333333333333333703, 0.3333333333333333703, 0.3333333333333333703, 0.3333333333333333703, 0.3333333333333333703, 0.3333333333333333703, 0.3333333333333333703, 0.3333333333333333703, 0.3333333333333333703),
 ( 1.000000000000000000, 1.000000000000000000, 1.000000000000000000, 1.000000000000000000, 1.000000000000000000, 1.000000000000000000, 1.000000000000000000, 1.000000000000000000, 1.000000000000000000, 1.000000000000000000, 1.000000000000000000, 1.000000000000000000, 1.000000000000000000, 1.000000000000000000, 1.000000000000000000, 1.000000000000000000, 1.000000000000000000, 1.000000000000000000, 1.000000000000000000, 1.000000000000000000, 1.000000000000000000, 1.000000000000000000, 1.000000000000000000, 1.000000000000000000, 1.000000000000000000, 1.000000000000000000, 1.000000000000000000, 1.000000000000000000, 1.000000000000000000, 1.000000000000000000) ) ) 
 REPRESENTATION_ITEM ( '' )  SURFACE ( )  );
#13336 = CARTESIAN_POINT ( 'NONE',  ( -575.0231298121466352, 75.00000000000000000, -30.00000000000202505 ) ) ;
#13337 = VERTEX_POINT ( 'NONE', #14537 ) ;
#13338 = CARTESIAN_POINT ( 'NONE',  ( 190.0000000000000284, -125.7889608577475400, 82.50000000000001421 ) ) ;
#13339 = CARTESIAN_POINT ( 'NONE',  ( 199.0197737566289504, -18.32000334048170487, -8.029774482221071707 ) ) ;
#13340 = CARTESIAN_POINT ( 'NONE',  ( -4.039451493210483690, -43.00522595894025812, 23.44932283416647323 ) ) ;
#13341 = ORIENTED_EDGE ( 'NONE', *, *, #16052, .F. ) ;
#13342 = ORIENTED_EDGE ( 'NONE', *, *, #3013, .F. ) ;
#13343 = CARTESIAN_POINT ( 'NONE',  ( -198.0356074513804572, -39.15871834505905724, -17.40982414986491733 ) ) ;
#13344 = CARTESIAN_POINT ( 'NONE',  ( 130.8568914410475088, 40.00000000000015632, -34.05028731879774284 ) ) ;
#13345 = FACE_OUTER_BOUND ( 'NONE', #25687, .T. ) ;
#13346 = ADVANCED_FACE ( 'NONE', ( #20802 ), #6943, .F. ) ;
#13347 = CARTESIAN_POINT ( 'NONE',  ( 210.0000000000000284, 66.50000000000009948, -66.50000000000005684 ) ) ;
#13348 = CARTESIAN_POINT ( 'NONE',  ( -162.0762913951020892, -3.568845385355699554E-14, 1.694272876828323948 ) ) ;
#13349 = CARTESIAN_POINT ( 'NONE',  ( 200.0000000000000284, -19.00889450552964988, -0.1561390237190347086 ) ) ;
#13350 = CARTESIAN_POINT ( 'NONE',  ( -87.13361725327074225, 15.19799821270826179, 15.19799821270854245 ) ) ;
#13351 = CARTESIAN_POINT ( 'NONE',  ( -6.342283169554272959, -13.66521761902986754, -46.19215417243526645 ) ) ;
#13352 = CARTESIAN_POINT ( 'NONE',  ( 57.59792236341148453, 1.722363176415528940, -54.84617931850878136 ) ) ;
#13353 = CARTESIAN_POINT ( 'NONE',  ( -105.2502153031284422, -21.20171025720616953, 3.401878988847722329 ) ) ;
#13354 = CARTESIAN_POINT ( 'NONE',  ( -208.1127848780264742, -39.99999999999948841, -55.00245453010965235 ) ) ;
#13355 = CARTESIAN_POINT ( 'NONE',  ( 35.93702929138175506, 12.87541766509833785, 42.26928858764885177 ) ) ;
#13356 = CARTESIAN_POINT ( 'NONE',  ( 57.59792236341148453, -37.56421063658185489, 40.00000000000002132 ) ) ;
#13357 = CARTESIAN_POINT ( 'NONE',  ( -238.4067589809705794, -40.96449427990185654, -40.00000000000002132 ) ) ;
#13358 = CARTESIAN_POINT ( 'NONE',  ( -105.3755690713226585, 43.67073346367970288, 12.89780903124427702 ) ) ;
#13359 = CARTESIAN_POINT ( 'NONE',  ( 146.6084372240433993, 34.62501878078308692, 0.000000000000000000 ) ) ;
#13361 = CARTESIAN_POINT ( 'NONE',  ( 163.1118516004056573, 40.00000000000014921, -27.26290988616858968 ) ) ;
#13360 = DIRECTION ( 'NONE',  ( 0.000000000000000000, 1.000000000000000000, 0.000000000000000000 ) ) ;
#13362 = CARTESIAN_POINT ( 'NONE',  ( 150.0000000000000284, -135.7889608577475258, 82.50000000000001421 ) ) ;
#13363 = CARTESIAN_POINT ( 'NONE',  ( 136.1360204305621551, 31.79587985999267374, -24.77266263493117293 ) ) ;
#13364 = CARTESIAN_POINT ( 'NONE',  ( 184.8905102610680444, 19.07866798485561333, 40.00000000000002132 ) ) ;
#13365 = ORIENTED_EDGE ( 'NONE', *, *, #21024, .T. ) ;
#13366 = CARTESIAN_POINT ( 'NONE',  ( 22.77497178454860816, -43.17449153292918851, 17.88345994150142815 ) ) ;
#13367 = CARTESIAN_POINT ( 'NONE',  ( -105.2054292635175869, 15.19799821370233062, -15.19799821370219206 ) ) ;
#13368 = EDGE_CURVE ( 'NONE', #433, #17301, #14073, .T. ) ;
#13369 = CARTESIAN_POINT ( 'NONE',  ( -86.96347745069644475, 12.89780903124401057, 12.89780903124407629 ) ) ;
#13370 = CARTESIAN_POINT ( 'NONE',  ( -259.2033419157646676, -40.00000000000003553, -9.517827891722768996 ) ) ;
#13371 = CARTESIAN_POINT ( 'NONE',  ( -87.04641387366682181, 20.92787283706964985, -4.638221027435098343 ) ) ;
#13372 = DIRECTION ( 'NONE',  ( 1.000000000000000000, -0.000000000000000000, -0.000000000000000000 ) ) ;
#13373 = CARTESIAN_POINT ( 'NONE',  ( 199.9999999999995737, -5.829854758272260185, 18.09651684827149865 ) ) ;
#13374 = EDGE_CURVE ( 'NONE', #11522, #16316, #11098, .T. ) ;
#13375 = CARTESIAN_POINT ( 'NONE',  ( -82.23726319249649919, -20.19517362732916510, -9.977985540125270190E-16 ) ) ;
#13376 = ADVANCED_FACE ( 'NONE', ( #16796 ), #24933, .T. ) ;
#13377 = CARTESIAN_POINT ( 'NONE',  ( -87.12812962371036463, 1.358531488422078937, -21.45735542732301226 ) ) ;
#13378 = CARTESIAN_POINT ( 'NONE',  ( 184.8905102610680444, -14.79361573936399665, 14.79361573936367158 ) ) ;
#13379 = CARTESIAN_POINT ( 'NONE',  ( -213.1075012329536946, -37.98287015391210275, -37.98287015391272092 ) ) ;
#13380 = CARTESIAN_POINT ( 'NONE',  ( 14.38125909742181996, -10.73282306403606157, 67.30136555895948902 ) ) ;
#13381 = LINE ( 'NONE', #17622, #20620 ) ;
#13382 = CARTESIAN_POINT ( 'NONE',  ( -213.1075012329536946, -37.98287015391210275, -37.98287015391272092 ) ) ;
#13384 = CARTESIAN_POINT ( 'NONE',  ( -238.4067589809705794, -27.60227080167029001, -28.96627169325357798 ) ) ;
#13383 = CARTESIAN_POINT ( 'NONE',  ( -105.3755690713226585, 15.38646221621820764, -41.18208027870583265 ) ) ;
#13385 = CARTESIAN_POINT ( 'NONE',  ( -135.8532207217289738, -6.472252184283586729, -50.09629031063973770 ) ) ;
#13386 = CARTESIAN_POINT ( 'NONE',  ( -716.9846540392142060, 82.50000000000008527, -52.49999999999977973 ) ) ;
#13387 = FACE_BOUND ( 'NONE', #23050, .T. ) ;
#13388 = CARTESIAN_POINT ( 'NONE',  ( 0.2972598230769957217, -4.999556039334937811E-14, 14.33493731733933352 ) ) ;
#13389 = CIRCLE ( 'NONE', #15504, 30.00000000000000355 ) ;
#13390 = CARTESIAN_POINT ( 'NONE',  ( 184.8905102610680444, -13.49065550809840630, 43.07788698682565354 ) ) ;
#13391 = CONICAL_SURFACE ( 'NONE', #17213, 60.00000000000009948, 0.7853981633974479459 ) ;
#13392 = CARTESIAN_POINT ( 'NONE',  ( 57.59792236341147031, 37.56421063658187620, 40.00000000000002132 ) ) ;
#13393 = ORIENTED_EDGE ( 'NONE', *, *, #3363, .F. ) ;
#13394 = CARTESIAN_POINT ( 'NONE',  ( -56.48582580120559982, 21.81201906317778594, -34.75652343174606074 ) ) ;
#13395 = CARTESIAN_POINT ( 'NONE',  ( -86.86493150571111244, -19.60045294882784717, -8.366608963953344968 ) ) ;
#13396 = CARTESIAN_POINT ( 'NONE',  ( 36.66494225440861499, 16.22659705908689531, 39.17447069130953707 ) ) ;
#13397 = CARTESIAN_POINT ( 'NONE',  ( -210.0000000000000284, 52.50000000000007816, 52.49999999999999289 ) ) ;
#13398 = EDGE_LOOP ( 'NONE', ( #18114, #16420, #15804, #18378 ) ) ;
#13399 = CARTESIAN_POINT ( 'NONE',  ( -188.8753211508388006, -43.29880796194907333, 17.93495349242729375 ) ) ;
#13400 = PRODUCT_DEFINITION_FORMATION_WITH_SPECIFIED_SOURCE ( 'ANY', '', #13756, .NOT_KNOWN. ) ;
#13401 = CARTESIAN_POINT ( 'NONE',  ( 200.0000000000000284, -15.63511319855579629, -10.80754414709790190 ) ) ;
#13402 = CARTESIAN_POINT ( 'NONE',  ( 25.31597067608044682, -17.58652183057975193, 42.45761951829265968 ) ) ;
#13403 = CARTESIAN_POINT ( 'NONE',  ( 98.29820294268672853, 20.00000000000089528, 2.652164898395847903 ) ) ;
#13404 = CARTESIAN_POINT ( 'NONE',  ( 199.0056860580130262, 9.997888132351027579, -17.31887563448481160 ) ) ;
#13405 = CIRCLE ( 'NONE', #22779, 28.79780246617542616 ) ;
#13406 = VECTOR ( 'NONE', #7913, 1000.000000000000000 ) ;
#13407 = DIRECTION ( 'NONE',  ( 0.000000000000000000, 1.000000000000000000, 0.000000000000000000 ) ) ;
#13408 = CARTESIAN_POINT ( 'NONE',  ( -56.48582580120560692, 40.00000000000004263, -9.153146818113443217 ) ) ;
#13409 = CARTESIAN_POINT ( 'NONE',  ( -77.70092821061149380, -5.501796661956294798, 21.35074465833452706 ) ) ;
#13410 = CARTESIAN_POINT ( 'NONE',  ( 17.75917311731580384, 48.46615948699212595, -14.04884443869896593 ) ) ;
#13411 = CARTESIAN_POINT ( 'NONE',  ( 200.0000000000000000, -19.99999999999989342, 40.00000000000002132 ) ) ;
#13413 = CARTESIAN_POINT ( 'NONE',  ( -215.0000000000000284, 69.29737539576900929, -75.30386416458597409 ) ) ;
#13412 = CARTESIAN_POINT ( 'NONE',  ( -114.4364955367321528, 8.644468109209284989, -20.04994829327632999 ) ) ;
#13414 = CARTESIAN_POINT ( 'NONE',  ( -100.7734535825088500, -17.32597176626813251, 40.00000000000002132 ) ) ;
#13416 = CARTESIAN_POINT ( 'NONE',  ( 199.9999999999999432, 14.14213562373113398, -14.14213562373094923 ) ) ;
#13415 = AXIS2_PLACEMENT_3D ( 'NONE', #14032, #5522, #22028 ) ;
#13417 = AXIS2_PLACEMENT_3D ( 'NONE', #14280, #1791, #24404 ) ;
#13418 = CARTESIAN_POINT ( 'NONE',  ( -162.0762913951021176, 40.00000000000042633, -41.69427287672947102 ) ) ;
#13419 = CARTESIAN_POINT ( 'NONE',  ( -213.1075012329537230, -39.99999999999991473, -13.71589010951953647 ) ) ;
#13420 = CARTESIAN_POINT ( 'NONE',  ( 101.9643209985650003, -19.81985618488135259, -8.209653236061971171 ) ) ;
#13421 = ORIENTED_EDGE ( 'NONE', *, *, #16396, .T. ) ;
#13423 = CARTESIAN_POINT ( 'NONE',  ( -4.004886986944939942, 47.00296421444957673, -13.82996668233321458 ) ) ;
#13422 = CARTESIAN_POINT ( 'NONE',  ( -16.41532015121172350, -42.70629200808449610, 12.95569205125167578 ) ) ;
#13424 = CARTESIAN_POINT ( 'NONE',  ( -135.8532207217289454, -30.84685318188649106, 40.00000000000002132 ) ) ;
#13425 = CARTESIAN_POINT ( 'NONE',  ( -162.0762913951020892, 1.198031840385732849, -1.198031840385733515 ) ) ;
#13426 = CARTESIAN_POINT ( 'NONE',  ( -114.7826396787322665, 2.171560191748074081E-13, -22.13135001986799111 ) ) ;
#13427 = DIRECTION ( 'NONE',  ( 0.000000000000000000, 0.000000000000000000, 1.000000000000000000 ) ) ;
#13428 = ORIENTED_EDGE ( 'NONE', *, *, #16108, .T. ) ;
#13429 = VERTEX_POINT ( 'NONE', #23191 ) ;
#13430 = CARTESIAN_POINT ( 'NONE',  ( -102.4068193528169246, -20.17396017424864141, 8.735227608996771309 ) ) ;
#13431 = CARTESIAN_POINT ( 'NONE',  ( 98.29820294273291381, -18.47759065023123526, -7.653668647304108674 ) ) ;
#13432 = CARTESIAN_POINT ( 'NONE',  ( -86.86493150571111244, 7.943527260496201947, -19.77569912839169319 ) ) ;
#13433 = VERTEX_POINT ( 'NONE', #10819 ) ;
#13434 = CARTESIAN_POINT ( 'NONE',  ( 199.0262772983307400, -15.97594543884460450, 12.04151787815577102 ) ) ;
#13435 = DIRECTION ( 'NONE',  ( 0.000000000000000000, 0.000000000000000000, 1.000000000000000000 ) ) ;
#13436 = VECTOR ( 'NONE', #16055, 1000.000000000000000 ) ;
#13437 = CARTESIAN_POINT ( 'NONE',  ( -238.4067589809705794, 28.96627169325315165, 28.96627169325329731 ) ) ;
#13438 = CARTESIAN_POINT ( 'NONE',  ( -678.9461782662772293, 75.00000000000000000, 25.00000000000157385 ) ) ;
#13439 = VECTOR ( 'NONE', #1880, 1000.000000000000000 ) ;
#13440 = CARTESIAN_POINT ( 'NONE',  ( -192.9588430854689989, -8.596193650988133061E-14, 14.46834944099969533 ) ) ;
#13441 = CARTESIAN_POINT ( 'NONE',  ( -105.4741150117383341, -8.366608964593364561, -19.60045294982747777 ) ) ;
#13442 = CARTESIAN_POINT ( 'NONE',  ( -199.9999999999999147, -49.28189405767606956, -14.17215463606684267 ) ) ;
#13443 = DIRECTION ( 'NONE',  ( 1.000000000000000000, -1.937599346585394162E-16, -0.000000000000000000 ) ) ;
#13444 = EDGE_CURVE ( 'NONE', #10703, #14209, #6682, .T. ) ;
#13445 = CARTESIAN_POINT ( 'NONE',  ( -86.96347745069643054, -39.99999999999985079, -18.24025645688394448 ) ) ;
#13446 = CARTESIAN_POINT ( 'NONE',  ( 4.995406935893291767, 40.00000000000059686, -55.24977328853165659 ) ) ;
#13447 = CARTESIAN_POINT ( 'NONE',  ( -87.13361725327069962, 15.19799821270825113, 15.19799821270852824 ) ) ;
#13448 = B_SPLINE_CURVE_WITH_KNOTS ( 'NONE', 3,
 ( #11361, #3134, #19610, #19478, #13612, #1656, #25490, #11482, #1265, #21610, #25620, #21740, #3516, #7239, #5384, #13489, #15864, #3384, #17355, #19874, #9497, #17602, #25744, #13241, #7493, #11236, #9765 ),
 .UNSPECIFIED., .F., .F.,
 ( 4, 2, 1, 1, 2, 2, 2, 2, 2, 2, 2, 2, 1, 2, 4 ),
 ( -5.999999998738660203E-08, 0.0002171475752860161713, 0.0004343551505720197347, 0.0008687703011440245848, 0.001737600602288039055, 0.003475261204576066479, 0.006950582409152118724, 0.01390122481830422495, 0.02085186722745633117, 0.02432718843203238862, 0.02606484903432041561, 0.02693367933546442911, 0.02736809448603644279, 0.02758530206132244963, 0.02780250963660845301 ),
 .UNSPECIFIED. ) ;
#13449 = CARTESIAN_POINT ( 'NONE',  ( 4.995406935893297984, -39.06748935135182421, -17.50105314357212549 ) ) ;
#13450 = CARTESIAN_POINT ( 'NONE',  ( 57.59792236341147031, 1.908507979671054758E-14, -2.435789363418160658 ) ) ;
#13451 = CARTESIAN_POINT ( 'NONE',  ( -100.7734535825088500, 16.03295912088713848, -16.03295912088698927 ) ) ;
#13452 = DIRECTION ( 'NONE',  ( 0.01051738792038098801, -0.9307051272723525503, -0.3656191332798196525 ) ) ;
#13453 = FACE_OUTER_BOUND ( 'NONE', #24480, .T. ) ;
#13454 = CARTESIAN_POINT ( 'NONE',  ( 151.7948205124835681, 51.78348778862537927, 4.785054706298732086 ) ) ;
#13455 = CARTESIAN_POINT ( 'NONE',  ( 192.4448373802100889, 1.051811698935164031E-13, -20.00000000003942091 ) ) ;
#13456 = CARTESIAN_POINT ( 'NONE',  ( -91.56559293963834989, -16.03295912088716335, 40.53558337403673306 ) ) ;
#13457 = CARTESIAN_POINT ( 'NONE',  ( -198.0356074513804572, -67.44298959253333692, -10.87444709761016348 ) ) ;
#13458 = CARTESIAN_POINT ( 'NONE',  ( -655.1879134060876595, 39.94028867827254459, -20.75640583205202816 ) ) ;
#13459 = CARTESIAN_POINT ( 'NONE',  ( 107.5473083967386572, -2.315402722108309326E-13, 23.99138244111235352 ) ) ;
#13460 = ORIENTED_EDGE ( 'NONE', *, *, #7406, .F. ) ;
#13461 = CARTESIAN_POINT ( 'NONE',  ( -56.48582580120559982, -6.472252184283581400, -50.09629031063973059 ) ) ;
#13462 = VECTOR ( 'NONE', #19415, 1000.000000000000000 ) ;
#13463 = CARTESIAN_POINT ( 'NONE',  ( 170.0000000000000284, 6.285860131565048192, 24.25569233607182440 ) ) ;
#13464 = ORIENTED_EDGE ( 'NONE', *, *, #11193, .F. ) ;
#13465 = CARTESIAN_POINT ( 'NONE',  ( 170.2234770963711128, -40.00000000000024158, 24.55285855007145202 ) ) ;
#13466 = CARTESIAN_POINT ( 'NONE',  ( 199.0258541015842866, -17.97331862618372611, 8.883049498760815510 ) ) ;
#13467 = DIRECTION ( 'NONE',  ( 0.000000000000000000, 0.000000000000000000, -1.000000000000000000 ) ) ;
#13468 = ORIENTED_EDGE ( 'NONE', *, *, #18340, .F. ) ;
#13469 = EDGE_LOOP ( 'NONE', ( #21940, #12509, #10802, #18954 ) ) ;
#13470 = CARTESIAN_POINT ( 'NONE',  ( -100.7734535825088500, -12.25131212657462498, -44.31723036834905827 ) ) ;
#13471 = CARTESIAN_POINT ( 'NONE',  ( 199.9999999999999432, -3.553951640073651008E-14, 19.99999999999992539 ) ) ;
#13472 = ADVANCED_FACE ( 'NONE', ( #2966 ), #8818, .T. ) ;
#13473 = CARTESIAN_POINT ( 'NONE',  ( -109.1264249741460048, 33.12752917269234132, -13.72187187123960150 ) ) ;
#13474 = DIRECTION ( 'NONE',  ( 0.000000000000000000, 1.000000000000000000, 0.000000000000000000 ) ) ;
#13475 = CARTESIAN_POINT ( 'NONE',  ( -259.2033419157646676, -40.00000000000017764, 30.48217210827725054 ) ) ;
#13476 = CARTESIAN_POINT ( 'NONE',  ( 200.0000000000000284, -17.94985894478863386, -6.254032569489808679 ) ) ;
#13477 = CARTESIAN_POINT ( 'NONE',  ( -135.8532207217289738, 40.00000000000002842, -9.153146818113432559 ) ) ;
#13478 = DIRECTION ( 'NONE',  ( 0.000000000000000000, -1.000000000000000000, 0.000000000000000000 ) ) ;
#13479 = CARTESIAN_POINT ( 'NONE',  ( -8.720657192081592513, -22.53512351407530190, -41.62108041047272167 ) ) ;
#13480 = CARTESIAN_POINT ( 'NONE',  ( 130.8568914410475088, 52.36146031193427319, -4.207082182989173802 ) ) ;
#13481 =( BOUNDED_CURVE ( )  B_SPLINE_CURVE ( 3, ( #17952, #21960, #11837, #26099 ),
 .UNSPECIFIED., .F., .F. ) 
 B_SPLINE_CURVE_WITH_KNOTS ( ( 4, 4 ),
 ( 0.004183487405659398924, 0.01388163287021780198 ),
 .UNSPECIFIED. ) 
 CURVE ( )  GEOMETRIC_REPRESENTATION_ITEM ( )  RATIONAL_B_SPLINE_CURVE ( ( 0.6809743333591580239, 0.7608653435686170141, 0.8672072324488977468, 1.000000000000000000 ) ) 
 REPRESENTATION_ITEM ( '' )  );
#13482 = CARTESIAN_POINT ( 'NONE',  ( 165.3321726438349515, -18.76308274332846437, 18.76308274332804160 ) ) ;
#13483 = CARTESIAN_POINT ( 'NONE',  ( -162.0762913951020892, 4.094006889353306706E-13, -41.69427287682835015 ) ) ;
#13484 = LINE ( 'NONE', #15355, #24884 ) ;
#13485 = CARTESIAN_POINT ( 'NONE',  ( -208.1127848780264742, -15.00245453012673202, 40.00000000000002132 ) ) ;
#13486 = CARTESIAN_POINT ( 'NONE',  ( -105.3755690713226585, 21.75974354311648185, -40.00000000000002132 ) ) ;
#13487 = CARTESIAN_POINT ( 'NONE',  ( 200.0000000000000000, 42.42640687119290988, 14.14213562373111976 ) ) ;
#13488 = CARTESIAN_POINT ( 'NONE',  ( 199.9999999999999432, 20.00000000000013856, 0.000000000000000000 ) ) ;
#13490 = CARTESIAN_POINT ( 'NONE',  ( -87.13361725327069962, -14.22820481747974775, -16.16779160793708314 ) ) ;
#13489 = CARTESIAN_POINT ( 'NONE',  ( 17.76569343199606621, -44.20364726159867530, -24.33587863439580090 ) ) ;
#13491 = CARTESIAN_POINT ( 'NONE',  ( -114.7818785417170488, 22.12720011206953430, -0.5288015316098635399 ) ) ;
#13492 = CARTESIAN_POINT ( 'NONE',  ( 184.8905102610680444, 13.49065550809807945, 13.49065550809809544 ) ) ;
#13493 = CARTESIAN_POINT ( 'NONE',  ( -208.1127848780265026, 55.00245453012668406, 2.449293598294708485E-15 ) ) ;
#13494 = ORIENTED_EDGE ( 'NONE', *, *, #25912, .F. ) ;
#13495 = CARTESIAN_POINT ( 'NONE',  ( 25.62979979008718701, -42.16299361905902288, 22.88075396655817073 ) ) ;
#13496 = LINE ( 'NONE', #11623, #12540 ) ;
#13497 = CARTESIAN_POINT ( 'NONE',  ( 57.59792236341147031, 26.56190807104684382, 26.56190807104692553 ) ) ;
#13498 = CARTESIAN_POINT ( 'NONE',  ( -135.8532207217289738, -40.00000000000001421, -9.153146818113709671 ) ) ;
#13499 = CARTESIAN_POINT ( 'NONE',  ( -87.10593701843048109, 21.31294500819610249, 2.647731699010448025 ) ) ;
#13500 = DIRECTION ( 'NONE',  ( 0.000000000000000000, 0.000000000000000000, 1.000000000000000000 ) ) ;
#13501 = CARTESIAN_POINT ( 'NONE',  ( 200.0000000000000568, 3.396018298074437780, 18.70303282425911462 ) ) ;
#13502 = CARTESIAN_POINT ( 'NONE',  ( 170.0000000000133014, 17.64300463311800016, 17.64300463311827016 ) ) ;
#13503 = CARTESIAN_POINT ( 'NONE',  ( -208.1127848780264742, 38.89260858015707356, 17.67593391476696141 ) ) ;
#13504 = CARTESIAN_POINT ( 'NONE',  ( -280.0000000000000568, 14.14213562373127431, -42.42640687119274645 ) ) ;
#13505 = CARTESIAN_POINT ( 'NONE',  ( -105.3145050212642104, 20.78637605557719326, -5.350913199671561316 ) ) ;
#13506 = DIRECTION ( 'NONE',  ( 0.000000000000000000, -1.000000000000000000, 0.000000000000000000 ) ) ;
#13507 = CARTESIAN_POINT ( 'NONE',  ( -86.96347745069643054, 15.38646221621821297, -41.18208027870583265 ) ) ;
#13509 = CARTESIAN_POINT ( 'NONE',  ( -238.4067589809705794, 0.6820004457912851592, -0.6820004457913123597 ) ) ;
#13508 = CARTESIAN_POINT ( 'NONE',  ( 200.0000000000000000, 42.42640687119310172, -14.14213562373052646 ) ) ;
#13510 = CARTESIAN_POINT ( 'NONE',  ( 184.8905102610680444, 41.77492675555983936, 14.79361573936436081 ) ) ;
#13511 = CARTESIAN_POINT ( 'NONE',  ( 199.9999999999999432, -20.00000000000006750, 0.000000000000000000 ) ) ;
#13512 = DIRECTION ( 'NONE',  ( 0.000000000000000000, 1.000000000000000000, 0.000000000000000000 ) ) ;
#13513 = EDGE_CURVE ( 'NONE', #5806, #19850, #21315, .T. ) ;
#13514 = CARTESIAN_POINT ( 'NONE',  ( -56.48582580120558561, -40.00000000000000000, -9.153146818113723882 ) ) ;
#13515 = CARTESIAN_POINT ( 'NONE',  ( -213.1075012329537230, 9.698598906450543566, -9.698598906450348167 ) ) ;
#13516 = CARTESIAN_POINT ( 'NONE',  ( -238.4067589809705794, 40.96449427998256709, 2.449293598294708485E-15 ) ) ;
#13517 = EDGE_LOOP ( 'NONE', ( #10836, #13393 ) ) ;
#13518 = CARTESIAN_POINT ( 'NONE',  ( 57.59792236341147031, 26.56190807104693619, -30.00663442387692115 ) ) ;
#13519 = CARTESIAN_POINT ( 'NONE',  ( -5.517256387798515682, 41.88221099414148085, 17.34817981594498804 ) ) ;
#13520 = CARTESIAN_POINT ( 'NONE',  ( 25.05785482536065700, 17.61697374401906657, 42.53113694077252660 ) ) ;
#13521 = CARTESIAN_POINT ( 'NONE',  ( -62.62756078658142656, -25.40230989543398010, -10.52198127449926623 ) ) ;
#13522 = EDGE_CURVE ( 'NONE', #15233, #25714, #13030, .T. ) ;
#13523 = EDGE_CURVE ( 'NONE', #3113, #21007, #12826, .T. ) ;
#13524 = ORIENTED_EDGE ( 'NONE', *, *, #18838, .T. ) ;
#13525 = CARTESIAN_POINT ( 'NONE',  ( -166.3490444785109048, -39.29840179227969088, 12.23457652159771669 ) ) ;
#13526 = CARTESIAN_POINT ( 'NONE',  ( 199.9999999999999432, -14.29115147104986860, -12.53286550942210198 ) ) ;
#13527 = CARTESIAN_POINT ( 'NONE',  ( 83.07250971288124219, -9.939191265011873000, 23.99533035163431194 ) ) ;
#13528 = CIRCLE ( 'NONE', #22906, 5.000000000000011546 ) ;
#13529 = DIRECTION ( 'NONE',  ( 1.000000000000000000, 0.000000000000000000, 0.000000000000000000 ) ) ;
#13530 = CARTESIAN_POINT ( 'NONE',  ( 199.0065089264240044, 19.04284699271596537, -6.106433644136123995 ) ) ;
#13531 = CARTESIAN_POINT ( 'NONE',  ( -77.90255099906767100, -8.064892378658175431, 20.29001641120675004 ) ) ;
#13532 = CARTESIAN_POINT ( 'NONE',  ( 146.6084372240433709, 40.00000000000017053, -34.62501878078291639 ) ) ;
#13533 = CARTESIAN_POINT ( 'NONE',  ( -626.9846540392142060, 90.00000000000000000, -46.18033988749894547 ) ) ;
#13534 = CARTESIAN_POINT ( 'NONE',  ( -200.0000000000000284, -22.85346793133670928, -44.96258949770064106 ) ) ;
#13535 = CARTESIAN_POINT ( 'NONE',  ( -30.26275506840324425, -1.694272468446265334, 40.00000000000002132 ) ) ;
#13537 = CARTESIAN_POINT ( 'NONE',  ( -617.0486879783372842, 28.24773862521455214, -28.32390266690136471 ) ) ;
#13536 = CARTESIAN_POINT ( 'NONE',  ( -129.2303573022295495, 9.309001179022315497, -25.82247248365979786 ) ) ;
#13538 = CARTESIAN_POINT ( 'NONE',  ( -198.0356074513804572, -15.37879056873074290, 40.00000000000002132 ) ) ;
#13539 = CARTESIAN_POINT ( 'NONE',  ( 192.4448373802101173, 20.00000000003945644, -40.00000000000002132 ) ) ;
#13540 = CARTESIAN_POINT ( 'NONE',  ( 151.7948205124836250, -33.23291073765550863, 0.000000000000000000 ) ) ;
#13541 = CARTESIAN_POINT ( 'NONE',  ( 57.59792236341147031, -1.493297263419786540E-14, 2.435789363418160658 ) ) ;
#13542 = CARTESIAN_POINT ( 'NONE',  ( 57.59792236341149163, -39.99999999999961631, -37.56421063658228832 ) ) ;
#13543 = CARTESIAN_POINT ( 'NONE',  ( -28.75808802781891416, -35.61482992978318407, 18.59445401971624889 ) ) ;
#13544 = ORIENTED_EDGE ( 'NONE', *, *, #10058, .T. ) ;
#13546 = CARTESIAN_POINT ( 'NONE',  ( 5.823571940253781776, 44.77584346942675353, -24.75780943189465688 ) ) ;
#13545 = CARTESIAN_POINT ( 'NONE',  ( -86.86493150571114086, -19.77569912839162569, 7.943527260496431985 ) ) ;
#13547 = CARTESIAN_POINT ( 'NONE',  ( 19.06497207195982924, -54.19242893257843008, 40.00000000000002132 ) ) ;
#13548 = CARTESIAN_POINT ( 'NONE',  ( -280.0000000000000000, -14.14213562373118371, 14.14213562373078936 ) ) ;
#13549 = CARTESIAN_POINT ( 'NONE',  ( -93.01741312764114866, -8.946232117585104504, 20.50009083230827756 ) ) ;
#13550 = DIRECTION ( 'NONE',  ( 1.000000000000000000, 0.000000000000000000, 0.000000000000000000 ) ) ;
#13551 = ORIENTED_EDGE ( 'NONE', *, *, #1673, .T. ) ;
#13552 = EDGE_LOOP ( 'NONE', ( #24201, #16551, #21707, #2733, #22080 ) ) ;
#13553 = CARTESIAN_POINT ( 'NONE',  ( -86.86493150571118349, -19.60045294882770506, 8.366608963953762412 ) ) ;
#13554 = CARTESIAN_POINT ( 'NONE',  ( 153.3020327024397034, 11.77299484472959890, -28.42252382389417775 ) ) ;
#13555 = AXIS2_PLACEMENT_3D ( 'NONE', #22208, #26070, #6100 ) ;
#13556 = ORIENTED_EDGE ( 'NONE', *, *, #13444, .T. ) ;
#13557 = CARTESIAN_POINT ( 'NONE',  ( -100.0753760173618332, 8.149786832858671559, -20.72827493166386859 ) ) ;
#13558 = ORIENTED_EDGE ( 'NONE', *, *, #7793, .T. ) ;
#13559 = CARTESIAN_POINT ( 'NONE',  ( 200.0000000000000000, -3.101357108925543837, 18.75734389255849521 ) ) ;
#13560 = CARTESIAN_POINT ( 'NONE',  ( -87.13361725327072804, 5.903697393916396424E-14, -21.49321519333428299 ) ) ;
#13561 = CARTESIAN_POINT ( 'NONE',  ( 19.06497207195981147, 38.31983398719620482, 38.31983398719633271 ) ) ;
#13562 = CARTESIAN_POINT ( 'NONE',  ( -105.2054292635175727, 7.329160573984922335E-13, -21.49321519473985020 ) ) ;
#13563 = CARTESIAN_POINT ( 'NONE',  ( -135.8532207217289738, 7.002209520526292428E-15, -9.153146818113572891 ) ) ;
#13564 = FACE_OUTER_BOUND ( 'NONE', #6954, .T. ) ;
#13565 = CARTESIAN_POINT ( 'NONE',  ( -90.07798792367796636, -2.498525064387717877E-13, 22.27377874500495381 ) ) ;
#13566 = DIRECTION ( 'NONE',  ( -3.936061032557143868E-17, 0.2142691827715866859, 0.9767746502210202797 ) ) ;
#13567 = DIRECTION ( 'NONE',  ( -1.000000000000000000, -0.000000000000000000, -0.000000000000000000 ) ) ;
#13568 = CARTESIAN_POINT ( 'NONE',  ( -192.9588430854690273, -39.99999999999948841, -54.46834944098263520 ) ) ;
#13569 = CARTESIAN_POINT ( 'NONE',  ( -199.9999999999999716, -48.57705986237291995, -14.87399974031227501 ) ) ;
#13570 = CARTESIAN_POINT ( 'NONE',  ( 130.8568914410475372, 24.07718906447243867, -24.07718906447216156 ) ) ;
#13571 = CARTESIAN_POINT ( 'NONE',  ( -162.0762913951020892, -3.568845385355699554E-14, 1.694272876828323948 ) ) ;
#13572 = CARTESIAN_POINT ( 'NONE',  ( -198.9234529669031701, 14.16707775658443857, 49.24835336340146341 ) ) ;
#13573 = CARTESIAN_POINT ( 'NONE',  ( -265.0000000000000000, -10.00000000000004796, -6.532754371361504014E-30 ) ) ;
#13574 = CARTESIAN_POINT ( 'NONE',  ( -259.2033419157646676, 6.730120644403521979, -6.730120644403498886 ) ) ;
#13575 = CARTESIAN_POINT ( 'NONE',  ( -100.7734535825088358, 6.065416334915073333E-14, -22.67402823373191723 ) ) ;
#13576 = CARTESIAN_POINT ( 'NONE',  ( 19.06497207195980792, -18.24870850772763475, 38.31983398719622613 ) ) ;
#13577 = CARTESIAN_POINT ( 'NONE',  ( -30.26275506840322294, -57.76657404653985139, -1.198031551616531853 ) ) ;
#13578 = CARTESIAN_POINT ( 'NONE',  ( -661.3723022781085774, 44.52532212870602280, -6.545884190707156769 ) ) ;
#13579 = CARTESIAN_POINT ( 'NONE',  ( -2.937533998744902508, 23.68967259522915114, 43.32931883109763760 ) ) ;
#13580 = ORIENTED_EDGE ( 'NONE', *, *, #21416, .T. ) ;
#13581 = CARTESIAN_POINT ( 'NONE',  ( 163.1118516004056573, 37.29075403953132906, 19.27778845539275565 ) ) ;
#13582 = DIRECTION ( 'NONE',  ( 0.000000000000000000, 0.000000000000000000, 1.000000000000000000 ) ) ;
#13583 = FACE_OUTER_BOUND ( 'NONE', #11023, .T. ) ;
#13584 = EDGE_LOOP ( 'NONE', ( #24680, #9664, #3989, #15043 ) ) ;
#13585 = CARTESIAN_POINT ( 'NONE',  ( 4.995406935893290878, 1.606505379428369110E-13, -15.24977328854832592 ) ) ;
#13586 = CARTESIAN_POINT ( 'NONE',  ( -3.971463587458989863, -23.46415232637805204, 43.02522237042967390 ) ) ;
#13587 = CARTESIAN_POINT ( 'NONE',  ( 7.340276910564550228, -44.87059041559395922, 24.82763627182874089 ) ) ;
#13588 = ORIENTED_EDGE ( 'NONE', *, *, #7255, .T. ) ;
#13589 = ORIENTED_EDGE ( 'NONE', *, *, #8428, .T. ) ;
#13590 = CARTESIAN_POINT ( 'NONE',  ( 19.06497207195980792, 54.19242893257844429, -40.00000000000002132 ) ) ;
#13591 = CARTESIAN_POINT ( 'NONE',  ( -30.26275506840324070, -1.198031551616032919, 1.198031551616014712 ) ) ;
#13592 = CARTESIAN_POINT ( 'NONE',  ( 151.7948205124836534, 40.00000000000002842, 6.767089262349174739 ) ) ;
#13593 = CARTESIAN_POINT ( 'NONE',  ( -94.58414068586590417, -20.73981583695825037, -8.590713000584871750 ) ) ;
#13594 = CIRCLE ( 'NONE', #17415, 5.000000000000004441 ) ;
#13595 = DIRECTION ( 'NONE',  ( -1.836970198721030181E-16, 1.000000000000000000, 0.000000000000000000 ) ) ;
#13596 = CARTESIAN_POINT ( 'NONE',  ( 91.82158438592156813, 39.99999999999986500, 17.20528682183341473 ) ) ;
#13597 = CARTESIAN_POINT ( 'NONE',  ( 184.8905102610680444, -40.00000000000005684, 19.07866798485543569 ) ) ;
#13598 = CARTESIAN_POINT ( 'NONE',  ( 199.9999999999999147, -15.08385563027219156, -11.56407354529143205 ) ) ;
#13599 = CARTESIAN_POINT ( 'NONE',  ( 130.8568914410475088, 40.00000000000015632, -34.05028731879774284 ) ) ;
#13600 = EDGE_CURVE ( 'NONE', #23212, #4362, #12694, .T. ) ;
#13601 = FACE_OUTER_BOUND ( 'NONE', #4291, .T. ) ;
#13602 = CARTESIAN_POINT ( 'NONE',  ( -62.79433447037396832, -9.335111860870215494, -25.93934121798541881 ) ) ;
#13603 = CARTESIAN_POINT ( 'NONE',  ( 199.9999999999999432, 14.14213562373093680, 14.14213562373114641 ) ) ;
#13604 = CARTESIAN_POINT ( 'NONE',  ( -87.01701082927806397, -18.46482525710459299, 10.86389608312037680 ) ) ;
#13605 = CARTESIAN_POINT ( 'NONE',  ( -162.0762913951021176, -40.00000000000003553, -1.694272876828743168 ) ) ;
#13606 = CARTESIAN_POINT ( 'NONE',  ( 73.43438319819851756, 9.843172589490714941, 28.18283897611961919 ) ) ;
#13607 = CARTESIAN_POINT ( 'NONE',  ( -86.96347745069645896, 21.75974354311648895, -0.000000000000000000 ) ) ;
#13608 = CARTESIAN_POINT ( 'NONE',  ( 200.0000000000000000, 20.00000000000013856, -40.00000000000002132 ) ) ;
#13609 = EDGE_CURVE ( 'NONE', #1209, #13720, #16199, .T. ) ;
#13610 = CARTESIAN_POINT ( 'NONE',  ( -30.26275506840324070, -1.198031551616032919, 1.198031551616014712 ) ) ;
#13611 = CARTESIAN_POINT ( 'NONE',  ( 130.8568914410475372, 34.05028731879791337, 0.000000000000000000 ) ) ;
#13612 = CARTESIAN_POINT ( 'NONE',  ( -3.555049149807454345, -43.14507846637731348, -23.55301256057186166 ) ) ;
#13613 = CARTESIAN_POINT ( 'NONE',  ( -114.4364955367328349, 20.29001642038852538, -8.064892380842216824 ) ) ;
#13614 = CARTESIAN_POINT ( 'NONE',  ( 0.2972598230769907257, 66.70487387989857098, 10.13633138497486641 ) ) ;
#13615 = ADVANCED_FACE ( 'NONE', ( #5756 ), #22526, .T. ) ;
#13616 = CARTESIAN_POINT ( 'NONE',  ( 146.6084372240433709, 5.374981219217002781, -40.00000000000002132 ) ) ;
#13617 = B_SPLINE_CURVE_WITH_KNOTS ( 'NONE', 3,
 ( #4103, #14195, #16461, #22327, #2101, #25696 ),
 .UNSPECIFIED., .F., .F.,
 ( 4, 2, 4 ),
 ( -6.000000000394485207E-08, 0.04016968416333294850, 0.08033942832666590705 ),
 .UNSPECIFIED. ) ;
#13618 = ORIENTED_EDGE ( 'NONE', *, *, #22424, .T. ) ;
#13619 = EDGE_CURVE ( 'NONE', #16348, #17701, #15561, .T. ) ;
#13620 = CARTESIAN_POINT ( 'NONE',  ( 22.78333232259052110, -43.17211919388228836, 17.88247728649368895 ) ) ;
#13621 = CARTESIAN_POINT ( 'NONE',  ( -348.0000000000001137, -4.857225732735059864E-14, 31.79780246617542616 ) ) ;
#13622 = CARTESIAN_POINT ( 'NONE',  ( -105.3755690713226585, 12.89780903124410472, -43.67073346367977393 ) ) ;
#13623 = CARTESIAN_POINT ( 'NONE',  ( 0.2972598230770030492, -1.921041075453695163E-13, 54.33493731733936016 ) ) ;
#13624 = AXIS2_PLACEMENT_3D ( 'NONE', #11384, #25645, #21390 ) ;
#13625 = CARTESIAN_POINT ( 'NONE',  ( 146.6084372240433709, 3.800685668858042821, 52.76785682606522698 ) ) ;
#13626 = VECTOR ( 'NONE', #941, 1000.000000000000114 ) ;
#13627 = CARTESIAN_POINT ( 'NONE',  ( -259.2033419157646676, -9.517827891722680178, -40.00000000000002132 ) ) ;
#13628 = CIRCLE ( 'NONE', #4739, 5.000000000000039080 ) ;
#13629 = DIRECTION ( 'NONE',  ( 0.000000000000000000, 1.000000000000000000, 0.000000000000000000 ) ) ;
#13630 = CARTESIAN_POINT ( 'NONE',  ( 199.9999999999996305, 11.56193655722446678, 15.09741884674619072 ) ) ;
#13631 = CARTESIAN_POINT ( 'NONE',  ( -82.30220482034330587, -7.441767004318580625, -18.74474319042437642 ) ) ;
#13632 = CARTESIAN_POINT ( 'NONE',  ( 14.38125909742180220, 39.01709431150892016, 17.55144818341517166 ) ) ;
#13633 = CARTESIAN_POINT ( 'NONE',  ( 184.8905102610680444, 14.79361573936424890, -41.77492675555986068 ) ) ;
#13634 = CARTESIAN_POINT ( 'NONE',  ( -110.0579415639987388, 19.23682107564352961, -6.226559743088629695 ) ) ;
#13635 = CARTESIAN_POINT ( 'NONE',  ( 57.59792236341147031, -1.493297263419786540E-14, 2.435789363418160658 ) ) ;
#13636 = CARTESIAN_POINT ( 'NONE',  ( 130.8568914410475088, 52.36146031193427319, -4.207082182989173802 ) ) ;
#13638 = CARTESIAN_POINT ( 'NONE',  ( -213.1075012329537230, 9.698598906438871126, -66.26714140136179765 ) ) ;
#13637 = CARTESIAN_POINT ( 'NONE',  ( -56.48582580120558561, 6.472252184284607246, -50.09629031063960269 ) ) ;
#13639 = CARTESIAN_POINT ( 'NONE',  ( -280.0000000000000000, -14.14213562373118549, 14.14213562373078936 ) ) ;
#13640 = LINE ( 'NONE', #13386, #8308 ) ;
#13641 = CARTESIAN_POINT ( 'NONE',  ( 163.1118516004056573, -19.27778845538761132, -19.27778845538770724 ) ) ;
#13643 = CARTESIAN_POINT ( 'NONE',  ( 4.995406935893305089, -40.00000000000021316, 55.24977328853194791 ) ) ;
#13642 = CARTESIAN_POINT ( 'NONE',  ( -86.96347745069644475, 12.89780903124349898, 43.67073346367994446 ) ) ;
#13644 = CARTESIAN_POINT ( 'NONE',  ( 57.59792236341148453, -26.56190807104700369, 26.56190807104673723 ) ) ;
#13645 = CARTESIAN_POINT ( 'NONE',  ( -280.0000000000000568, 14.14213562373038968, 42.42640687119305198 ) ) ;
#13646 = CIRCLE ( 'NONE', #15764, 5.000000000000004441 ) ;
#13647 = CARTESIAN_POINT ( 'NONE',  ( -162.0762913951020892, 41.69427287682832173, 2.449293598294708485E-15 ) ) ;
#13648 = ORIENTED_EDGE ( 'NONE', *, *, #22837, .T. ) ;
#13649 = CARTESIAN_POINT ( 'NONE',  ( -208.1127848780265026, 10.60833733269537049, 10.60833733269544510 ) ) ;
#13650 = B_SPLINE_CURVE_WITH_KNOTS ( 'NONE', 3,
 ( #18342, #12351, #20480, #2254, #18745, #16485, #8631, #18878, #10362, #391, #16742, #24875 ),
 .UNSPECIFIED., .F., .F.,
 ( 4, 2, 2, 2, 2, 4 ),
 ( -5.998499567893129066E-08, 0.003531500499830294692, 0.007063060984656268325, 0.01412618195430822773, 0.02118930292396017934, 0.02825242389361213441 ),
 .UNSPECIFIED. ) ;
#13651 = CARTESIAN_POINT ( 'NONE',  ( -200.0000000000000000, -71.50000000000002842, 66.50000000000005684 ) ) ;
#13652 = CARTESIAN_POINT ( 'NONE',  ( 44.46627453567793964, 15.24062802624261437, 36.79413088023001421 ) ) ;
#13653 = CARTESIAN_POINT ( 'NONE',  ( 98.29820294267493352, -20.00000000000511235, 5.223721743777709619E-12 ) ) ;
#13654 = VERTEX_POINT ( 'NONE', #5464 ) ;
#13655 = CARTESIAN_POINT ( 'NONE',  ( -188.3392535381713913, -47.00481007172062675, 13.83023904993491371 ) ) ;
#13656 = CARTESIAN_POINT ( 'NONE',  ( 199.9999999999998010, -4.930716969832944940, -18.35446462305003834 ) ) ;
#13657 = CARTESIAN_POINT ( 'NONE',  ( 22.75882399337420026, -17.88527043150875429, 43.17886244245843130 ) ) ;
#13658 = ADVANCED_FACE ( 'NONE', ( #17686 ), #7573, .F. ) ;
#13659 = CARTESIAN_POINT ( 'NONE',  ( 23.39921416754922134, 13.79910252519628955, -46.79910576274355094 ) ) ;
#13660 = CARTESIAN_POINT ( 'NONE',  ( 199.0057329523134513, 9.713090712928652337, -17.48024697358846069 ) ) ;
#13661 = AXIS2_PLACEMENT_3D ( 'NONE', #4856, #6700, #2865 ) ;
#13662 = CARTESIAN_POINT ( 'NONE',  ( 190.0000000000000000, 70.00000000000000000, 0.000000000000000000 ) ) ;
#13663 = CARTESIAN_POINT ( 'NONE',  ( 57.59792236341146321, 40.00000000000004263, -2.435789363418021214 ) ) ;
#13664 = CARTESIAN_POINT ( 'NONE',  ( -295.0000000000000568, 9.999999999999948486, 0.000000000000000000 ) ) ;
#13665 = DIRECTION ( 'NONE',  ( 1.000000000000000000, -0.000000000000000000, -0.000000000000000000 ) ) ;
#13666 = CARTESIAN_POINT ( 'NONE',  ( 0.2972598230770129857, -54.33493731733938148, 40.00000000000002132 ) ) ;
#13668 = CARTESIAN_POINT ( 'NONE',  ( -611.0068738282783443, 30.90074614832916566, -25.40852347241385800 ) ) ;
#13667 = CARTESIAN_POINT ( 'NONE',  ( -183.1091233172239185, 13.45963571009543891, -45.18843800006289513 ) ) ;
#13669 = EDGE_CURVE ( 'NONE', #1902, #15674, #10147, .T. ) ;
#13670 = CARTESIAN_POINT ( 'NONE',  ( 98.29820294268675696, -2.727061086135049273, -20.00000000000119371 ) ) ;
#13671 = CARTESIAN_POINT ( 'NONE',  ( -192.9588430854690273, -54.46834944101725284, -40.00000000000002132 ) ) ;
#13672 = CARTESIAN_POINT ( 'NONE',  ( -30.26275506840324425, 1.694272468446254232, 40.00000000000002132 ) ) ;
#13673 = CARTESIAN_POINT ( 'NONE',  ( 4.995406935893306866, -39.99999999999944578, -55.24977328856505920 ) ) ;
#13674 = CARTESIAN_POINT ( 'NONE',  ( 190.0000000000000000, -52.49999999999970868, 82.49999999999998579 ) ) ;
#13675 = CARTESIAN_POINT ( 'NONE',  ( 19.06497207195981147, -10.03556273973425483, -10.03556273973443247 ) ) ;
#13676 = ORIENTED_EDGE ( 'NONE', *, *, #7036, .F. ) ;
#13677 = CARTESIAN_POINT ( 'NONE',  ( -28.75808802591297209, -38.33175228464053674, 12.03522322449780724 ) ) ;
#13678 = CARTESIAN_POINT ( 'NONE',  ( 4.995406935893289102, 10.78321810388998081, 10.78321810389001811 ) ) ;
#13679 = CARTESIAN_POINT ( 'NONE',  ( 163.1118516004056573, -19.27778845538787422, 19.27778845538743724 ) ) ;
#13680 = FACE_OUTER_BOUND ( 'NONE', #16521, .T. ) ;
#13681 = DIRECTION ( 'NONE',  ( 0.000000000000000000, 0.000000000000000000, 1.000000000000000000 ) ) ;
#13682 = ORIENTED_EDGE ( 'NONE', *, *, #21906, .T. ) ;
#13683 = VERTEX_POINT ( 'NONE', #8071 ) ;
#13684 = VECTOR ( 'NONE', #17703, 1000.000000000000000 ) ;
#13685 = CARTESIAN_POINT ( 'NONE',  ( -190.0000000000000000, -52.49999999999972289, -82.49999999999998579 ) ) ;
#13686 = CARTESIAN_POINT ( 'NONE',  ( 60.28378959955089300, -33.17072922786156397, -10.93033916064820055 ) ) ;
#13687 = ORIENTED_EDGE ( 'NONE', *, *, #2313, .F. ) ;
#13688 = CARTESIAN_POINT ( 'NONE',  ( 151.7948205124836534, -33.23291073765550863, -40.00000000000002132 ) ) ;
#13689 = CARTESIAN_POINT ( 'NONE',  ( -97.73860346104272878, -20.56359266937362662, 8.987542150667973573 ) ) ;
#13690 = ORIENTED_EDGE ( 'NONE', *, *, #3427, .F. ) ;
#13691 = CARTESIAN_POINT ( 'NONE',  ( 199.9999999999997158, -10.44119114510941770, 15.88703355754643098 ) ) ;
#13692 = CARTESIAN_POINT ( 'NONE',  ( -190.6721449140024447, 13.94344083317847272, 47.76494005424133604 ) ) ;
#13693 = CARTESIAN_POINT ( 'NONE',  ( 4.995406935893287326, 67.35176059882533650, 10.78321810390163549 ) ) ;
#13694 = CARTESIAN_POINT ( 'NONE',  ( 200.0000000000000000, -66.50000000000001421, 66.50000000000005684 ) ) ;
#13695 = CARTESIAN_POINT ( 'NONE',  ( 57.59792236341147031, 1.908507979671054758E-14, -2.435789363418160658 ) ) ;
#13696 = CARTESIAN_POINT ( 'NONE',  ( 146.6084372240433993, 3.800685668858732935, -3.800685668858610367 ) ) ;
#13697 = CARTESIAN_POINT ( 'NONE',  ( 170.0000000000000000, 3.122849337825751958E-14, 0.000000000000000000 ) ) ;
#13698 = DIRECTION ( 'NONE',  ( 0.000000000000000000, -0.9767746502210202797, 0.2142691827715866859 ) ) ;
#13699 = CARTESIAN_POINT ( 'NONE',  ( 192.4448373802100889, -1.741373372144848397E-13, 20.00000000003942091 ) ) ;
#13700 = CARTESIAN_POINT ( 'NONE',  ( 19.06497207195982924, -39.99999999999945288, -54.19242893257885640 ) ) ;
#13701 = CARTESIAN_POINT ( 'NONE',  ( -105.4293522939502310, -9.002736003369118833, 19.36070119851716598 ) ) ;
#13702 = CARTESIAN_POINT ( 'NONE',  ( -208.1127848780265026, -10.60833733269551971, 10.60833733269537049 ) ) ;
#13703 = CARTESIAN_POINT ( 'NONE',  ( -238.4067589809705794, -4.716212492215116094E-14, 0.9644942799825824142 ) ) ;
#13704 = EDGE_CURVE ( 'NONE', #17673, #22942, #9820, .T. ) ;
#13705 = CARTESIAN_POINT ( 'NONE',  ( -198.0356074513804572, -67.44298959250878056, 10.87444709758448447 ) ) ;
#13706 = LINE ( 'NONE', #3878, #10044 ) ;
#13707 = CARTESIAN_POINT ( 'NONE',  ( -83.21262154144248768, 13.72187187061462232, 33.12752917118429963 ) ) ;
#13708 = CARTESIAN_POINT ( 'NONE',  ( 136.1360204305621266, -3.419521671106983309E-13, 35.03383547441296741 ) ) ;
#13709 = CARTESIAN_POINT ( 'NONE',  ( 184.8905102610680444, -39.99999999999991473, -20.92133201514458207 ) ) ;
#13710 = CARTESIAN_POINT ( 'NONE',  ( -198.0356074513804572, 39.15871834505901461, 39.15871834505919935 ) ) ;
#13711 = CARTESIAN_POINT ( 'NONE',  ( -162.0762913951020892, -1.198031840385767266, -1.198031840385758384 ) ) ;
#13712 = CARTESIAN_POINT ( 'NONE',  ( -188.2871287166310594, -23.44689273421379738, -43.00155302796976287 ) ) ;
#13713 = CARTESIAN_POINT ( 'NONE',  ( 136.1360204305621266, 24.77266263493138965, -24.77266263493110188 ) ) ;
#13714 = ORIENTED_EDGE ( 'NONE', *, *, #24102, .F. ) ;
#13715 = CARTESIAN_POINT ( 'NONE',  ( -213.1075012329537230, 9.698598906438871126, -66.26714140136179765 ) ) ;
#13716 = CARTESIAN_POINT ( 'NONE',  ( -91.56559293963836410, 22.67402823373190301, -40.00000000000002132 ) ) ;
#13717 = PLANE ( 'NONE',  #18701 ) ;
#13718 = CARTESIAN_POINT ( 'NONE',  ( -198.0356074513804572, -17.40982414986427429, -39.15871834505933435 ) ) ;
#13719 = CARTESIAN_POINT ( 'NONE',  ( -87.07756624669964651, 3.737545040615061875, 21.12895881758995387 ) ) ;
#13720 = VERTEX_POINT ( 'NONE', #2232 ) ;
#13721 = CARTESIAN_POINT ( 'NONE',  ( 199.9999999999999432, 16.46500086087206682, -9.483425485471467908 ) ) ;
#13722 = CARTESIAN_POINT ( 'NONE',  ( 199.0242950697381445, -19.85973387450291128, 2.734947709465418875 ) ) ;
#13723 = CARTESIAN_POINT ( 'NONE',  ( 2.303792037522391922, 18.40682559462096179, 44.43800799080432995 ) ) ;
#13724 = ORIENTED_EDGE ( 'NONE', *, *, #18043, .F. ) ;
#13725 = VERTEX_POINT ( 'NONE', #4240 ) ;
#13726 = CARTESIAN_POINT ( 'NONE',  ( -208.1127848780264742, 55.00245453010919050, -40.00000000000002132 ) ) ;
#13727 = CARTESIAN_POINT ( 'NONE',  ( -105.3755690713226727, 15.38646221621793231, -15.38646221621779020 ) ) ;
#13728 = CARTESIAN_POINT ( 'NONE',  ( -91.56559293963836410, 40.00000000000008527, -22.67402823373177867 ) ) ;
#13729 = CARTESIAN_POINT ( 'NONE',  ( -97.73806390048314086, -20.71810467718897542, -8.581719943884214885 ) ) ;
#13730 = DIRECTION ( 'NONE',  ( 0.000000000000000000, -1.000000000000000000, 0.000000000000000000 ) ) ;
#13731 = CARTESIAN_POINT ( 'NONE',  ( 57.59792236341146321, 40.00000000000000711, 2.435789363418579434 ) ) ;
#13732 = CARTESIAN_POINT ( 'NONE',  ( 200.0000000000000568, -14.79650836250383250, 11.93661649116771173 ) ) ;
#13733 = DIRECTION ( 'NONE',  ( 0.000000000000000000, -1.000000000000000000, 0.000000000000000000 ) ) ;
#13734 = CARTESIAN_POINT ( 'NONE',  ( -3.993758944536813349, -23.45926997169897277, -43.01863922058836209 ) ) ;
#13735 = CARTESIAN_POINT ( 'NONE',  ( 4.995406935893300648, -10.78321810387790514, -67.35176059880241439 ) ) ;
#13736 = CARTESIAN_POINT ( 'NONE',  ( -77.78697283798516082, -20.89074004981921462, 6.810146944722274220 ) ) ;
#13737 = CARTESIAN_POINT ( 'NONE',  ( 19.06497207195981858, -38.31983398719616218, -18.24870850772777331 ) ) ;
#13738 = CARTESIAN_POINT ( 'NONE',  ( -56.48582580120559271, -1.062504017861011783E-13, 9.153146818113587102 ) ) ;
#13739 = CARTESIAN_POINT ( 'NONE',  ( -105.2940237833728219, -20.91877113668857291, -4.710801307200714660 ) ) ;
#13740 = CARTESIAN_POINT ( 'NONE',  ( -198.0356074513804572, -15.37879056873074290, 0.000000000000000000 ) ) ;
#13741 = CARTESIAN_POINT ( 'NONE',  ( -91.56559293963834989, -17.32597176626812896, -2.449293598294708485E-15 ) ) ;
#13742 = CARTESIAN_POINT ( 'NONE',  ( 57.59792236341147031, 30.00663442387683588, 26.56190807104703211 ) ) ;
#13743 = CARTESIAN_POINT ( 'NONE',  ( -162.0762913951020892, -41.69427287672991866, -40.00000000000002132 ) ) ;
#13744 = CARTESIAN_POINT ( 'NONE',  ( -109.1264249741454790, 13.72187187123907393, 33.12752917269271080 ) ) ;
#13745 = CARTESIAN_POINT ( 'NONE',  ( 91.82158438592158234, -1.633484621919921769E-13, 17.20528682183300262 ) ) ;
#13746 = CARTESIAN_POINT ( 'NONE',  ( -208.1127848780264742, 67.17687982760683951, 10.60833733268317403 ) ) ;
#13747 = CARTESIAN_POINT ( 'NONE',  ( -213.1075012329537230, 53.71589010950162191, -40.00000000000002132 ) ) ;
#13748 = ORIENTED_EDGE ( 'NONE', *, *, #19163, .T. ) ;
#13749 = FACE_OUTER_BOUND ( 'NONE', #15080, .T. ) ;
#13750 = CARTESIAN_POINT ( 'NONE',  ( -53.37717264285771535, -10.11115224722899342, 29.42738956023912777 ) ) ;
#13751 = CARTESIAN_POINT ( 'NONE',  ( 151.7948205124836534, 4.785054706298574878, -51.78348778862537927 ) ) ;
#13752 = CARTESIAN_POINT ( 'NONE',  ( 163.1118516004056573, -1.695744499706194789E-14, 12.73709011382475254 ) ) ;
#13753 = CARTESIAN_POINT ( 'NONE',  ( 57.59792236341147031, -1.722363176415055985, 1.722363176415024677 ) ) ;
#13754 = CARTESIAN_POINT ( 'NONE',  ( -259.2033419157646676, -9.517827891722680178, 0.000000000000000000 ) ) ;
#13755 = CARTESIAN_POINT ( 'NONE',  ( -105.3755690713226727, -21.75974354311652093, 0.000000000000000000 ) ) ;
#13756 = PRODUCT ( 'Coupling rod', 'Coupling rod', '', ( #25945 ) ) ;
#13757 = LINE ( 'NONE', #21753, #2379 ) ;
#13758 = CARTESIAN_POINT ( 'NONE',  ( 200.0000000000000568, 5.208214048020466613, 18.28294570233482119 ) ) ;
#13759 = CARTESIAN_POINT ( 'NONE',  ( -77.84504298467653882, -7.440570986992908864, -20.58891737387387977 ) ) ;
#13760 = CARTESIAN_POINT ( 'NONE',  ( 192.4448373802100889, -14.14213562375896061, 14.14213562375865330 ) ) ;
#13761 = CARTESIAN_POINT ( 'NONE',  ( -56.48582580120559982, 34.75652343174628101, -21.81201906317743067 ) ) ;
#13762 = EDGE_CURVE ( 'NONE', #22287, #22653, #13617, .T. ) ;
#13763 = CARTESIAN_POINT ( 'NONE',  ( -105.2143515744611477, 21.43501564603285559, -1.534306871497952640 ) ) ;
#13764 = CARTESIAN_POINT ( 'NONE',  ( -77.55658273868580466, 16.64052652070787985, -14.65657382810189802 ) ) ;
#13765 = CARTESIAN_POINT ( 'NONE',  ( -162.0762913951020892, -29.48230308784744125, -29.48230308784792442 ) ) ;
#13767 = CARTESIAN_POINT ( 'NONE',  ( -56.48582580120559982, -34.75652343174584047, -21.81201906317815187 ) ) ;
#13766 = CARTESIAN_POINT ( 'NONE',  ( -238.4067589809705794, -0.6820004457337348613, -57.25054294065803617 ) ) ;
#13768 = CARTESIAN_POINT ( 'NONE',  ( -56.48582580120559982, -34.75652343174584047, -21.81201906317815187 ) ) ;
#13769 = DIRECTION ( 'NONE',  ( 0.000000000000000000, 1.000000000000000000, 0.000000000000000000 ) ) ;
#13770 = CARTESIAN_POINT ( 'NONE',  ( 151.7948205124836250, 33.23291073765556547, 0.000000000000000000 ) ) ;
#13772 = CARTESIAN_POINT ( 'NONE',  ( 146.6084372240433993, 1.478241399363601114E-13, -34.62501878078305850 ) ) ;
#13771 = CARTESIAN_POINT ( 'NONE',  ( 14.38125909742180752, 10.73282306404735387, -10.73282306404708919 ) ) ;
#13773 = CARTESIAN_POINT ( 'NONE',  ( -100.7734535825088500, 44.31723036834890905, 12.25131212657507795 ) ) ;
#13774 = CARTESIAN_POINT ( 'NONE',  ( 14.38125909742180752, 10.73282306404735387, -10.73282306404708919 ) ) ;
#13775 = CARTESIAN_POINT ( 'NONE',  ( 4.995406935893288214, 15.24977328854832770, 40.00000000000002132 ) ) ;
#13776 = ORIENTED_EDGE ( 'NONE', *, *, #7337, .T. ) ;
#13777 = CARTESIAN_POINT ( 'NONE',  ( 170.2234770963711128, 10.92277846919210660, -45.64576402573182889 ) ) ;
#13778 = CARTESIAN_POINT ( 'NONE',  ( 69.64403118996989406, 28.54215590813338110, 11.82254807651625761 ) ) ;
#13779 = CARTESIAN_POINT ( 'NONE',  ( -4.039451493210483690, -13.82811171175408127, -46.99046209229819482 ) ) ;
#13780 = CARTESIAN_POINT ( 'NONE',  ( -192.9588430854689989, 14.46834944099965981, 0.000000000000000000 ) ) ;
#13781 = ORIENTED_EDGE ( 'NONE', *, *, #6614, .F. ) ;
#13782 = CARTESIAN_POINT ( 'NONE',  ( -3.901164313503196812, 23.47934491069935703, -43.04571088859049866 ) ) ;
#13783 = DIRECTION ( 'NONE',  ( 1.000000000000000000, -1.836970198721030181E-16, -0.000000000000000000 ) ) ;
#13784 = CARTESIAN_POINT ( 'NONE',  ( -3.966425590329204720, -13.83202835294355459, 47.01685867532394525 ) ) ;
#13785 = CARTESIAN_POINT ( 'NONE',  ( 17.91733029159264490, 24.32486282482700091, -44.18858371746296143 ) ) ;
#13786 = CARTESIAN_POINT ( 'NONE',  ( 199.0072342795740497, 19.67962538453564036, -3.556093180948044274 ) ) ;
#13787 = CARTESIAN_POINT ( 'NONE',  ( -86.84962968273566730, 19.67999904273991163, 8.151722510992470916 ) ) ;
#13788 = FACE_OUTER_BOUND ( 'NONE', #4883, .T. ) ;
#13789 = CARTESIAN_POINT ( 'NONE',  ( 136.1360204305621551, 31.79587985999232558, 24.77266263493161702 ) ) ;
#13790 = CARTESIAN_POINT ( 'NONE',  ( -192.9588430854690273, -14.46834944099973264, 40.00000000000002132 ) ) ;
#13791 = AXIS2_PLACEMENT_3D ( 'NONE', #22673, #20809, #4582 ) ;
#13793 = CARTESIAN_POINT ( 'NONE',  ( -597.8200346137707584, 39.37724756625295441, -7.048631215857795951 ) ) ;
#13792 = CARTESIAN_POINT ( 'NONE',  ( 199.9999999999998863, 13.43021917686961331, -13.43983678748323918 ) ) ;
#13794 = CARTESIAN_POINT ( 'NONE',  ( -192.9588430854689989, 10.23066800230756712, -10.23066800230735396 ) ) ;
#13795 = CARTESIAN_POINT ( 'NONE',  ( -238.4067589809705794, -0.9644942799826263791, -40.00000000000002132 ) ) ;
#13796 = CARTESIAN_POINT ( 'NONE',  ( -192.9588430854690273, 54.46834944101718889, 40.00000000000002132 ) ) ;
#13797 = CARTESIAN_POINT ( 'NONE',  ( 57.59792236341149163, -39.99999999999961631, -37.56421063658228832 ) ) ;
#13798 = CARTESIAN_POINT ( 'NONE',  ( 98.29820294267409508, -12.20973600809984738, 15.89413956775044845 ) ) ;
#13799 = CARTESIAN_POINT ( 'NONE',  ( -208.1127848780265026, -10.60833733269537227, -10.60833733269551793 ) ) ;
#13800 = ORIENTED_EDGE ( 'NONE', *, *, #20172, .F. ) ;
#13801 = CARTESIAN_POINT ( 'NONE',  ( 98.29820294267436509, 14.14213562374297695, -14.14213562372651189 ) ) ;
#13802 = CARTESIAN_POINT ( 'NONE',  ( 136.1360204305621266, 35.03383547441298873, 0.000000000000000000 ) ) ;
#13803 = CARTESIAN_POINT ( 'NONE',  ( -105.4741150117391015, -7.943527260750077978, 19.77569912955109288 ) ) ;
#13804 = ITEM_DEFINED_TRANSFORMATION ( 'NONE', 'NONE', #24447,  #21058 ) ;
#13805 = AXIS2_PLACEMENT_3D ( 'NONE', #7178, #15668, #19294 ) ;
#13806 = ORIENTED_EDGE ( 'NONE', *, *, #9711, .T. ) ;
#13807 = ORIENTED_EDGE ( 'NONE', *, *, #3062, .F. ) ;
#13808 = CARTESIAN_POINT ( 'NONE',  ( 170.2234770963711128, 17.36149277827004411, -17.36149277826983095 ) ) ;
#13809 = CARTESIAN_POINT ( 'NONE',  ( 83.07250971316962307, -23.99533035190363961, -9.939191265417465004 ) ) ;
#13810 = ORIENTED_EDGE ( 'NONE', *, *, #10101, .T. ) ;
#13811 = CARTESIAN_POINT ( 'NONE',  ( 184.8905102610680444, -20.92133201514440799, -40.00000000000002132 ) ) ;
#13812 = CARTESIAN_POINT ( 'NONE',  ( -114.4364955367335881, -20.04994829326802019, 8.644468109231409514 ) ) ;
#13813 = ORIENTED_EDGE ( 'NONE', *, *, #14586, .F. ) ;
#13814 = CARTESIAN_POINT ( 'NONE',  ( 199.9999999999996874, 18.36026428565764945, 4.938082948735277533 ) ) ;
#13815 = AXIS2_PLACEMENT_3D ( 'NONE', #17651, #19656, #25411 ) ;
#13816 = DIRECTION ( 'NONE',  ( -1.000000000000000000, -0.000000000000000000, -0.000000000000000000 ) ) ;
#13817 = EDGE_CURVE ( 'NONE', #3201, #9561, #15350, .T. ) ;
#13818 = CARTESIAN_POINT ( 'NONE',  ( 184.8905102610680444, -14.79361573936389540, 41.77492675555996016 ) ) ;
#13819 = CARTESIAN_POINT ( 'NONE',  ( 190.0000000000000000, -52.49999999999991473, 52.49999999999999289 ) ) ;
#13820 = CARTESIAN_POINT ( 'NONE',  ( -198.0356074513804572, -9.007331120208026888E-14, 15.37879056873070560 ) ) ;
#13821 = CARTESIAN_POINT ( 'NONE',  ( -56.48582580120559982, -9.153146818113595984, 40.00000000000002132 ) ) ;
#13822 = CARTESIAN_POINT ( 'NONE',  ( 130.8568914410475088, -24.07718906446864793, -32.49135343045505664 ) ) ;
#13823 = CARTESIAN_POINT ( 'NONE',  ( 200.0000000000000000, 82.50000000000008527, 52.49999999999979394 ) ) ;
#13824 = CIRCLE ( 'NONE', #246, 30.00000000000000000 ) ;
#13825 = CARTESIAN_POINT ( 'NONE',  ( -208.1127848780265026, -9.061048840815752106E-14, 15.00245453012669472 ) ) ;
#13826 = CARTESIAN_POINT ( 'NONE',  ( -162.0762913951020892, -1.202636532414034422E-14, -1.694272876828323948 ) ) ;
#13827 = CARTESIAN_POINT ( 'NONE',  ( -370.0000000000001137, -4.857225732735059864E-14, 0.000000000000000000 ) ) ;
#13828 = CARTESIAN_POINT ( 'NONE',  ( 19.06497207195982568, -38.31983398719646061, 38.31983398719606271 ) ) ;
#13829 = CARTESIAN_POINT ( 'NONE',  ( 4.995406935893294431, -15.24977328854832415, -40.00000000000002132 ) ) ;
#13830 = CARTESIAN_POINT ( 'NONE',  ( -135.8532207217289738, -21.81201906317758343, -34.75652343174620995 ) ) ;
#13831 = CARTESIAN_POINT ( 'NONE',  ( -626.9846540392142060, 75.00000000000000000, 0.000000000000000000 ) ) ;
#13832 = CARTESIAN_POINT ( 'NONE',  ( -2.654373026594509355, -47.46285323120914512, 13.89837698318172343 ) ) ;
#13833 = CARTESIAN_POINT ( 'NONE',  ( 14.38125909742181108, 1.616281842095393922E-13, -15.17850393972633682 ) ) ;
#13834 = CARTESIAN_POINT ( 'NONE',  ( -91.56559293963834989, -39.99999999999995737, -22.67402823373205933 ) ) ;
#13835 = CARTESIAN_POINT ( 'NONE',  ( 170.2234770963711128, 10.92277846919201068, 10.92277846919202133 ) ) ;
#13836 = AXIS2_PLACEMENT_3D ( 'NONE', #24796, #10687, #6548 ) ;
#13837 = CARTESIAN_POINT ( 'NONE',  ( -192.9588430854689989, -10.23066800230742501, -10.23066800230756712 ) ) ;
#13838 = CARTESIAN_POINT ( 'NONE',  ( -188.3392995398617700, -23.45797413244939378, -43.01688924974088479 ) ) ;
#13839 = CARTESIAN_POINT ( 'NONE',  ( 199.9999999999999432, 14.14213562373113398, -14.14213562373094923 ) ) ;
#13840 = EDGE_LOOP ( 'NONE', ( #24515, #1928 ) ) ;
#13841 = CARTESIAN_POINT ( 'NONE',  ( 146.6084372240433709, -52.76785682606510619, -3.800685668859292043 ) ) ;
#13842 = CARTESIAN_POINT ( 'NONE',  ( -86.96347745069644475, 15.38646221621793586, -15.38646221621778842 ) ) ;
#13843 = CARTESIAN_POINT ( 'NONE',  ( -726.9846540392142060, 52.49999999999991473, -82.49999999999998579 ) ) ;
#13844 = EDGE_CURVE ( 'NONE', #10098, #19642, #22168, .T. ) ;
#13845 = CARTESIAN_POINT ( 'NONE',  ( -716.9846540392142060, 66.50000000000009948, 71.50000000000005684 ) ) ;
#13846 = CARTESIAN_POINT ( 'NONE',  ( -208.1127848780264742, -17.67593391476605547, -38.89260858015755673 ) ) ;
#13847 = CARTESIAN_POINT ( 'NONE',  ( 48.46027384457784137, -35.02097776273539864, 18.19770403991817886 ) ) ;
#13848 = ORIENTED_EDGE ( 'NONE', *, *, #11755, .T. ) ;
#13849 = CARTESIAN_POINT ( 'NONE',  ( 199.9999999999999432, 19.00129205762390683, 0.6358089133326541020 ) ) ;
#13850 = CARTESIAN_POINT ( 'NONE',  ( -210.0000000000000284, 52.50000000000007816, -52.49999999999999289 ) ) ;
#13851 = EDGE_CURVE ( 'NONE', #8803, #19588, #12733, .T. ) ;
#13852 = CARTESIAN_POINT ( 'NONE',  ( -4.004886986946478267, 23.45685150724344581, 43.01537795656734176 ) ) ;
#13853 = VECTOR ( 'NONE', #4241, 1000.000000000000000 ) ;
#13854 = ORIENTED_EDGE ( 'NONE', *, *, #17113, .F. ) ;
#13855 = VERTEX_POINT ( 'NONE', #8741 ) ;
#13856 = DIRECTION ( 'NONE',  ( 0.000000000000000000, 0.000000000000000000, -1.000000000000000000 ) ) ;
#13857 = CARTESIAN_POINT ( 'NONE',  ( 199.0108247880216368, -5.504876786518239307, -19.22761790364454271 ) ) ;
#13858 = CARTESIAN_POINT ( 'NONE',  ( 19.06497207195981858, -1.881589693694111225E-13, 54.19242893257843008 ) ) ;
#13859 = ADVANCED_FACE ( 'NONE', ( #8469 ), #6741, .F. ) ;
#13860 = EDGE_CURVE ( 'NONE', #19577, #16610, #22161, .T. ) ;
#13861 = SURFACE_SIDE_STYLE ('',( #7475 ) ) ;
#13862 = AXIS2_PLACEMENT_3D ( 'NONE', #10612, #102, #26204 ) ;
#13863 = CARTESIAN_POINT ( 'NONE',  ( 4.995406935893290878, 39.06748935135239265, -39.06748935135144762 ) ) ;
#13864 =( BOUNDED_SURFACE ( )  B_SPLINE_SURFACE ( 3, 3, ( 
 ( #12574, #24971, #8587, #14440, #24831, #20706, #22305, #22570, #18566, #24565, #20568, #4082, #2472, #10582, #482, #14704, #2214, #12183, #12708, #22441, #18834, #16439, #22835, #10323, #8316, #614, #6320, #20304, #4612, #2611 ),
 ( #8720, #18292, #18430, #78, #8187, #207, #16304, #24428, #6194, #4218, #12309, #3223, #13328, #11329, #7585, #1619, #11713, #23696, #13576, #19833, #9338, #21575, #1233, #19445, #5347, #9462, #3349, #15444, #17446, #9726 ),
 ( #11449, #25841, #25584, #1486, #21703, #19698, #21835, #19320, #22964, #17696, #17569, #13456, #7331, #25706, #15572, #23572, #7457, #19572, #21449, #17828, #1363, #5476, #3480, #3604, #10852, #15697, #23821, #4744, #1102, #9212 ),
 ( #11578, #25975, #9591, #14832, #5603, #13710, #12850, #20967, #2748, #17323, #25457, #7208, #15323, #23449, #5224, #3742, #20504, #14240, #14376, #1884, #2276, #7715, #22380, #12117, #23956, #20241, #13835, #12, #24233, #22242 ),
 ( #6263, #10385, #2022, #4017, #10124, #7983, #14114, #24092, #12251, #2148, #22509, #18225, #16240, #8123, #21970, #6006, #24369, #9857, #5731, #6132, #20373, #1749, #4156, #5867, #11847, #10258, #15967, #17960, #18367, #13973 ),
 ( #18496, #147, #15826, #19968, #8251, #22107, #16369, #24502, #4287, #3883, #26107, #12376, #11983, #7846, #20107, #9989, #18099, #26248, #16101, #12645, #8788, #679, #20633, #20770, #4547, #16506, #18632, #2540, #19034, #551 ),
 ( #16900, #276, #2938, #6519, #13047, #23162, #14767, #21031, #12505, #8655, #23037, #25164, #11048, #8919, #14897, #8384, #12778, #15032, #20905, #6652, #10922, #10658, #12914, #25032, #4812, #6915, #4411, #24631, #2814, #2683 ) ),
 .UNSPECIFIED., .T., .F., .T. ) 
 B_SPLINE_SURFACE_WITH_KNOTS ( ( 4, 3, 4 ),
 ( 4, 2, 2, 2, 2, 2, 2, 2, 2, 2, 2, 2, 2, 2, 4 ),
 ( 0.000000000000000000, 0.5000000000000000000, 1.000000000000000000 ),
 ( 0.000000000000000000, 0.1357259735107005372, 0.1651108541090157700, 0.1944957347073310028, 0.3598804999793158710, 0.3867117631979620773, 0.4135430264166082281, 0.5789277916885930964, 0.6062785021374117456, 0.6336292125862302838, 0.8508620842112317728, 0.8814014469398914198, 0.9119408096685510667, 0.9559704048342755334, 1.000000000000000000 ),
 .UNSPECIFIED. ) 
 GEOMETRIC_REPRESENTATION_ITEM ( )  RATIONAL_B_SPLINE_SURFACE ( (
 ( 1.000000000000000000, 1.000000000000000000, 1.000000000000000000, 1.000000000000000000, 1.000000000000000000, 1.000000000000000000, 1.000000000000000000, 1.000000000000000000, 1.000000000000000000, 1.000000000000000000, 1.000000000000000000, 1.000000000000000000, 1.000000000000000000, 1.000000000000000000, 1.000000000000000000, 1.000000000000000000, 1.000000000000000000, 1.000000000000000000, 1.000000000000000000, 1.000000000000000000, 1.000000000000000000, 1.000000000000000000, 1.000000000000000000, 1.000000000000000000, 1.000000000000000000, 1.000000000000000000, 1.000000000000000000, 1.000000000000000000, 1.000000000000000000, 1.000000000000000000),
 ( 0.3333333333333333703, 0.3333333333333333703, 0.3333333333333333703, 0.3333333333333333703, 0.3333333333333333703, 0.3333333333333333703, 0.3333333333333333703, 0.3333333333333333703, 0.3333333333333333703, 0.3333333333333333703, 0.3333333333333333703, 0.3333333333333333703, 0.3333333333333333703, 0.3333333333333333703, 0.3333333333333333703, 0.3333333333333333703, 0.3333333333333333703, 0.3333333333333333703, 0.3333333333333333703, 0.3333333333333333703, 0.3333333333333333703, 0.3333333333333333703, 0.3333333333333333703, 0.3333333333333333703, 0.3333333333333333703, 0.3333333333333333703, 0.3333333333333333703, 0.3333333333333333703, 0.3333333333333333703, 0.3333333333333333703),
 ( 0.3333333333333333703, 0.3333333333333333703, 0.3333333333333333703, 0.3333333333333333703, 0.3333333333333333703, 0.3333333333333333703, 0.3333333333333333703, 0.3333333333333333703, 0.3333333333333333703, 0.3333333333333333703, 0.3333333333333333703, 0.3333333333333333703, 0.3333333333333333703, 0.3333333333333333703, 0.3333333333333333703, 0.3333333333333333703, 0.3333333333333333703, 0.3333333333333333703, 0.3333333333333333703, 0.3333333333333333703, 0.3333333333333333703, 0.3333333333333333703, 0.3333333333333333703, 0.3333333333333333703, 0.3333333333333333703, 0.3333333333333333703, 0.3333333333333333703, 0.3333333333333333703, 0.3333333333333333703, 0.3333333333333333703),
 ( 1.000000000000000000, 1.000000000000000000, 1.000000000000000000, 1.000000000000000000, 1.000000000000000000, 1.000000000000000000, 1.000000000000000000, 1.000000000000000000, 1.000000000000000000, 1.000000000000000000, 1.000000000000000000, 1.000000000000000000, 1.000000000000000000, 1.000000000000000000, 1.000000000000000000, 1.000000000000000000, 1.000000000000000000, 1.000000000000000000, 1.000000000000000000, 1.000000000000000000, 1.000000000000000000, 1.000000000000000000, 1.000000000000000000, 1.000000000000000000, 1.000000000000000000, 1.000000000000000000, 1.000000000000000000, 1.000000000000000000, 1.000000000000000000, 1.000000000000000000),
 ( 0.3333333333333333703, 0.3333333333333333703, 0.3333333333333333703, 0.3333333333333333703, 0.3333333333333333703, 0.3333333333333333703, 0.3333333333333333703, 0.3333333333333333703, 0.3333333333333333703, 0.3333333333333333703, 0.3333333333333333703, 0.3333333333333333703, 0.3333333333333333703, 0.3333333333333333703, 0.3333333333333333703, 0.3333333333333333703, 0.3333333333333333703, 0.3333333333333333703, 0.3333333333333333703, 0.3333333333333333703, 0.3333333333333333703, 0.3333333333333333703, 0.3333333333333333703, 0.3333333333333333703, 0.3333333333333333703, 0.3333333333333333703, 0.3333333333333333703, 0.3333333333333333703, 0.3333333333333333703, 0.3333333333333333703),
 ( 0.3333333333333333703, 0.3333333333333333703, 0.3333333333333333703, 0.3333333333333333703, 0.3333333333333333703, 0.3333333333333333703, 0.3333333333333333703, 0.3333333333333333703, 0.3333333333333333703, 0.3333333333333333703, 0.3333333333333333703, 0.3333333333333333703, 0.3333333333333333703, 0.3333333333333333703, 0.3333333333333333703, 0.3333333333333333703, 0.3333333333333333703, 0.3333333333333333703, 0.3333333333333333703, 0.3333333333333333703, 0.3333333333333333703, 0.3333333333333333703, 0.3333333333333333703, 0.3333333333333333703, 0.3333333333333333703, 0.3333333333333333703, 0.3333333333333333703, 0.3333333333333333703, 0.3333333333333333703, 0.3333333333333333703),
 ( 1.000000000000000000, 1.000000000000000000, 1.000000000000000000, 1.000000000000000000, 1.000000000000000000, 1.000000000000000000, 1.000000000000000000, 1.000000000000000000, 1.000000000000000000, 1.000000000000000000, 1.000000000000000000, 1.000000000000000000, 1.000000000000000000, 1.000000000000000000, 1.000000000000000000, 1.000000000000000000, 1.000000000000000000, 1.000000000000000000, 1.000000000000000000, 1.000000000000000000, 1.000000000000000000, 1.000000000000000000, 1.000000000000000000, 1.000000000000000000, 1.000000000000000000, 1.000000000000000000, 1.000000000000000000, 1.000000000000000000, 1.000000000000000000, 1.000000000000000000) ) ) 
 REPRESENTATION_ITEM ( '' )  SURFACE ( )  );
#13865 = LINE ( 'NONE', #15722, #8310 ) ;
#13866 = CARTESIAN_POINT ( 'NONE',  ( -87.11181950073759594, -21.35018704950691060, -2.713672234369203018 ) ) ;
#13867 = CARTESIAN_POINT ( 'NONE',  ( -77.90255099906859471, -8.644468104251766150, 20.04994828524300843 ) ) ;
#13868 = CARTESIAN_POINT ( 'NONE',  ( 199.0214920807345322, 4.534629261753806873, 19.48466678343157454 ) ) ;
#13869 = CARTESIAN_POINT ( 'NONE',  ( -144.1957000270774927, 12.48102028655531903, 30.13184844817395458 ) ) ;
#13870 = CARTESIAN_POINT ( 'NONE',  ( -4.112199523540041923, -23.43514144949427447, -42.98379141459099628 ) ) ;
#13871 = CARTESIAN_POINT ( 'NONE',  ( 170.2234770963711128, 17.36149277827028925, -39.20704971665377059 ) ) ;
#13872 = AXIS2_PLACEMENT_3D ( 'NONE', #21151, #19521, #13033 ) ;
#13873 = DIRECTION ( 'NONE',  ( 1.000000000000000000, 1.836970198721030181E-16, 0.000000000000000000 ) ) ;
#13874 = CARTESIAN_POINT ( 'NONE',  ( 14.38125909742181818, -39.01709431150904095, -17.55144818341490165 ) ) ;
#13875 = CARTESIAN_POINT ( 'NONE',  ( -259.2033419157646676, -40.00000000000017053, 9.517827891722212996 ) ) ;
#13876 = DIRECTION ( 'NONE',  ( 0.000000000000000000, -1.000000000000000000, 0.000000000000000000 ) ) ;
#13877 = CARTESIAN_POINT ( 'NONE',  ( -91.56559293963836410, 16.03295912088692177, 16.03295912088721664 ) ) ;
#13878 = CARTESIAN_POINT ( 'NONE',  ( -198.0356074513804288, -55.37879056873077133, -2.449293598294708485E-15 ) ) ;
#13879 = CARTESIAN_POINT ( 'NONE',  ( -162.0762913951021176, 27.08623940707598265, 29.48230308784781428 ) ) ;
#13880 = CARTESIAN_POINT ( 'NONE',  ( 136.1360204305621551, -4.966164525587036138, -40.00000000000002132 ) ) ;
#13881 = CARTESIAN_POINT ( 'NONE',  ( -89.92902785008674016, 20.44110050034136705, -8.088236460649897097 ) ) ;
#13882 = DIRECTION ( 'NONE',  ( -1.000000000000000000, 0.000000000000000000, -0.000000000000000000 ) ) ;
#13883 = CARTESIAN_POINT ( 'NONE',  ( 151.7948205124836534, 4.785054706298574878, -51.78348778862537927 ) ) ;
#13884 = CARTESIAN_POINT ( 'NONE',  ( 146.6084372240433709, -34.62501878078303008, -40.00000000000002132 ) ) ;
#13885 = VERTEX_POINT ( 'NONE', #20855 ) ;
#13886 = CARTESIAN_POINT ( 'NONE',  ( 23.36462152323021613, -42.86003749000681040, 23.34178792078220965 ) ) ;
#13887 = CARTESIAN_POINT ( 'NONE',  ( 135.5356265174576151, 12.51227922893862399, 30.20731421070357925 ) ) ;
#13888 = CIRCLE ( 'NONE', #3644, 6.000000000000005329 ) ;
#13889 = CARTESIAN_POINT ( 'NONE',  ( 184.8905102610680444, 13.49065550809807945, 13.49065550809809544 ) ) ;
#13890 = CARTESIAN_POINT ( 'NONE',  ( 4.995406935893305089, -40.00000000000021316, 55.24977328853194791 ) ) ;
#13891 = CARTESIAN_POINT ( 'NONE',  ( 146.6084372240433993, -24.48358557860353457, 24.48358557860296258 ) ) ;
#13892 = CARTESIAN_POINT ( 'NONE',  ( -56.48582580120559271, -9.153146818113595984, 0.000000000000000000 ) ) ;
#13893 = CARTESIAN_POINT ( 'NONE',  ( 57.59792236341147031, -2.435789363418150444, 0.000000000000000000 ) ) ;
#13894 = CARTESIAN_POINT ( 'NONE',  ( -210.0000000000000284, 1.836970198721030378E-15, 0.000000000000000000 ) ) ;
#13895 = CARTESIAN_POINT ( 'NONE',  ( 199.9999999999995168, 19.00182775553472325, -0.6082061139381043091 ) ) ;
#13896 = CARTESIAN_POINT ( 'NONE',  ( 200.0000000000000284, -16.14727532946531241, -10.03029091962484642 ) ) ;
#13897 = B_SPLINE_CURVE_WITH_KNOTS ( 'NONE', 3,
 ( #11250, #7130, #9125, #21248, #1026, #16982, #897, #6995, #7378, #5269, #15489, #10874, #15242, #5149, #25244, #4890, #1276, #19369, #1156, #21120, #20984, #17367, #25504, #2897, #15116, #23247 ),
 .UNSPECIFIED., .F., .F.,
 ( 4, 2, 1, 2, 2, 2, 2, 2, 2, 2, 2, 1, 2, 4 ),
 ( -5.999999998908891326E-08, 0.0004354487530732538848, 0.0008709575061464967880, 0.001741975012292981727, 0.003484010024585949654, 0.006968080049171881604, 0.01045215007375781269, 0.01393622009834374550, 0.02090436014751561114, 0.02438843017210155090, 0.02613046518439452251, 0.02700148269054100658, 0.02743699144361424341, 0.02787250019668748025 ),
 .UNSPECIFIED. ) ;
#13898 = CARTESIAN_POINT ( 'NONE',  ( -86.96347745069644475, 12.89780903124419353, -12.89780903124389333 ) ) ;
#13899 = CARTESIAN_POINT ( 'NONE',  ( 0.2972598230770027716, -38.42060263243681817, 18.14793986248684377 ) ) ;
#13900 = CARTESIAN_POINT ( 'NONE',  ( -114.4364955367327781, 20.29001642038848274, -8.064892380842206165 ) ) ;
#13901 = CARTESIAN_POINT ( 'NONE',  ( -87.13368444204334651, 14.72469439730582152, -15.67192210925590068 ) ) ;
#13902 = CARTESIAN_POINT ( 'NONE',  ( 19.06497207195981858, -10.03556273973377166, -66.60410523465827737 ) ) ;
#13904 = CARTESIAN_POINT ( 'NONE',  ( -77.90255099907052738, 8.064892378688679031, 20.29001641119211641 ) ) ;
#13903 = CARTESIAN_POINT ( 'NONE',  ( -280.0000000000000568, -42.42640687119305198, 14.14213562373058686 ) ) ;
#13905 = CARTESIAN_POINT ( 'NONE',  ( 4.995406935893297984, 10.78321810390233892, -67.35176059882522281 ) ) ;
#13906 = DIRECTION ( 'NONE',  ( -1.000000000000000000, 0.000000000000000000, 0.000000000000000000 ) ) ;
#13907 = CARTESIAN_POINT ( 'NONE',  ( 199.0238599485892621, -1.396734769875851212, 20.00262899750501333 ) ) ;
#13909 = CARTESIAN_POINT ( 'NONE',  ( -238.4067589809705794, -40.00000000000021316, 40.96449427990166470 ) ) ;
#13908 = CARTESIAN_POINT ( 'NONE',  ( -238.4067589809705794, 28.96627169325285678, 27.60227080167094726 ) ) ;
#13910 = CARTESIAN_POINT ( 'NONE',  ( -280.0000000000000000, 14.14213562373098299, -14.14213562373088706 ) ) ;
#13911 = CARTESIAN_POINT ( 'NONE',  ( -105.3755690713226727, 15.38646221621771737, 15.38646221621800514 ) ) ;
#13912 = CARTESIAN_POINT ( 'NONE',  ( 184.8905102610680444, 19.07866798485561333, 40.00000000000002132 ) ) ;
#13913 = ORIENTED_EDGE ( 'NONE', *, *, #21209, .T. ) ;
#13914 = CARTESIAN_POINT ( 'NONE',  ( 184.8905102610680444, -14.79361573936379415, -14.79361573936387941 ) ) ;
#13915 = CARTESIAN_POINT ( 'NONE',  ( 9.807832026182905949, 43.71718838542761176, 18.10825233806385270 ) ) ;
#13916 = CARTESIAN_POINT ( 'NONE',  ( 23.46661716382963192, 13.79413593526274262, 46.77475180958831658 ) ) ;
#13917 = CARTESIAN_POINT ( 'NONE',  ( -105.3220005116004785, -5.373930277592323890, 20.73876282934741866 ) ) ;
#13918 = ORIENTED_EDGE ( 'NONE', *, *, #12873, .F. ) ;
#13919 = CARTESIAN_POINT ( 'NONE',  ( -191.2489946133628393, -43.85245824699192241, 18.16428294931126786 ) ) ;
#13920 = CARTESIAN_POINT ( 'NONE',  ( 199.9999999999997158, -17.84428681738966205, -6.548952533294360556 ) ) ;
#13921 = EDGE_CURVE ( 'NONE', #9443, #15984, #24720, .T. ) ;
#13922 = CARTESIAN_POINT ( 'NONE',  ( 13.28449813596001228, -14.15462405556703018, 49.16593779330992220 ) ) ;
#13923 = CARTESIAN_POINT ( 'NONE',  ( 25.88393124174635318, 22.82896322164242875, -42.08451360837176480 ) ) ;
#13924 = CARTESIAN_POINT ( 'NONE',  ( 199.0170773700648397, -15.56690153483635264, -12.55869779031424116 ) ) ;
#13925 = CARTESIAN_POINT ( 'NONE',  ( 135.5356265174576151, -30.20731421070357214, 12.51227922893874656 ) ) ;
#13926 = CARTESIAN_POINT ( 'NONE',  ( -121.8425463767455597, -9.420908037836060345, 22.74408395719867571 ) ) ;
#13927 = CARTESIAN_POINT ( 'NONE',  ( 146.6084372240433709, 32.08495691632030145, 24.48358557860365181 ) ) ;
#13928 = CARTESIAN_POINT ( 'NONE',  ( 19.06497207195982924, -54.19242893257843008, 40.00000000000002132 ) ) ;
#13930 = CARTESIAN_POINT ( 'NONE',  ( -192.9588430854689989, 10.23066800230756712, -10.23066800230735396 ) ) ;
#13929 = CARTESIAN_POINT ( 'NONE',  ( 90.68848816920421996, -8.337973095858520978, -21.47805809303278934 ) ) ;
#13931 = CARTESIAN_POINT ( 'NONE',  ( 57.59792236341147031, 2.435789363418171760, 0.000000000000000000 ) ) ;
#13932 = EDGE_CURVE ( 'NONE', #10135, #22711, #16719, .T. ) ;
#13933 = CARTESIAN_POINT ( 'NONE',  ( -91.56559293963836410, 22.67402823373189946, -0.000000000000000000 ) ) ;
#13934 = CARTESIAN_POINT ( 'NONE',  ( -100.7734535825088500, -22.67402823373193499, 40.00000000000002132 ) ) ;
#13935 = CARTESIAN_POINT ( 'NONE',  ( 4.995406935893298872, 5.820775922023080204E-13, -55.24977328854835434 ) ) ;
#13936 = CARTESIAN_POINT ( 'NONE',  ( -135.8532207217289738, -1.208299557080134822E-13, 9.153146818113572891 ) ) ;
#13937 = CARTESIAN_POINT ( 'NONE',  ( -30.26275506840325136, 27.08623969584614244, -29.48230279907770779 ) ) ;
#13938 = ADVANCED_FACE ( 'NONE', ( #25247 ), #2306, .T. ) ;
#13939 = ORIENTED_EDGE ( 'NONE', *, *, #13600, .T. ) ;
#13940 = CARTESIAN_POINT ( 'NONE',  ( 98.29820294267416614, 12.20973600806160775, -15.89413956777835679 ) ) ;
#13941 = CARTESIAN_POINT ( 'NONE',  ( 184.8905102610680444, 20.92133201514447549, 0.000000000000000000 ) ) ;
#13942 = CARTESIAN_POINT ( 'NONE',  ( -189.4799703873391081, 47.39666448643376384, -13.88847319136868563 ) ) ;
#13943 = SHAPE_DEFINITION_REPRESENTATION ( #3569, #3691 ) ;
#13944 = EDGE_LOOP ( 'NONE', ( #6797, #17804, #17174, #8293, #5084, #3759 ) ) ;
#13945 = ORIENTED_EDGE ( 'NONE', *, *, #16296, .F. ) ;
#13946 = CARTESIAN_POINT ( 'NONE',  ( 4.995406935893297984, -39.06748935135182421, -17.50105314357212549 ) ) ;
#13947 = CARTESIAN_POINT ( 'NONE',  ( 23.32574057153218305, -42.87194976637074717, -23.35062444423069294 ) ) ;
#13948 = VERTEX_POINT ( 'NONE', #366 ) ;
#13949 = CARTESIAN_POINT ( 'NONE',  ( -100.7734535825088500, -22.67402823373193499, -40.00000000000002132 ) ) ;
#13950 = CARTESIAN_POINT ( 'NONE',  ( -114.4364955367322949, 8.644468109217019247, 20.04994829327305794 ) ) ;
#13951 = CIRCLE ( 'NONE', #2497, 28.79780246617542616 ) ;
#13953 = ORIENTED_EDGE ( 'NONE', *, *, #4520, .T. ) ;
#13952 = EDGE_CURVE ( 'NONE', #854, #24980, #15553, .T. ) ;
#13954 = CARTESIAN_POINT ( 'NONE',  ( 199.9999999999996021, 18.99368777275013898, 0.6330478706754758544 ) ) ;
#13955 = CARTESIAN_POINT ( 'NONE',  ( -105.4741150117367283, 19.77569912955882359, -7.943527260733686646 ) ) ;
#13956 = CARTESIAN_POINT ( 'NONE',  ( -162.0762913951021176, 29.48230308784768638, -27.08623940707612121 ) ) ;
#13957 = CARTESIAN_POINT ( 'NONE',  ( -189.0540493709901568, -43.34488811517300633, -17.95404051684990776 ) ) ;
#13958 = CARTESIAN_POINT ( 'NONE',  ( 57.59792236341149163, -40.00000000000014211, 37.56421063658172699 ) ) ;
#13959 = CARTESIAN_POINT ( 'NONE',  ( -91.56559293963834989, -22.67402823373193499, 40.00000000000002132 ) ) ;
#13960 = CARTESIAN_POINT ( 'NONE',  ( 91.82158438592158234, 16.11829626346161604, -16.11829626346121103 ) ) ;
#13961 = DIRECTION ( 'NONE',  ( 0.000000000000000000, 0.000000000000000000, 1.000000000000000000 ) ) ;
#13962 = CARTESIAN_POINT ( 'NONE',  ( 91.82158438592158234, 7.693928927950222250E-14, -17.20528682183300262 ) ) ;
#13963 = CARTESIAN_POINT ( 'NONE',  ( 4.995406935893306866, -39.99999999999944578, -55.24977328856505920 ) ) ;
#13964 = FACE_BOUND ( 'NONE', #19672, .T. ) ;
#13965 = CARTESIAN_POINT ( 'NONE',  ( -105.3755690713226585, 15.38646221621762678, 41.18208027870604582 ) ) ;
#13966 = CARTESIAN_POINT ( 'NONE',  ( -91.56559293963836410, 22.67402823373189946, -0.000000000000000000 ) ) ;
#13967 = CARTESIAN_POINT ( 'NONE',  ( -91.56559293963836410, -12.25131212657462321, -44.31723036834905827 ) ) ;
#13968 = FACE_BOUND ( 'NONE', #24411, .T. ) ;
#13969 = AXIS2_PLACEMENT_3D ( 'NONE', #2210, #10319, #18426 ) ;
#13970 = DIRECTION ( 'NONE',  ( -0.000000000000000000, 0.000000000000000000, -1.000000000000000000 ) ) ;
#13971 = CARTESIAN_POINT ( 'NONE',  ( -100.7734535825088358, -2.560096224687585342E-13, 22.67402823373191723 ) ) ;
#13972 = CARTESIAN_POINT ( 'NONE',  ( 57.59792236341147031, 1.908507979671054758E-14, -2.435789363418160658 ) ) ;
#13973 = CARTESIAN_POINT ( 'NONE',  ( 200.0000000000000000, 42.42640687119288856, -14.14213562373094746 ) ) ;
#13974 = FACE_OUTER_BOUND ( 'NONE', #20644, .T. ) ;
#13975 = CARTESIAN_POINT ( 'NONE',  ( -188.9478905404521640, -17.94277290414830262, -43.31768569177597783 ) ) ;
#13976 = DIRECTION ( 'NONE',  ( 1.000000000000000000, -1.836970198721030181E-16, -0.000000000000000000 ) ) ;
#13977 = ORIENTED_EDGE ( 'NONE', *, *, #11560, .T. ) ;
#13978 = VECTOR ( 'NONE', #19439, 1000.000000000000000 ) ;
#13979 = CARTESIAN_POINT ( 'NONE',  ( 200.0000000000000000, -42.42640687119272513, -14.14213562373140753 ) ) ;
#13980 = CARTESIAN_POINT ( 'NONE',  ( -87.11144460458852734, -13.16695842547661499, -17.02332938628118342 ) ) ;
#13981 = CARTESIAN_POINT ( 'NONE',  ( 163.1118516004056573, 19.27778845538780317, -19.27778845538757224 ) ) ;
#13982 = CARTESIAN_POINT ( 'NONE',  ( -77.90255099906769942, -20.29001641120677846, -8.064892378658084837 ) ) ;
#13983 = DIRECTION ( 'NONE',  ( 0.000000000000000000, -0.3995982397846142287, 0.9166903767145360149 ) ) ;
#13984 = CARTESIAN_POINT ( 'NONE',  ( -162.0762913951020892, 1.198031840456041497, -57.76657433537918251 ) ) ;
#13985 =( NAMED_UNIT ( * ) SI_UNIT ( $, .STERADIAN. ) SOLID_ANGLE_UNIT ( ) );
#13986 = LINE ( 'NONE', #1496, #19807 ) ;
#13987 = ORIENTED_EDGE ( 'NONE', *, *, #22836, .T. ) ;
#13988 = CARTESIAN_POINT ( 'NONE',  ( 199.9999999999999432, 12.98018377190829753, 13.88592919840850648 ) ) ;
#13989 = CARTESIAN_POINT ( 'NONE',  ( -210.0000000000000284, -71.50000000000002842, 66.50000000000005684 ) ) ;
#13990 = CARTESIAN_POINT ( 'NONE',  ( 3.468680970031286392, 14.11592159093371812, 48.91035688725572328 ) ) ;
#13991 = VERTEX_POINT ( 'NONE', #14987 ) ;
#13992 = ORIENTED_EDGE ( 'NONE', *, *, #9534, .T. ) ;
#13993 = PRODUCT_DEFINITION_SHAPE ( 'NONE', 'NONE',  #26359 ) ;
#13994 = CARTESIAN_POINT ( 'NONE',  ( -259.2033419157646676, -6.730120644403570829, -6.730120644403545960 ) ) ;
#13995 = CARTESIAN_POINT ( 'NONE',  ( 199.0080442515877905, 1.130919702028742257, -19.96471691786700120 ) ) ;
#13996 = FACE_OUTER_BOUND ( 'NONE', #26111, .T. ) ;
#13997 = EDGE_CURVE ( 'NONE', #17170, #16549, #2857, .T. ) ;
#13998 = FACE_BOUND ( 'NONE', #8094, .T. ) ;
#13999 = AXIS2_PLACEMENT_3D ( 'NONE', #11483, #7367, #4163 ) ;
#14000 = CARTESIAN_POINT ( 'NONE',  ( -213.1075012329537230, 40.00000000000012790, -13.71589010951869980 ) ) ;
#14001 = CARTESIAN_POINT ( 'NONE',  ( 199.9999999999998295, -17.79330310134281135, 6.698924172861754123 ) ) ;
#14002 = CARTESIAN_POINT ( 'NONE',  ( -637.8274243086653996, 28.58169946791086957, -27.98848419961302980 ) ) ;
#14003 = FACE_OUTER_BOUND ( 'NONE', #15036, .T. ) ;
#14004 = CARTESIAN_POINT ( 'NONE',  ( 199.0183491629479988, 10.55513269831597079, 16.99244513920028510 ) ) ;
#14005 = CARTESIAN_POINT ( 'NONE',  ( -184.2925746397123135, 41.26799595407793220, 17.09376361613362150 ) ) ;
#14006 = CARTESIAN_POINT ( 'NONE',  ( -4.201409602818406697, -23.41774994521158249, -42.95750343186449527 ) ) ;
#14007 = ADVANCED_FACE ( 'NONE', ( #21251 ), #5184, .T. ) ;
#14008 = CARTESIAN_POINT ( 'NONE',  ( 170.2234770963711128, -10.92277846919187034, -10.92277846919209594 ) ) ;
#14009 = CARTESIAN_POINT ( 'NONE',  ( -114.7826396787322665, -15.64922767586156915, -15.64922767586183383 ) ) ;
#14010 = CARTESIAN_POINT ( 'NONE',  ( 136.1360204305621551, -31.79587985999244282, -24.77266263493140386 ) ) ;
#14011 = CARTESIAN_POINT ( 'NONE',  ( -105.3755690713226585, -40.00000000000027711, 21.75974354311608749 ) ) ;
#14012 = CARTESIAN_POINT ( 'NONE',  ( -280.0000000000000000, 14.14213562373078581, 14.14213562373108424 ) ) ;
#14013 = CARTESIAN_POINT ( 'NONE',  ( -30.26275506840323004, -41.69427246844629309, 40.00000000000002132 ) ) ;
#14014 = EDGE_CURVE ( 'NONE', #8031, #11219, #11310, .T. ) ;
#14015 = DIRECTION ( 'NONE',  ( 1.000000000000000000, 0.000000000000000000, -0.000000000000000000 ) ) ;
#14016 = CARTESIAN_POINT ( 'NONE',  ( 57.59792236341148453, -37.56421063658185489, -40.00000000000002132 ) ) ;
#14017 = CARTESIAN_POINT ( 'NONE',  ( -103.9474983245025044, 20.15710290851490427, -8.027156558344678672 ) ) ;
#14018 = AXIS2_PLACEMENT_3D ( 'NONE', #18655, #22795, #4966 ) ;
#14019 = CARTESIAN_POINT ( 'NONE',  ( -192.9588430854690273, 40.00000000000055422, -54.46834944101679810 ) ) ;
#14020 = CARTESIAN_POINT ( 'NONE',  ( -238.4067589809705794, 28.96627169325324758, -27.60227080167054581 ) ) ;
#14021 = CARTESIAN_POINT ( 'NONE',  ( 170.2234770963711128, 15.44714144992819627, -40.00000000000002132 ) ) ;
#14022 = VERTEX_POINT ( 'NONE', #23498 ) ;
#14023 = AXIS2_PLACEMENT_3D ( 'NONE', #17576, #25464, #3488 ) ;
#14024 = CARTESIAN_POINT ( 'NONE',  ( -208.1127848780264742, 15.00245453012665742, 40.00000000000002132 ) ) ;
#14025 = DIRECTION ( 'NONE',  ( 1.000000000000000000, 0.000000000000000000, 0.000000000000000000 ) ) ;
#14026 =( BOUNDED_SURFACE ( )  B_SPLINE_SURFACE ( 3, 3, ( 
 ( #4773, #18999, #6750, #2644, #9020, #7006, #7139, #12877, #21132, #10751, #25387, #21259, #4638, #9135, #24997, #15254, #20993, #14862, #510, #23257, #8615, #24857, #14729, #6611, #5033, #11140, #13140, #2907, #22861, #3031 ),
 ( #12740, #20860, #643, #8749, #2775, #11015, #10887, #16993, #19125, #8882, #25128, #907, #14994, #23129, #4901, #19896, #21631, #21386, #19379, #3670, #17501, #9786, #23384, #3536, #1417, #13264, #9518, #3158, #15626, #13508 ),
 ( #5531, #15498, #13766, #5158, #19634, #11508, #23628, #3407, #11260, #13383, #9394, #11778, #17624, #13637, #25768, #1166, #7518, #11380, #9269, #1681, #23749, #7774, #17888, #21763, #21510, #17377, #11636, #5278, #15382, #25516 ),
 ( #5407, #1286, #7263, #19759, #23504, #1549, #3282, #9653, #25641, #19501, #17758, #7387, #25899, #7640, #15755, #21893, #23883, #5660, #26037, #9917, #20036, #1814, #18023, #22037, #15889, #3809, #26172, #24017, #11914, #5796 ),
 ( #13903, #20758, #20892, #12631, #4800, #2528, #10774, #537, #21153, #3053, #13160, #17145, #18755, #22756, #10645, #14619, #4534, #6773, #2800, #16888, #12765, #19146, #931, #17274, #23025, #23150, #2669, #9162, #5054, #14754 ),
 ( #8642, #1056, #21280, #18887, #12901, #16751, #25020, #25408, #9040, #25279, #11158, #24885, #19273, #23278, #6640, #7033, #22884, #13035, #4663, #801, #2927, #666, #8775, #14885, #21017, #19022, #10911, #8906, #4924, #17016 ),
 ( #25152, #6903, #15150, #15020, #11036, #8925, #684, #8793, #2943, #17162, #21170, #22902, #13052, #23042, #24902, #15290, #9057, #19417, #21419, #4946, #6790, #6657, #15037, #16905, #25037, #14772, #4680, #12783, #20910, #19289 ) ),
 .UNSPECIFIED., .T., .F., .F. ) 
 B_SPLINE_SURFACE_WITH_KNOTS ( ( 4, 3, 4 ),
 ( 4, 2, 2, 2, 2, 2, 2, 2, 2, 2, 2, 2, 2, 2, 4 ),
 ( 0.000000000000000000, 0.5000000000000000000, 1.000000000000000000 ),
 ( 0.000000000000000000, 0.1357259735107005372, 0.1651108541090157700, 0.1944957347073310028, 0.3598804999793158710, 0.3867117631979620773, 0.4135430264166082281, 0.5789277916885930964, 0.6062785021374117456, 0.6336292125862302838, 0.8508620842112317728, 0.8814014469398914198, 0.9119408096685510667, 0.9559704048342755334, 1.000000000000000000 ),
 .UNSPECIFIED. ) 
 GEOMETRIC_REPRESENTATION_ITEM ( )  RATIONAL_B_SPLINE_SURFACE ( (
 ( 1.000000000000000000, 1.000000000000000000, 1.000000000000000000, 1.000000000000000000, 1.000000000000000000, 1.000000000000000000, 1.000000000000000000, 1.000000000000000000, 1.000000000000000000, 1.000000000000000000, 1.000000000000000000, 1.000000000000000000, 1.000000000000000000, 1.000000000000000000, 1.000000000000000000, 1.000000000000000000, 1.000000000000000000, 1.000000000000000000, 1.000000000000000000, 1.000000000000000000, 1.000000000000000000, 1.000000000000000000, 1.000000000000000000, 1.000000000000000000, 1.000000000000000000, 1.000000000000000000, 1.000000000000000000, 1.000000000000000000, 1.000000000000000000, 1.000000000000000000),
 ( 0.3333333333333333703, 0.3333333333333333703, 0.3333333333333333703, 0.3333333333333333703, 0.3333333333333333703, 0.3333333333333333703, 0.3333333333333333703, 0.3333333333333333703, 0.3333333333333333703, 0.3333333333333333703, 0.3333333333333333703, 0.3333333333333333703, 0.3333333333333333703, 0.3333333333333333703, 0.3333333333333333703, 0.3333333333333333703, 0.3333333333333333703, 0.3333333333333333703, 0.3333333333333333703, 0.3333333333333333703, 0.3333333333333333703, 0.3333333333333333703, 0.3333333333333333703, 0.3333333333333333703, 0.3333333333333333703, 0.3333333333333333703, 0.3333333333333333703, 0.3333333333333333703, 0.3333333333333333703, 0.3333333333333333703),
 ( 0.3333333333333333703, 0.3333333333333333703, 0.3333333333333333703, 0.3333333333333333703, 0.3333333333333333703, 0.3333333333333333703, 0.3333333333333333703, 0.3333333333333333703, 0.3333333333333333703, 0.3333333333333333703, 0.3333333333333333703, 0.3333333333333333703, 0.3333333333333333703, 0.3333333333333333703, 0.3333333333333333703, 0.3333333333333333703, 0.3333333333333333703, 0.3333333333333333703, 0.3333333333333333703, 0.3333333333333333703, 0.3333333333333333703, 0.3333333333333333703, 0.3333333333333333703, 0.3333333333333333703, 0.3333333333333333703, 0.3333333333333333703, 0.3333333333333333703, 0.3333333333333333703, 0.3333333333333333703, 0.3333333333333333703),
 ( 1.000000000000000000, 1.000000000000000000, 1.000000000000000000, 1.000000000000000000, 1.000000000000000000, 1.000000000000000000, 1.000000000000000000, 1.000000000000000000, 1.000000000000000000, 1.000000000000000000, 1.000000000000000000, 1.000000000000000000, 1.000000000000000000, 1.000000000000000000, 1.000000000000000000, 1.000000000000000000, 1.000000000000000000, 1.000000000000000000, 1.000000000000000000, 1.000000000000000000, 1.000000000000000000, 1.000000000000000000, 1.000000000000000000, 1.000000000000000000, 1.000000000000000000, 1.000000000000000000, 1.000000000000000000, 1.000000000000000000, 1.000000000000000000, 1.000000000000000000),
 ( 0.3333333333333333703, 0.3333333333333333703, 0.3333333333333333703, 0.3333333333333333703, 0.3333333333333333703, 0.3333333333333333703, 0.3333333333333333703, 0.3333333333333333703, 0.3333333333333333703, 0.3333333333333333703, 0.3333333333333333703, 0.3333333333333333703, 0.3333333333333333703, 0.3333333333333333703, 0.3333333333333333703, 0.3333333333333333703, 0.3333333333333333703, 0.3333333333333333703, 0.3333333333333333703, 0.3333333333333333703, 0.3333333333333333703, 0.3333333333333333703, 0.3333333333333333703, 0.3333333333333333703, 0.3333333333333333703, 0.3333333333333333703, 0.3333333333333333703, 0.3333333333333333703, 0.3333333333333333703, 0.3333333333333333703),
 ( 0.3333333333333333703, 0.3333333333333333703, 0.3333333333333333703, 0.3333333333333333703, 0.3333333333333333703, 0.3333333333333333703, 0.3333333333333333703, 0.3333333333333333703, 0.3333333333333333703, 0.3333333333333333703, 0.3333333333333333703, 0.3333333333333333703, 0.3333333333333333703, 0.3333333333333333703, 0.3333333333333333703, 0.3333333333333333703, 0.3333333333333333703, 0.3333333333333333703, 0.3333333333333333703, 0.3333333333333333703, 0.3333333333333333703, 0.3333333333333333703, 0.3333333333333333703, 0.3333333333333333703, 0.3333333333333333703, 0.3333333333333333703, 0.3333333333333333703, 0.3333333333333333703, 0.3333333333333333703, 0.3333333333333333703),
 ( 1.000000000000000000, 1.000000000000000000, 1.000000000000000000, 1.000000000000000000, 1.000000000000000000, 1.000000000000000000, 1.000000000000000000, 1.000000000000000000, 1.000000000000000000, 1.000000000000000000, 1.000000000000000000, 1.000000000000000000, 1.000000000000000000, 1.000000000000000000, 1.000000000000000000, 1.000000000000000000, 1.000000000000000000, 1.000000000000000000, 1.000000000000000000, 1.000000000000000000, 1.000000000000000000, 1.000000000000000000, 1.000000000000000000, 1.000000000000000000, 1.000000000000000000, 1.000000000000000000, 1.000000000000000000, 1.000000000000000000, 1.000000000000000000, 1.000000000000000000) ) ) 
 REPRESENTATION_ITEM ( '' )  SURFACE ( )  );
#14027 = CARTESIAN_POINT ( 'NONE',  ( 4.995406935893287326, 67.35176059882533650, 10.78321810390163549 ) ) ;
#14028 = CARTESIAN_POINT ( 'NONE',  ( 146.6084372240433709, -39.99999999999987921, -34.62501878078319351 ) ) ;
#14029 = CARTESIAN_POINT ( 'NONE',  ( 151.7948205124836534, 4.785054706297857230, 51.78348778862544322 ) ) ;
#14030 = CARTESIAN_POINT ( 'NONE',  ( -208.1127848780265026, 15.00245453012665564, 0.000000000000000000 ) ) ;
#14031 = CARTESIAN_POINT ( 'NONE',  ( 130.8568914410475372, -34.05028731879786363, 0.000000000000000000 ) ) ;
#14032 = CARTESIAN_POINT ( 'NONE',  ( 199.9999999999999432, -2.560943207453569512E-14, 6.234883604895477860E-14 ) ) ;
#14033 = CARTESIAN_POINT ( 'NONE',  ( 199.9999999999998010, 17.44192585402499418, -7.542491233669909256 ) ) ;
#14034 = CARTESIAN_POINT ( 'NONE',  ( 199.9999999999999716, -16.46561772086350217, -9.499012046328999759 ) ) ;
#14035 = CARTESIAN_POINT ( 'NONE',  ( -280.0000000000000000, 14.14213562373108246, -14.14213562373078581 ) ) ;
#14036 = CARTESIAN_POINT ( 'NONE',  ( 19.06497207195982924, -66.60410523465809263, -10.03556273973493163 ) ) ;
#14037 = AXIS2_PLACEMENT_3D ( 'NONE', #14652, #25187, #7072 ) ;
#14038 = CARTESIAN_POINT ( 'NONE',  ( 170.2234770963711128, -39.20704971665404059, 17.36149277826957160 ) ) ;
#14039 = CARTESIAN_POINT ( 'NONE',  ( -726.9846540392142060, -66.50000000000001421, 61.50000000000005684 ) ) ;
#14040 = CARTESIAN_POINT ( 'NONE',  ( -135.8532207217289738, -34.75652343174584757, -21.81201906317816253 ) ) ;
#14041 = ADVANCED_FACE ( 'NONE', ( #1279 ), #18982, .F. ) ;
#14042 = CARTESIAN_POINT ( 'NONE',  ( -280.0000000000000568, -14.14213562373078226, -42.42640687119295251 ) ) ;
#14043 = CARTESIAN_POINT ( 'NONE',  ( 199.0233509355391277, -0.007210440545907509553, 20.00363007596296328 ) ) ;
#14045 = CARTESIAN_POINT ( 'NONE',  ( -56.48582580120557850, -40.00000000000014211, 30.84685318188629921 ) ) ;
#14044 = CARTESIAN_POINT ( 'NONE',  ( -105.3755690713226727, 12.89780903124418998, -12.89780903124389155 ) ) ;
#14046 = B_SPLINE_CURVE_WITH_KNOTS ( 'NONE', 3,
 ( #1571, #23649, #7286, #15401, #23526, #17523, #7538, #23775, #5553, #7407, #11661, #19785 ),
 .UNSPECIFIED., .F., .F.,
 ( 4, 2, 2, 2, 2, 4 ),
 ( 5.045153280873417672E-16, 0.004698945756007614528, 0.007048418634011168957, 0.009397891512014724252, 0.01409683726802183311, 0.01879578302402894197 ),
 .UNSPECIFIED. ) ;
#14047 = CARTESIAN_POINT ( 'NONE',  ( -100.7734535825088500, 16.03295912088691821, 16.03295912088721309 ) ) ;
#14048 = CARTESIAN_POINT ( 'NONE',  ( 2.303792037526079639, 44.43800799081192565, -18.40682559463163415 ) ) ;
#14049 = CARTESIAN_POINT ( 'NONE',  ( 184.8905102610680444, 19.07866798485562043, 2.449293598294708485E-15 ) ) ;
#14050 = ORIENTED_EDGE ( 'NONE', *, *, #7185, .F. ) ;
#14051 = CARTESIAN_POINT ( 'NONE',  ( 14.38125909742180752, 10.73282306404720465, 10.73282306404724018 ) ) ;
#14052 = DIRECTION ( 'NONE',  ( 1.000000000000000000, 1.836970198721030181E-16, 0.000000000000000000 ) ) ;
#14053 = DIRECTION ( 'NONE',  ( 0.000000000000000000, 1.000000000000000000, 0.000000000000000000 ) ) ;
#14054 = CARTESIAN_POINT ( 'NONE',  ( 91.82158438592158234, -17.20528682183298486, 0.000000000000000000 ) ) ;
#14055 = EDGE_LOOP ( 'NONE', ( #20338, #6232, #20318, #1992 ) ) ;
#14056 = CARTESIAN_POINT ( 'NONE',  ( -194.7885354600801975, -44.44047100927770799, 18.40784581028790612 ) ) ;
#14057 = AXIS2_PLACEMENT_3D ( 'NONE', #21373, #3141, #6864 ) ;
#14058 = CIRCLE ( 'NONE', #22586, 74.99999999999995737 ) ;
#14059 = AXIS2_PLACEMENT_3D ( 'NONE', #9828, #17931, #1458 ) ;
#14060 = CARTESIAN_POINT ( 'NONE',  ( 199.9999999999998010, -18.94725682776174835, -1.557189005449375330 ) ) ;
#14061 = CARTESIAN_POINT ( 'NONE',  ( 6.202588568023359450, -14.15973318136377301, 49.19971320596261677 ) ) ;
#14062 = CARTESIAN_POINT ( 'NONE',  ( 23.32574057153200187, 23.35062444423039807, -42.87194976637071164 ) ) ;
#14063 = CARTESIAN_POINT ( 'NONE',  ( 199.0196534518890701, -18.22073438007316071, -8.257363271777977687 ) ) ;
#14064 = CARTESIAN_POINT ( 'NONE',  ( 149.5797498300190398, -29.41965740490887882, 12.18602109748309559 ) ) ;
#14065 = CARTESIAN_POINT ( 'NONE',  ( -185.5190930961058484, -17.55874694108397804, 42.39056500340862499 ) ) ;
#14066 = CARTESIAN_POINT ( 'NONE',  ( -238.4067589809705794, 28.96627169325354956, -28.96627169325289231 ) ) ;
#14067 = CARTESIAN_POINT ( 'NONE',  ( -87.02160487651677556, -5.405486468710360981, 20.76754707253114063 ) ) ;
#14068 = CIRCLE ( 'NONE', #14917, 9.999999999999969802 ) ;
#14070 = CARTESIAN_POINT ( 'NONE',  ( -56.48582580120559271, -6.472252184284276844, 6.472252184284108978 ) ) ;
#14069 = CARTESIAN_POINT ( 'NONE',  ( -192.1964066538111808, 24.16259023443393517, -43.96877160661179573 ) ) ;
#14071 = CARTESIAN_POINT ( 'NONE',  ( 184.8905102610680444, 20.92133201514447549, 0.000000000000000000 ) ) ;
#14072 = CARTESIAN_POINT ( 'NONE',  ( 19.06497207195980792, -14.19242893257839988, -40.00000000000002132 ) ) ;
#14073 = CIRCLE ( 'NONE', #25992, 30.00000000000000355 ) ;
#14074 = CARTESIAN_POINT ( 'NONE',  ( -105.3755690713226585, -21.75974354311652448, 40.00000000000002132 ) ) ;
#14075 = CARTESIAN_POINT ( 'NONE',  ( 151.7948205124836534, 40.00000000000012079, -6.767089262348609857 ) ) ;
#14076 = CARTESIAN_POINT ( 'NONE',  ( -162.0762913951020892, 29.48230308784758691, 29.48230308784772191 ) ) ;
#14077 = DIRECTION ( 'NONE',  ( 0.000000000000000000, -1.000000000000000000, 1.682156097916904081E-16 ) ) ;
#14078 = CARTESIAN_POINT ( 'NONE',  ( 151.7948205124835681, 51.78348778862544322, -4.785054706298002891 ) ) ;
#14079 = EDGE_LOOP ( 'NONE', ( #12292, #11826, #22343, #7688 ) ) ;
#14080 = CARTESIAN_POINT ( 'NONE',  ( 4.995406935893289102, 10.78321810388998081, 10.78321810389001811 ) ) ;
#14081 = CARTESIAN_POINT ( 'NONE',  ( -86.86493150571118349, -8.366608963954250910, 19.60045294882748124 ) ) ;
#14082 = ORIENTED_EDGE ( 'NONE', *, *, #7691, .F. ) ;
#14083 = ORIENTED_EDGE ( 'NONE', *, *, #13296, .T. ) ;
#14084 = CARTESIAN_POINT ( 'NONE',  ( 163.1118516004056573, -37.29075403953139300, -19.27778845539249630 ) ) ;
#14085 = CARTESIAN_POINT ( 'NONE',  ( 22.81400246987437441, -43.16348862150560706, -17.87890238636475360 ) ) ;
#14086 = ORIENTED_EDGE ( 'NONE', *, *, #25603, .T. ) ;
#14087 = CARTESIAN_POINT ( 'NONE',  ( 192.4448373802101173, 19.99999999996065014, -40.00000000000002132 ) ) ;
#14088 = FACE_OUTER_BOUND ( 'NONE', #25594, .T. ) ;
#14089 = ORIENTED_EDGE ( 'NONE', *, *, #21579, .F. ) ;
#14090 = CARTESIAN_POINT ( 'NONE',  ( 199.9999999999998010, 13.53697630789494255, 13.34066885590318030 ) ) ;
#14091 = CIRCLE ( 'NONE', #24309, 30.00000000000000355 ) ;
#14092 = CARTESIAN_POINT ( 'NONE',  ( -105.2333882009265693, 21.31109190976440715, -2.724924291338312266 ) ) ;
#14093 = EDGE_CURVE ( 'NONE', #9873, #7172, #14183, .T. ) ;
#14094 = CARTESIAN_POINT ( 'NONE',  ( -198.0356074513804572, 10.87444709759714989, 10.87444709759722450 ) ) ;
#14095 = CARTESIAN_POINT ( 'NONE',  ( -188.2871287166140917, -43.00155302796438406, -23.44689273421207076 ) ) ;
#14096 = CARTESIAN_POINT ( 'NONE',  ( -198.0356074513804572, -40.00000000000011369, 15.37879056873056527 ) ) ;
#14097 = CARTESIAN_POINT ( 'NONE',  ( 14.38125909742180752, 15.17850393972634038, 40.00000000000002132 ) ) ;
#14098 = CARTESIAN_POINT ( 'NONE',  ( -238.4067589809705794, 28.96627169325354956, -28.96627169325289231 ) ) ;
#14099 = CARTESIAN_POINT ( 'NONE',  ( 199.0222638060928375, 2.763249014911820733, 19.81200274180636711 ) ) ;
#14100 = CARTESIAN_POINT ( 'NONE',  ( 184.8905102610680444, 1.070102760522089011E-13, -20.92133201514444352 ) ) ;
#14101 = CARTESIAN_POINT ( 'NONE',  ( -105.3755690713226585, -40.00000000000010658, 18.24025645688337249 ) ) ;
#14102 = CARTESIAN_POINT ( 'NONE',  ( -86.96347745069644475, -2.438961472018186339E-13, 21.75974354311649961 ) ) ;
#14103 = CARTESIAN_POINT ( 'NONE',  ( 19.06497207195979726, 39.99999999999997158, 14.19242893257854554 ) ) ;
#14104 = CARTESIAN_POINT ( 'NONE',  ( -105.2333497862889686, -16.99530394072478856, 13.14348404883646815 ) ) ;
#14105 = CARTESIAN_POINT ( 'NONE',  ( 14.38125909742182529, -39.01709431150933938, 39.01709431150894147 ) ) ;
#14106 = CARTESIAN_POINT ( 'NONE',  ( -86.96347745069645896, 21.75974354311648895, -0.000000000000000000 ) ) ;
#14107 = EDGE_CURVE ( 'NONE', #20820, #17548, #3132, .T. ) ;
#14108 = CARTESIAN_POINT ( 'NONE',  ( -259.2033419157646676, -49.83842185052031937, -6.730120644403796426 ) ) ;
#14109 = DIRECTION ( 'NONE',  ( 0.000000000000000000, 0.000000000000000000, 1.000000000000000000 ) ) ;
#14110 = EDGE_CURVE ( 'NONE', #6927, #3040, #6885, .T. ) ;
#14111 = DIRECTION ( 'NONE',  ( -0.000000000000000000, -1.000000000000000000, -0.000000000000000000 ) ) ;
#14112 = CARTESIAN_POINT ( 'NONE',  ( 57.59792236341147031, -1.493297263419786540E-14, 2.435789363418160658 ) ) ;
#14113 = CARTESIAN_POINT ( 'NONE',  ( 170.2234770963711128, -40.00000000000004263, 15.44714144992801685 ) ) ;
#14114 = CARTESIAN_POINT ( 'NONE',  ( -192.9588430854690273, 66.79921049721887982, 10.23066800229522677 ) ) ;
#14115 = CIRCLE ( 'NONE', #2664, 5.000000000000004441 ) ;
#14116 = CARTESIAN_POINT ( 'NONE',  ( -114.4098922876147384, 20.15198150140922451, 8.347224046571190215 ) ) ;
#14117 = CARTESIAN_POINT ( 'NONE',  ( -188.9001659262688690, -17.93767091109449652, -43.30536839095078250 ) ) ;
#14118 = FACE_OUTER_BOUND ( 'NONE', #19913, .T. ) ;
#14119 = ORIENTED_EDGE ( 'NONE', *, *, #22424, .F. ) ;
#14120 = CARTESIAN_POINT ( 'NONE',  ( -213.1075012329537230, 9.698598906450543566, -9.698598906450348167 ) ) ;
#14121 = CARTESIAN_POINT ( 'NONE',  ( -259.2033419157646676, 9.517827891722584255, -0.000000000000000000 ) ) ;
#14122 =( NAMED_UNIT ( * ) SI_UNIT ( $, .STERADIAN. ) SOLID_ANGLE_UNIT ( ) );
#14123 = CARTESIAN_POINT ( 'NONE',  ( 0.2972598230770011618, 10.13633138497555919, -66.70487387989845729 ) ) ;
#14124 = CARTESIAN_POINT ( 'NONE',  ( -77.55640685880874230, 0.6928334182872019076, 22.13135000835299593 ) ) ;
#14125 = ORIENTED_EDGE ( 'NONE', *, *, #10379, .F. ) ;
#14126 = CARTESIAN_POINT ( 'NONE',  ( 199.9999999999999716, 17.43237942262683049, 7.572151140094372401 ) ) ;
#14127 = CARTESIAN_POINT ( 'NONE',  ( 21.15138808362599221, -23.80076113581848318, 43.47948264999429568 ) ) ;
#14128 = CARTESIAN_POINT ( 'NONE',  ( -4.339409867980440261, 17.83714383556808869, 43.06267456183103093 ) ) ;
#14129 = ORIENTED_EDGE ( 'NONE', *, *, #10544, .T. ) ;
#14130 = ORIENTED_EDGE ( 'NONE', *, *, #10058, .F. ) ;
#14131 = CARTESIAN_POINT ( 'NONE',  ( -192.9588430854689989, 10.23066800230742679, 10.23066800230749607 ) ) ;
#14132 = CARTESIAN_POINT ( 'NONE',  ( 199.0102239786929488, -4.226749394367478097, -19.54603893341629473 ) ) ;
#14133 = DIRECTION ( 'NONE',  ( 0.000000000000000000, 1.321694076934715579E-16, 1.000000000000000000 ) ) ;
#14134 = PRESENTATION_STYLE_ASSIGNMENT (( #26270 ) ) ;
#14135 = FACE_OUTER_BOUND ( 'NONE', #20053, .T. ) ;
#14136 = CARTESIAN_POINT ( 'NONE',  ( -105.3755690713226585, 39.99999999999977263, 21.75974354311691883 ) ) ;
#14137 = CARTESIAN_POINT ( 'NONE',  ( 98.29820294267415193, 2.605266741687827903, -19.87244099730190072 ) ) ;
#14138 = CARTESIAN_POINT ( 'NONE',  ( -82.28158677657542341, -19.22558455003817102, -6.254308823251737870 ) ) ;
#14139 = DIRECTION ( 'NONE',  ( 0.9698969544100564111, 0.09318942523058482141, 0.2249791742612868850 ) ) ;
#14140 = CARTESIAN_POINT ( 'NONE',  ( 199.0223319294094892, 2.599958516019920118, 19.83413122362564351 ) ) ;
#14141 = CARTESIAN_POINT ( 'NONE',  ( -678.9461782662789346, 75.00000000000000000, -29.99999999999836220 ) ) ;
#14142 = CARTESIAN_POINT ( 'NONE',  ( -4.037857402784335470, -23.44963359339763898, -43.00569567200361831 ) ) ;
#14143 = CARTESIAN_POINT ( 'NONE',  ( 184.8905102610680444, 14.79361573936424890, -41.77492675555986068 ) ) ;
#14144 = CARTESIAN_POINT ( 'NONE',  ( 200.0000000000000000, 60.00000000000007816, 7.960204194457792519E-15 ) ) ;
#14145 = CARTESIAN_POINT ( 'NONE',  ( -238.4067589809705794, -28.96627169325343942, 28.96627169325309126 ) ) ;
#14146 = CYLINDRICAL_SURFACE ( 'NONE', #25310, 69.99999999999998579 ) ;
#14147 = DIRECTION ( 'NONE',  ( 1.836970198721030181E-16, -1.000000000000000000, 0.000000000000000000 ) ) ;
#14148 = CARTESIAN_POINT ( 'NONE',  ( 192.4448373802101173, -19.99999999996057554, 40.00000000000002132 ) ) ;
#14149 = CARTESIAN_POINT ( 'NONE',  ( -317.0000000000000568, -4.857225732735059864E-14, -31.79780246617542616 ) ) ;
#14150 = CARTESIAN_POINT ( 'NONE',  ( -259.2033419157646676, -30.48217210827744239, -2.449293598294708485E-15 ) ) ;
#14151 = CARTESIAN_POINT ( 'NONE',  ( -110.1014694628346575, 14.86203413257348771, 13.68874972777938304 ) ) ;
#14152 = CARTESIAN_POINT ( 'NONE',  ( -100.7734535825088500, 40.00000000000017764, -17.32597176626768487 ) ) ;
#14153 = CARTESIAN_POINT ( 'NONE',  ( 146.6084372240433709, 3.800685668858776900, -52.76785682606518435 ) ) ;
#14154 = CARTESIAN_POINT ( 'NONE',  ( -208.1127848780265026, 15.00245453012665564, 0.000000000000000000 ) ) ;
#14155 = ORIENTED_EDGE ( 'NONE', *, *, #23310, .T. ) ;
#14156 = ORIENTED_EDGE ( 'NONE', *, *, #944, .F. ) ;
#14157 = CARTESIAN_POINT ( 'NONE',  ( -192.9588430854690273, 14.46834944099966336, 40.00000000000002132 ) ) ;
#14158 = CARTESIAN_POINT ( 'NONE',  ( 151.0853911467767432, 12.04115959307956452, 29.06993079631229548 ) ) ;
#14159 = CARTESIAN_POINT ( 'NONE',  ( -30.26275506840323359, -1.535832457777009877E-13, 41.69427246844629309 ) ) ;
#14160 = CARTESIAN_POINT ( 'NONE',  ( -86.96347745069644475, 12.89780903124349898, 43.67073346367994446 ) ) ;
#14161 = FACE_OUTER_BOUND ( 'NONE', #11096, .T. ) ;
#14162 = DIRECTION ( 'NONE',  ( 0.000000000000000000, 1.000000000000000000, 0.000000000000000000 ) ) ;
#14163 = CARTESIAN_POINT ( 'NONE',  ( 170.0000000000428315, 17.64300463311351308, -17.64300463311329992 ) ) ;
#14164 = CARTESIAN_POINT ( 'NONE',  ( 199.9999999999998579, 18.23094931701148269, -5.355502299499542040 ) ) ;
#14165 = CARTESIAN_POINT ( 'NONE',  ( 199.9999999999999432, -18.58351610408307764, -4.007049993893891049 ) ) ;
#14166 = CARTESIAN_POINT ( 'NONE',  ( 170.2234770963711128, 10.92277846919216522, -10.92277846919186501 ) ) ;
#14167 = CARTESIAN_POINT ( 'NONE',  ( 57.59792236341148453, -54.84617931850879557, 1.722363176414566155 ) ) ;
#14168 = DIRECTION ( 'NONE',  ( -1.000000000000000000, -1.836970198721030181E-16, -2.465190328815661892E-32 ) ) ;
#14169 = CARTESIAN_POINT ( 'NONE',  ( -77.59243545050232171, 13.54949188064891530, -17.47199274921711876 ) ) ;
#14170 = CARTESIAN_POINT ( 'NONE',  ( 192.4448373802100889, -14.14213562370293431, -14.14213562370322030 ) ) ;
#14171 = CARTESIAN_POINT ( 'NONE',  ( -30.26275506840324070, 1.198031551616030033, -1.198031551616006496 ) ) ;
#14172 = CARTESIAN_POINT ( 'NONE',  ( 136.1360204305621551, -53.05693388239309627, -3.511608612531332163 ) ) ;
#14173 = CARTESIAN_POINT ( 'NONE',  ( 91.82158438592156813, -16.11829626348402655, -40.45024623143966380 ) ) ;
#14174 = CARTESIAN_POINT ( 'NONE',  ( 199.0199791362716439, 7.640007438824279795, 18.48538610549022465 ) ) ;
#14176 = CARTESIAN_POINT ( 'NONE',  ( 19.06497207195981858, -1.881589693694111225E-13, 54.19242893257843008 ) ) ;
#14175 = CARTESIAN_POINT ( 'NONE',  ( -56.48582580120559271, 21.81201906317798489, -21.81201906317746619 ) ) ;
#14177 = CARTESIAN_POINT ( 'NONE',  ( -192.9588430854690273, 66.79921049724377724, -10.23066800231904239 ) ) ;
#14178 = CARTESIAN_POINT ( 'NONE',  ( 23.38399212876566935, 46.80460545930672822, -13.80022400692470974 ) ) ;
#14179 = CARTESIAN_POINT ( 'NONE',  ( 184.8905102610680444, 19.07866798485562398, -40.00000000000002132 ) ) ;
#14180 = VERTEX_POINT ( 'NONE', #4468 ) ;
#14181 = CARTESIAN_POINT ( 'NONE',  ( -105.3755690713226727, -15.38646221621786481, -15.38646221621789856 ) ) ;
#14182 = EDGE_CURVE ( 'NONE', #6305, #218, #22828, .T. ) ;
#14183 =( BOUNDED_CURVE ( )  B_SPLINE_CURVE ( 3, ( #13502, #3400, #7512, #15620 ),
 .UNSPECIFIED., .F., .F. ) 
 B_SPLINE_CURVE_WITH_KNOTS ( ( 4, 4 ),
 ( 0.01388163287021833454, 0.02359082919310023091 ),
 .UNSPECIFIED. ) 
 CURVE ( )  GEOMETRIC_REPRESENTATION_ITEM ( )  RATIONAL_B_SPLINE_CURVE ( ( 1.000000000000000000, 0.8672072324488980799, 0.7608653435686176802, 0.6809743333591588010 ) ) 
 REPRESENTATION_ITEM ( '' )  );
#14184 = CARTESIAN_POINT ( 'NONE',  ( -70.35386311763890888, -22.51194464688922636, 10.19784241824625681 ) ) ;
#14185 = CARTESIAN_POINT ( 'NONE',  ( -213.1075012329537230, 13.71589010951907817, 40.00000000000002132 ) ) ;
#14186 = EDGE_CURVE ( 'NONE', #10069, #12261, #924, .T. ) ;
#14187 = ORIENTED_EDGE ( 'NONE', *, *, #10625, .T. ) ;
#14188 = CARTESIAN_POINT ( 'NONE',  ( 22.68416413276406729, 23.49220544186221105, -43.06288726621002638 ) ) ;
#14189 = CARTESIAN_POINT ( 'NONE',  ( 200.0000000000005400, -16.47398309245309278, 9.506867245997410620 ) ) ;
#14190 = CARTESIAN_POINT ( 'NONE',  ( 6.371015797575695139, -18.55864253218550530, 44.80452650039092788 ) ) ;
#14191 = EDGE_CURVE ( 'NONE', #17701, #21989, #7481, .T. ) ;
#14192 = EDGE_CURVE ( 'NONE', #5353, #20921, #1152, .T. ) ;
#14193 = CARTESIAN_POINT ( 'NONE',  ( 23.32574057153225056, 13.80366151303488031, -46.82643129194528342 ) ) ;
#14194 = CARTESIAN_POINT ( 'NONE',  ( 199.0087111817176435, -0.6649071253763039202, -19.99597453042600392 ) ) ;
#14195 = CARTESIAN_POINT ( 'NONE',  ( 35.93702929055792339, -42.26928858464287231, 12.87541766862415571 ) ) ;
#14196 = FACE_BOUND ( 'NONE', #22876, .T. ) ;
#14197 = LINE ( 'NONE', #17917, #5050 ) ;
#14198 = CARTESIAN_POINT ( 'NONE',  ( 199.9999999999999432, 14.14213562373110911, -14.14213562373072364 ) ) ;
#14199 = CARTESIAN_POINT ( 'NONE',  ( -102.2610585947572872, -22.27377874548545833, 0.000000000000000000 ) ) ;
#14201 = CARTESIAN_POINT ( 'NONE',  ( 0.2972598230769938343, 10.13633138497486286, -10.13633138497461594 ) ) ;
#14200 = CARTESIAN_POINT ( 'NONE',  ( -188.3392995398497192, 23.45797413244903495, -43.01688924973676365 ) ) ;
#14202 = FACE_OUTER_BOUND ( 'NONE', #14394, .T. ) ;
#14203 = CARTESIAN_POINT ( 'NONE',  ( 91.82158438592159655, -22.79471317813468545, -2.449293598294708485E-15 ) ) ;
#14204 = CARTESIAN_POINT ( 'NONE',  ( -30.26275506840324425, 41.69427246844627177, 40.00000000000002132 ) ) ;
#14205 = CARTESIAN_POINT ( 'NONE',  ( -30.26275506840323359, -39.99999999999959499, -41.69427246844670520 ) ) ;
#14206 = CARTESIAN_POINT ( 'NONE',  ( -100.7734535825088500, 40.53558337403677569, -16.03295912088699993 ) ) ;
#14207 = CARTESIAN_POINT ( 'NONE',  ( 98.29820294268671432, 20.00000000000122213, -2.727061086135174062 ) ) ;
#14208 = CARTESIAN_POINT ( 'NONE',  ( -192.9588430854689989, -10.23066800230742501, -10.23066800230756712 ) ) ;
#14209 = VERTEX_POINT ( 'NONE', #13105 ) ;
#14210 = CARTESIAN_POINT ( 'NONE',  ( 57.59792236341147031, -1.722363176415032004, -1.722363176415048880 ) ) ;
#14211 = DIRECTION ( 'NONE',  ( 1.000000000000000000, -1.836970198721030181E-16, -0.000000000000000000 ) ) ;
#14212 = APPLICATION_PROTOCOL_DEFINITION ( 'draft international standard', 'automotive_design', 1998, #21585 ) ;
#14213 = ORIENTED_EDGE ( 'NONE', *, *, #7999, .F. ) ;
#14214 = ORIENTED_EDGE ( 'NONE', *, *, #18047, .F. ) ;
#14215 = CARTESIAN_POINT ( 'NONE',  ( -162.0762913951021176, -29.48230308784755493, -27.08623940707632372 ) ) ;
#14216 = CARTESIAN_POINT ( 'NONE',  ( 60.07376046255615876, -31.81923430144854237, -13.17995839187771701 ) ) ;
#14217 = ORIENTED_EDGE ( 'NONE', *, *, #970, .F. ) ;
#14218 = CARTESIAN_POINT ( 'NONE',  ( 146.6084372240433709, -34.62501878078303008, -40.00000000000002132 ) ) ;
#14219 = CARTESIAN_POINT ( 'NONE',  ( -99.31267923333899716, -20.62886818714040515, 8.544756979565530486 ) ) ;
#14220 = ORIENTED_EDGE ( 'NONE', *, *, #8637, .F. ) ;
#14221 = CARTESIAN_POINT ( 'NONE',  ( 199.9999999999997442, 15.07190321012488887, 11.58049570127731798 ) ) ;
#14222 = LINE ( 'NONE', #20485, #14517 ) ;
#14223 = CARTESIAN_POINT ( 'NONE',  ( 91.82158438592158234, 16.11829626348434630, -40.45024623143955012 ) ) ;
#14224 = CARTESIAN_POINT ( 'NONE',  ( -184.9730489279452570, -42.02334742175309401, -22.80026000643668382 ) ) ;
#14225 = CARTESIAN_POINT ( 'NONE',  ( -100.7734535825088500, -39.99999999999995737, -22.67402823373205578 ) ) ;
#14226 = CARTESIAN_POINT ( 'NONE',  ( 184.8905102610680444, -20.92133201514440799, 40.00000000000002132 ) ) ;
#14227 = CARTESIAN_POINT ( 'NONE',  ( 4.995406935893297984, 10.78321810390233892, -67.35176059882522281 ) ) ;
#14228 = CARTESIAN_POINT ( 'NONE',  ( 199.0263607205240532, -13.20175300279655062, 15.04466839055514527 ) ) ;
#14229 = CARTESIAN_POINT ( 'NONE',  ( 0.2972598230769957217, -4.999556039334937811E-14, 14.33493731733933352 ) ) ;
#14230 = CARTESIAN_POINT ( 'NONE',  ( 170.2234770963711128, -2.511315425431857630E-14, 15.44714144992816074 ) ) ;
#14231 = CARTESIAN_POINT ( 'NONE',  ( -91.56559293963836410, 40.00000000000008527, -22.67402823373177867 ) ) ;
#14232 = CARTESIAN_POINT ( 'NONE',  ( -91.56559293963836410, 22.67402823373190301, -40.00000000000002132 ) ) ;
#14233 = CARTESIAN_POINT ( 'NONE',  ( -162.0762913951020892, -29.48230308784785692, 29.48230308784751230 ) ) ;
#14234 = CARTESIAN_POINT ( 'NONE',  ( 136.1360204305621266, 35.03383547441298873, 0.000000000000000000 ) ) ;
#14235 = CARTESIAN_POINT ( 'NONE',  ( 146.6084372240433709, -32.08495691632041513, -24.48358557860343154 ) ) ;
#14236 = DIRECTION ( 'NONE',  ( 1.000000000000000000, 0.000000000000000000, 0.000000000000000000 ) ) ;
#14237 = CYLINDRICAL_SURFACE ( 'NONE', #12363, 29.99999999999999289 ) ;
#14238 = CARTESIAN_POINT ( 'NONE',  ( 130.8568914410475372, 24.07718906447210472, 24.07718906447249907 ) ) ;
#14239 = CARTESIAN_POINT ( 'NONE',  ( 184.8905102610680444, -3.509827109981123710E-14, 19.07866798485558490 ) ) ;
#14240 = CARTESIAN_POINT ( 'NONE',  ( 14.38125909742181108, 39.01709431150907648, 39.01709431150921858 ) ) ;
#14241 = CARTESIAN_POINT ( 'NONE',  ( 163.1118516004056573, -9.006482792074626431, 47.56205970284951690 ) ) ;
#14242 = CARTESIAN_POINT ( 'NONE',  ( -188.3611024622183265, -13.83140737835580580, -47.01268868734971562 ) ) ;
#14243 = CARTESIAN_POINT ( 'NONE',  ( -105.3755690713226727, 15.38646221621793231, -15.38646221621779020 ) ) ;
#14244 = ORIENTED_EDGE ( 'NONE', *, *, #24271, .F. ) ;
#14245 = CARTESIAN_POINT ( 'NONE',  ( -135.8532207217289738, -34.75652343174584757, -21.81201906317816253 ) ) ;
#14246 = LINE ( 'NONE', #7494, #15272 ) ;
#14247 = CARTESIAN_POINT ( 'NONE',  ( -162.0762913951020892, -1.694272876828353702, 0.000000000000000000 ) ) ;
#14248 = CARTESIAN_POINT ( 'NONE',  ( 150.0000000000000284, -3.909639452396722983E-15, -7.395570986446985676E-31 ) ) ;
#14249 = CARTESIAN_POINT ( 'NONE',  ( -238.4067589809705794, 0.6820004458491113475, -57.25054294077229144 ) ) ;
#14250 =( NAMED_UNIT ( * ) PLANE_ANGLE_UNIT ( ) SI_UNIT ( $, .RADIAN. ) );
#14251 = CARTESIAN_POINT ( 'NONE',  ( -83.21262154144250189, 13.72187187061492075, 33.12752917118417173 ) ) ;
#14252 = COLOUR_RGB ( '',0.7921568627450980005, 0.8196078431372548767, 0.9333333333333333481 ) ;
#14253 = VERTEX_POINT ( 'NONE', #3506 ) ;
#14254 = VECTOR ( 'NONE', #12634, 1000.000000000000114 ) ;
#14255 = CARTESIAN_POINT ( 'NONE',  ( 199.9999999999999432, 15.44072620018067887, 11.08370022558889545 ) ) ;
#14256 = CARTESIAN_POINT ( 'NONE',  ( 17.76569343199600226, -24.33587863439579024, 44.20364726159875346 ) ) ;
#14257 = CARTESIAN_POINT ( 'NONE',  ( -1.087763065865680279, 13.97201973057867619, 47.95583523901584755 ) ) ;
#14258 = VERTEX_POINT ( 'NONE', #5374 ) ;
#14259 = ORIENTED_EDGE ( 'NONE', *, *, #17492, .T. ) ;
#14260 = CARTESIAN_POINT ( 'NONE',  ( 130.8568914410475372, -34.05028731879786363, 0.000000000000000000 ) ) ;
#14261 = CARTESIAN_POINT ( 'NONE',  ( 199.0070327355206246, 4.219744681889460836, -19.54794762927634366 ) ) ;
#14262 = CARTESIAN_POINT ( 'NONE',  ( -716.9846540392142060, -66.50000000000001421, 61.50000000000005684 ) ) ;
#14263 = AXIS2_PLACEMENT_3D ( 'NONE', #5099, #17319, #25452 ) ;
#14264 = ADVANCED_FACE ( 'NONE', ( #19599, #17591 ), #17345, .F. ) ;
#14265 = CARTESIAN_POINT ( 'NONE',  ( -97.73806390046838999, -8.581719943991895860, -20.71810467719076598 ) ) ;
#14266 = CARTESIAN_POINT ( 'NONE',  ( -56.48582580120559982, 40.00000000000034106, -30.84685318188602210 ) ) ;
#14267 = CARTESIAN_POINT ( 'NONE',  ( 98.29820294267348402, 5.160908283043466938, -19.33391160836868750 ) ) ;
#14268 = CARTESIAN_POINT ( 'NONE',  ( -629.0547673868355787, 26.53338973019900138, 29.93293935381844406 ) ) ;
#14269 = VECTOR ( 'NONE', #21023, 1000.000000000000000 ) ;
#14270 = CARTESIAN_POINT ( 'NONE',  ( -317.0000000000000568, -4.504554366608264653E-14, -28.79780246617542616 ) ) ;
#14271 = CARTESIAN_POINT ( 'NONE',  ( 199.0156213727907186, 14.58859942632390094, 13.68185500382998576 ) ) ;
#14272 = CARTESIAN_POINT ( 'NONE',  ( -726.9846540392142060, 66.50000000000009948, -66.50000000000005684 ) ) ;
#14273 = CARTESIAN_POINT ( 'NONE',  ( -3.856733984653721414, -17.89110409353214948, -43.19294614843406777 ) ) ;
#14274 = CARTESIAN_POINT ( 'NONE',  ( -192.9588430854690273, -66.79921049721887982, -10.23066800229569040 ) ) ;
#14275 = CARTESIAN_POINT ( 'NONE',  ( -114.7539999570855400, -13.57343626010274740, -17.50303175002473566 ) ) ;
#14276 = CARTESIAN_POINT ( 'NONE',  ( 151.7948205124836534, -33.06932595376343897, -23.49921654116042902 ) ) ;
#14277 = CARTESIAN_POINT ( 'NONE',  ( 190.0000000000000000, -35.78896085774750446, 65.91016826501511616 ) ) ;
#14278 = CARTESIAN_POINT ( 'NONE',  ( 163.1118516004056573, 27.26290988616875310, 0.000000000000000000 ) ) ;
#14279 = CARTESIAN_POINT ( 'NONE',  ( -213.1075012329537230, -13.71589010951915810, 40.00000000000002132 ) ) ;
#14280 = CARTESIAN_POINT ( 'NONE',  ( -200.0000000000000000, 75.00000000000000000, 0.000000000000000000 ) ) ;
#14281 = CARTESIAN_POINT ( 'NONE',  ( -105.3755690713226585, -18.24025645688355013, 40.00000000000002132 ) ) ;
#14282 = CARTESIAN_POINT ( 'NONE',  ( -114.7122376710347424, 18.03507107370589679, 12.72361799391042858 ) ) ;
#14283 = CARTESIAN_POINT ( 'NONE',  ( -162.0762913951020892, 4.094006889353306706E-13, -41.69427287682835015 ) ) ;
#14284 = CARTESIAN_POINT ( 'NONE',  ( 184.8905102610680444, 13.49065550809817715, -43.07788698682574591 ) ) ;
#14285 = ADVANCED_FACE ( 'NONE', ( #9487 ), #7482, .T. ) ;
#14286 = CARTESIAN_POINT ( 'NONE',  ( 163.1118516004056573, -27.26290988616869626, 0.000000000000000000 ) ) ;
#14287 = ORIENTED_EDGE ( 'NONE', *, *, #1740, .F. ) ;
#14288 = EDGE_LOOP ( 'NONE', ( #20954, #20210, #8840, #3754 ) ) ;
#14289 = ORIENTED_EDGE ( 'NONE', *, *, #14753, .T. ) ;
#14290 = CARTESIAN_POINT ( 'NONE',  ( -135.8532207217289738, -9.153146818113595984, 0.000000000000000000 ) ) ;
#14291 = CARTESIAN_POINT ( 'NONE',  ( 169.9999999999999716, -22.62041470344880523, -9.369682556672316309 ) ) ;
#14292 =( BOUNDED_CURVE ( )  B_SPLINE_CURVE ( 3, ( #37, #12532, #20403, #24931 ),
 .UNSPECIFIED., .F., .F. ) 
 B_SPLINE_CURVE_WITH_KNOTS ( ( 4, 4 ),
 ( 0.01388163287021780372, 0.02359082919310006438 ),
 .UNSPECIFIED. ) 
 CURVE ( )  GEOMETRIC_REPRESENTATION_ITEM ( )  RATIONAL_B_SPLINE_CURVE ( ( 1.000000000000000000, 0.8672072324488987460, 0.7608653435686186794, 0.6809743333591599113 ) ) 
 REPRESENTATION_ITEM ( '' )  );
#14293 = CARTESIAN_POINT ( 'NONE',  ( 170.2234770963711128, 40.00000000000000000, 15.44714144992830462 ) ) ;
#14294 = CARTESIAN_POINT ( 'NONE',  ( -100.7734535825088500, 40.53558337403654832, 16.03295912088756481 ) ) ;
#14295 = CARTESIAN_POINT ( 'NONE',  ( 192.4448373802100889, -1.741373372144848397E-13, 20.00000000003942091 ) ) ;
#14296 = VECTOR ( 'NONE', #4631, 1000.000000000000000 ) ;
#14297 = CYLINDRICAL_SURFACE ( 'NONE', #12556, 30.00000000000000000 ) ;
#14298 = CARTESIAN_POINT ( 'NONE',  ( 190.0000000000000000, -61.50000000000001421, 66.50000000000005684 ) ) ;
#14299 = CARTESIAN_POINT ( 'NONE',  ( 199.9999999999998010, 13.53697630789494255, 13.34066885590318030 ) ) ;
#14300 = CARTESIAN_POINT ( 'NONE',  ( 199.9999999999998863, -9.911147489498389973, -16.22017844385999297 ) ) ;
#14301 = CARTESIAN_POINT ( 'NONE',  ( -135.8532207217289738, 50.09629031063956006, 6.472252184284782217 ) ) ;
#14302 = CARTESIAN_POINT ( 'NONE',  ( 146.6084372240433709, -32.08495691632075619, 24.48358557860298035 ) ) ;
#14303 = CARTESIAN_POINT ( 'NONE',  ( -348.0000000000001137, -4.857225732735059864E-14, 0.000000000000000000 ) ) ;
#14304 = CARTESIAN_POINT ( 'NONE',  ( -280.0000000000000568, 39.99999999999976552, 20.00000000000043343 ) ) ;
#14305 = CARTESIAN_POINT ( 'NONE',  ( 151.7948205124836534, -33.06932595376376582, 23.49921654115996006 ) ) ;
#14306 = CARTESIAN_POINT ( 'NONE',  ( -87.12803293485033862, 14.20621343982535834, -16.13817828096302165 ) ) ;
#14307 = CARTESIAN_POINT ( 'NONE',  ( 184.8905102610680444, -14.79361573936399665, 14.79361573936367158 ) ) ;
#14308 = CARTESIAN_POINT ( 'NONE',  ( 0.2972598230769976091, -10.13633138497479180, 10.13633138497468522 ) ) ;
#14309 = CARTESIAN_POINT ( 'NONE',  ( 199.0176277365346778, 11.71792290964084060, 16.22639131207622754 ) ) ;
#14311 = CARTESIAN_POINT ( 'NONE',  ( -56.48582580120558561, -1.205267837095813407E-13, 30.84685318188644132 ) ) ;
#14310 = CARTESIAN_POINT ( 'NONE',  ( -30.26275506840325136, 57.76657404653985139, -1.198031551615314161 ) ) ;
#14312 = CARTESIAN_POINT ( 'NONE',  ( -135.8532207217289738, 21.81201906317729566, 34.75652343174635917 ) ) ;
#14313 = CARTESIAN_POINT ( 'NONE',  ( 22.13784119383518600, 43.34234508276902176, -17.95298715833884629 ) ) ;
#14314 = CARTESIAN_POINT ( 'NONE',  ( 91.82158438592158234, 22.79471317813472098, 2.449293598294708485E-15 ) ) ;
#14315 = ORIENTED_EDGE ( 'NONE', *, *, #15160, .F. ) ;
#14316 = CARTESIAN_POINT ( 'NONE',  ( -2.937533998801357349, -23.68967259551906324, -43.32931883107454496 ) ) ;
#14317 = AXIS2_PLACEMENT_3D ( 'NONE', #2925, #23523, #13529 ) ;
#14318 = CARTESIAN_POINT ( 'NONE',  ( -24.88648382771808798, -39.69105101982836459, 12.31763033300906152 ) ) ;
#14319 = CARTESIAN_POINT ( 'NONE',  ( -135.8532207217289738, 30.84685318188643066, 2.449293598294708485E-15 ) ) ;
#14320 = VERTEX_POINT ( 'NONE', #25353 ) ;
#14321 = DIRECTION ( 'NONE',  ( 0.000000000000000000, 1.000000000000000000, 0.000000000000000000 ) ) ;
#14322 = VECTOR ( 'NONE', #253, 1000.000000000000000 ) ;
#14323 = DIRECTION ( 'NONE',  ( 0.000000000000000000, 1.000000000000000000, 0.000000000000000000 ) ) ;
#14324 = CARTESIAN_POINT ( 'NONE',  ( 2.332272417610701698, -14.08759251168401860, 48.72342300853175345 ) ) ;
#14325 = B_SPLINE_CURVE_WITH_KNOTS ( 'NONE', 3,
 ( #21341, #23464, #23708, #11590, #3112, #11217, #1244, #25854, #13587, #9225, #17334, #25468, #11341, #7219, #15335, #13340 ),
 .UNSPECIFIED., .F., .F.,
 ( 4, 2, 2, 2, 2, 2, 2, 4 ),
 ( -5.998499567629515208E-08, 0.003520343011582079042, 0.007040746008159834424, 0.01408155200131533044, 0.01760195499789308018, 0.02112235799447082646, 0.02464276099104857620, 0.02816316398762632248 ),
 .UNSPECIFIED. ) ;
#14326 = CARTESIAN_POINT ( 'NONE',  ( 2.692156443674271760, 18.42752958144669506, -44.48799183654966782 ) ) ;
#14327 = CARTESIAN_POINT ( 'NONE',  ( 199.0168191192024949, -15.25344411108907572, -12.94054329384263724 ) ) ;
#14328 = CARTESIAN_POINT ( 'NONE',  ( -86.96347745069644475, -2.438961472018186339E-13, 21.75974354311649961 ) ) ;
#14329 = DIRECTION ( 'NONE',  ( 0.000000000000000000, 0.000000000000000000, 1.000000000000000000 ) ) ;
#14330 = CARTESIAN_POINT ( 'NONE',  ( -166.3490736463351993, -12.23457872950100267, 39.29841219613869896 ) ) ;
#14331 = ADVANCED_FACE ( 'NONE', ( #17724 ), #23595, .F. ) ;
#14332 = CARTESIAN_POINT ( 'NONE',  ( -91.56559293963834989, 12.25131212657497848, -12.25131212657469426 ) ) ;
#14333 = CARTESIAN_POINT ( 'NONE',  ( -105.3895334812061293, 9.637394427376211326, -19.08270859416220944 ) ) ;
#14335 = CARTESIAN_POINT ( 'NONE',  ( 4.995406935893283773, 39.06748935135171052, 17.50105314357239195 ) ) ;
#14334 = CARTESIAN_POINT ( 'NONE',  ( -189.6939645179747629, 18.01965094556769387, -43.50328570201348555 ) ) ;
#14336 = CARTESIAN_POINT ( 'NONE',  ( 199.9999999999999432, -14.14213562373115884, 14.14213562373085153 ) ) ;
#14337 = CARTESIAN_POINT ( 'NONE',  ( 19.06497207195982924, -54.19242893257843008, -40.00000000000002132 ) ) ;
#14338 = CARTESIAN_POINT ( 'NONE',  ( -56.48582580120559271, 30.84685318188643066, 2.449293598294708485E-15 ) ) ;
#14339 = EDGE_CURVE ( 'NONE', #19588, #21418, #25374, .T. ) ;
#14340 = CARTESIAN_POINT ( 'NONE',  ( 146.6084372240433709, -40.00000000000036238, 34.62501878078263218 ) ) ;
#14341 = CARTESIAN_POINT ( 'NONE',  ( -91.56559293963834989, 12.25131212657480440, 12.25131212657486834 ) ) ;
#14342 =( BOUNDED_SURFACE ( )  B_SPLINE_SURFACE ( 3, 2, ( 
 ( #1598, #11686, #19676 ),
 ( #9565, #20216, #15937 ),
 ( #17940, #22085, #11824 ),
 ( #8096, #15676, #17675 ),
 ( #18202, #14219, #25817 ),
 ( #13689, #26086, #22355 ),
 ( #21484, #19942, #16216 ),
 ( #7821, #7563, #21810 ),
 ( #7961, #5980, #4133 ),
 ( #24070, #17806, #3858 ),
 ( #7694, #16079, #3995 ),
 ( #15806, #23931, #24207 ) ),
 .UNSPECIFIED., .F., .F., .F. ) 
 B_SPLINE_SURFACE_WITH_KNOTS ( ( 4, 2, 2, 2, 2, 4 ),
 ( 3, 3 ),
 ( 0.006022589392323847955, 0.01254516766564278685, 0.01580645680230225586, 0.01906774593896172487, 0.02559032421228066290, 0.03211290248559960092 ),
 ( 0.000000000000000000, 1.000000000000000000 ),
 .UNSPECIFIED. ) 
 GEOMETRIC_REPRESENTATION_ITEM ( )  RATIONAL_B_SPLINE_SURFACE ( (
 ( 1.000000000000000000, 0.9998834880171260098, 1.000000000000000000),
 ( 1.000000000000000000, 0.9998139205012248620, 1.000000000000000000),
 ( 1.000000000000000000, 0.9997315632444678801, 1.000000000000000000),
 ( 1.000000000000000000, 0.9996405464946959141, 1.000000000000000000),
 ( 1.000000000000000000, 0.9996155081777534646, 1.000000000000000000),
 ( 1.000000000000000000, 0.9995814087510496160, 1.000000000000000000),
 ( 1.000000000000000000, 0.9995724100939920032, 1.000000000000000000),
 ( 1.000000000000000000, 0.9995726760936896049, 1.000000000000000000),
 ( 1.000000000000000000, 0.9996103361817947341, 1.000000000000000000),
 ( 1.000000000000000000, 0.9997312749795597142, 1.000000000000000000),
 ( 1.000000000000000000, 0.9998135910915183500, 1.000000000000000000),
 ( 1.000000000000000000, 0.9998834880173385065, 1.000000000000000000) ) ) 
 REPRESENTATION_ITEM ( '' )  SURFACE ( )  );
#14343 = CARTESIAN_POINT ( 'NONE',  ( 98.29820294267403824, -2.605266741685067888, 19.87244099730234481 ) ) ;
#14344 = CARTESIAN_POINT ( 'NONE',  ( -91.56559293963834989, -12.25131212657475466, -12.25131212657495361 ) ) ;
#14345 = ADVANCED_FACE ( 'NONE', ( #15594 ), #25610, .F. ) ;
#14346 = ADVANCED_FACE ( 'NONE', ( #23719 ), #5500, .T. ) ;
#14347 = ORIENTED_EDGE ( 'NONE', *, *, #7424, .T. ) ;
#14348 = CARTESIAN_POINT ( 'NONE',  ( -259.2033419157646676, -35.01439189186554302, 21.55415060305832498 ) ) ;
#14349 = CARTESIAN_POINT ( 'NONE',  ( -89.91646883265939039, 8.407637968706790588, 20.29783361022716193 ) ) ;
#14350 = ORIENTED_EDGE ( 'NONE', *, *, #16780, .T. ) ;
#14351 = CARTESIAN_POINT ( 'NONE',  ( -86.96347745069643054, -41.18208027870589660, -15.38646221621809040 ) ) ;
#14352 = CARTESIAN_POINT ( 'NONE',  ( 8.556015491681991492, -49.31947911770831894, -14.17785852676117209 ) ) ;
#14353 = ORIENTED_EDGE ( 'NONE', *, *, #2792, .T. ) ;
#14354 = CARTESIAN_POINT ( 'NONE',  ( 199.9999999999999432, -20.00000000000006750, 0.000000000000000000 ) ) ;
#14355 = CARTESIAN_POINT ( 'NONE',  ( -82.30220482034326324, -7.992411108785252516, -18.51665893431348309 ) ) ;
#14356 = ORIENTED_EDGE ( 'NONE', *, *, #16711, .T. ) ;
#14357 = CARTESIAN_POINT ( 'NONE',  ( 200.0000000000003695, 4.006257452897062699, 18.58368358710308144 ) ) ;
#14358 = CARTESIAN_POINT ( 'NONE',  ( -190.0000000000000284, -82.49999999999990052, 52.49999999999977973 ) ) ;
#14359 = CARTESIAN_POINT ( 'NONE',  ( 200.0000000000000000, 14.14213562373100608, -42.42640687119291698 ) ) ;
#14360 = CARTESIAN_POINT ( 'NONE',  ( -188.6013942375920749, -43.09289976588301840, -23.51434495930372393 ) ) ;
#14361 = CARTESIAN_POINT ( 'NONE',  ( 192.4448373802101173, -39.99999999999991473, -20.00000000003956302 ) ) ;
#14362 = CARTESIAN_POINT ( 'NONE',  ( -86.96347745069644475, -21.75974354311651737, 0.000000000000000000 ) ) ;
#14363 = CARTESIAN_POINT ( 'NONE',  ( 14.38125909742181285, -17.55144818341421598, -39.01709431150935359 ) ) ;
#14364 = CARTESIAN_POINT ( 'NONE',  ( 199.0263115711520072, -12.44642065545630238, 15.66510279686564289 ) ) ;
#14365 = CARTESIAN_POINT ( 'NONE',  ( 192.4448373802101173, -39.99999999999991473, -20.00000000003956302 ) ) ;
#14366 = CARTESIAN_POINT ( 'NONE',  ( 192.4448373802101173, -39.99999999999991473, -20.00000000003956302 ) ) ;
#14367 = CARTESIAN_POINT ( 'NONE',  ( 151.7948205124836534, 40.00000000000002842, 6.767089262349174739 ) ) ;
#14368 = CARTESIAN_POINT ( 'NONE',  ( 163.1118516004056573, 27.26290988616875310, 0.000000000000000000 ) ) ;
#14369 = CARTESIAN_POINT ( 'NONE',  ( 57.59792236341148453, -26.56190807104700369, 26.56190807104673723 ) ) ;
#14370 = CARTESIAN_POINT ( 'NONE',  ( -162.0762913951020607, -41.69427287682838568, -2.449293598294708485E-15 ) ) ;
#14371 = CARTESIAN_POINT ( 'NONE',  ( 192.4448373802101173, 14.14213562375862665, 42.42640687116509213 ) ) ;
#14372 = CARTESIAN_POINT ( 'NONE',  ( -163.5815475687390403, 12.03526863292960236, 38.33196416462965317 ) ) ;
#14373 = CARTESIAN_POINT ( 'NONE',  ( -188.2995950289364657, -23.44932284466040784, 43.00522595870950937 ) ) ;
#14374 = CARTESIAN_POINT ( 'NONE',  ( -91.56559293963836410, 40.00000000000019185, -17.32597176626768487 ) ) ;
#14375 = CARTESIAN_POINT ( 'NONE',  ( 200.0000000000000000, -40.00000000000005684, 19.99999999999978328 ) ) ;
#14376 = CARTESIAN_POINT ( 'NONE',  ( 19.06497207195981147, 38.31983398719620482, 38.31983398719633271 ) ) ;
#14377 = CARTESIAN_POINT ( 'NONE',  ( 150.0000000000000284, -125.7889608577475116, 82.50000000000001421 ) ) ;
#14378 = PLANE ( 'NONE',  #19943 ) ;
#14379 = CARTESIAN_POINT ( 'NONE',  ( -208.1127848780264742, -67.17687982763172272, 10.60833733270744617 ) ) ;
#14380 = EDGE_CURVE ( 'NONE', #2026, #5206, #20693, .T. ) ;
#14381 = ORIENTED_EDGE ( 'NONE', *, *, #16617, .T. ) ;
#14382 = CARTESIAN_POINT ( 'NONE',  ( -105.3755690713226727, -15.38646221621807619, 15.38646221621768362 ) ) ;
#14383 = CARTESIAN_POINT ( 'NONE',  ( -83.87175289014592749, 19.20738476421698238, 7.955959267057188811 ) ) ;
#14384 = CARTESIAN_POINT ( 'NONE',  ( 170.2234770963711128, -15.44714144992812699, -40.00000000000002132 ) ) ;
#14385 = DIRECTION ( 'NONE',  ( 0.9352143328345648987, -0.3271292286618222023, -0.1355013631515235850 ) ) ;
#14386 = CARTESIAN_POINT ( 'NONE',  ( 91.82158438592158234, -12.16597498397778843, 12.16597498397750954 ) ) ;
#14387 =( NAMED_UNIT ( * ) PLANE_ANGLE_UNIT ( ) SI_UNIT ( $, .RADIAN. ) );
#14388 = ORIENTED_EDGE ( 'NONE', *, *, #3799, .T. ) ;
#14389 = EDGE_LOOP ( 'NONE', ( #23301, #7306 ) ) ;
#14390 = CARTESIAN_POINT ( 'NONE',  ( 199.9999999999999716, 7.398602371178625958, 17.50881939353996231 ) ) ;
#14391 = CARTESIAN_POINT ( 'NONE',  ( -77.90255099906769942, -8.644468104261466834, -20.04994828523962980 ) ) ;
#14392 = CARTESIAN_POINT ( 'NONE',  ( 23.26364522860060191, 13.80713620122610941, 46.84987168987027673 ) ) ;
#14393 = ORIENTED_EDGE ( 'NONE', *, *, #2327, .T. ) ;
#14394 = EDGE_LOOP ( 'NONE', ( #10141, #6405, #12095, #5389 ) ) ;
#14395 = CARTESIAN_POINT ( 'NONE',  ( -162.0762913951020892, 1.198031840385716418, 1.198031840385750169 ) ) ;
#14396 = CARTESIAN_POINT ( 'NONE',  ( 199.0130599948309680, -9.716555752287060699, -17.48250520384952367 ) ) ;
#14397 = CARTESIAN_POINT ( 'NONE',  ( -198.0012401002533977, -44.79720214428356684, 24.77357857137259955 ) ) ;
#14398 =( NAMED_UNIT ( * ) SI_UNIT ( $, .STERADIAN. ) SOLID_ANGLE_UNIT ( ) );
#14399 = B_SPLINE_CURVE_WITH_KNOTS ( 'NONE', 3,
 ( #15267, #21398, #11274, #1179, #19646, #1430, #17006, #9281 ),
 .UNSPECIFIED., .F., .F.,
 ( 4, 2, 2, 4 ),
 ( 0.0002278873370217108000, 0.004309043385688178691, 0.006349621410021411526, 0.008390199434354645228 ),
 .UNSPECIFIED. ) ;
#14400 = CIRCLE ( 'NONE', #19917, 5.000000000000004441 ) ;
#14401 = CARTESIAN_POINT ( 'NONE',  ( -99.31364972223276766, -8.164808577092738773, -20.79869444142337187 ) ) ;
#14402 = CARTESIAN_POINT ( 'NONE',  ( -56.48582580120558561, 3.151766524733697544E-13, -30.84685318188644132 ) ) ;
#14403 = CARTESIAN_POINT ( 'NONE',  ( -198.0356074513804572, 1.247057299367198800E-13, -15.37879056873070560 ) ) ;
#14404 = CARTESIAN_POINT ( 'NONE',  ( -175.9234132798436292, 42.70618380303040595, -12.95567000669884905 ) ) ;
#14405 = CARTESIAN_POINT ( 'NONE',  ( -16.41582555442421665, -21.03675245956757323, 39.35881747731896496 ) ) ;
#14406 = CARTESIAN_POINT ( 'NONE',  ( 199.0221265002223845, 3.088699012602908578, 19.76381171561452632 ) ) ;
#14407 = CARTESIAN_POINT ( 'NONE',  ( -184.9729924863079020, 13.59277144552584815, 45.83719276897330985 ) ) ;
#14408 = CARTESIAN_POINT ( 'NONE',  ( 23.42154907652914630, -23.32998349128497750, -42.84253412640330794 ) ) ;
#14409 = CARTESIAN_POINT ( 'NONE',  ( -238.4067589809705794, -57.25054294077233408, -0.6820004458489551391 ) ) ;
#14410 = CARTESIAN_POINT ( 'NONE',  ( -86.86493150571116928, 19.60045294882758071, -8.366608963953975575 ) ) ;
#14411 = CARTESIAN_POINT ( 'NONE',  ( -91.56559293963836410, 44.31723036834890905, 12.25131212657507795 ) ) ;
#14412 = CARTESIAN_POINT ( 'NONE',  ( -77.55640685876512919, -9.396736996787174904E-14, 22.13135000837103661 ) ) ;
#14413 = CARTESIAN_POINT ( 'NONE',  ( 170.2234770963711128, 17.36149277826980253, 17.36149277827007253 ) ) ;
#14414 = CARTESIAN_POINT ( 'NONE',  ( 0.2972598230769983307, -14.33493731733933352, 40.00000000000002132 ) ) ;
#14415 = DIRECTION ( 'NONE',  ( -1.000000000000000000, 0.000000000000000000, 0.000000000000000000 ) ) ;
#14416 = CARTESIAN_POINT ( 'NONE',  ( -56.48582580120558561, -30.84685318188645908, 40.00000000000002132 ) ) ;
#14417 = CARTESIAN_POINT ( 'NONE',  ( -105.4282329516590977, 9.018643079774772531, 19.35470593465534250 ) ) ;
#14418 = CARTESIAN_POINT ( 'NONE',  ( 151.7948205124836534, 40.00000000000012079, -6.767089262348609857 ) ) ;
#14419 = CARTESIAN_POINT ( 'NONE',  ( 4.995406935893283773, 39.06748935135195211, -17.50105314357185193 ) ) ;
#14420 = CARTESIAN_POINT ( 'NONE',  ( 0.2972598230769930017, 14.33493731733933352, -40.00000000000002132 ) ) ;
#14421 = EDGE_LOOP ( 'NONE', ( #19810, #112, #22551, #12796 ) ) ;
#14422 = ORIENTED_EDGE ( 'NONE', *, *, #16234, .T. ) ;
#14423 = CARTESIAN_POINT ( 'NONE',  ( 136.1360204305621266, -35.03383547441293899, 0.000000000000000000 ) ) ;
#14424 =( NAMED_UNIT ( * ) SI_UNIT ( $, .STERADIAN. ) SOLID_ANGLE_UNIT ( ) );
#14425 = AXIS2_PLACEMENT_3D ( 'NONE', #17479, #15479, #19611 ) ;
#14426 = CARTESIAN_POINT ( 'NONE',  ( -86.96347745069644475, 41.18208027870576871, 15.38646221621837107 ) ) ;
#14427 = CARTESIAN_POINT ( 'NONE',  ( -105.2502192157103877, -21.20168261174586988, 3.402547493086664154 ) ) ;
#14428 = ADVANCED_FACE ( 'NONE', ( #13601 ), #21494, .T. ) ;
#14429 = CARTESIAN_POINT ( 'NONE',  ( 146.6084372240433993, -34.62501878078303008, 0.000000000000000000 ) ) ;
#14430 = CARTESIAN_POINT ( 'NONE',  ( -726.9846540392142060, 82.50000000000008527, 52.49999999999980105 ) ) ;
#14431 = CARTESIAN_POINT ( 'NONE',  ( 199.9999999999997442, 17.78964944107278967, -6.681507572083275726 ) ) ;
#14432 = ADVANCED_FACE ( 'NONE', ( #7353 ), #15466, .T. ) ;
#14433 = CARTESIAN_POINT ( 'NONE',  ( 199.9999999999999716, 2.628281398024471027, -18.82296940602922675 ) ) ;
#14434 = CARTESIAN_POINT ( 'NONE',  ( 192.4448373802101173, 14.14213562370261279, 42.42640687122091236 ) ) ;
#14435 = CARTESIAN_POINT ( 'NONE',  ( 146.6084372240433993, -3.800685668858596156, -3.800685668858692967 ) ) ;
#14436 = CARTESIAN_POINT ( 'NONE',  ( -105.2334388082176844, 21.30961024024002626, 2.995222947295622440 ) ) ;
#14437 = CARTESIAN_POINT ( 'NONE',  ( -162.0762913951021176, 40.00000000000042633, -41.69427287672947102 ) ) ;
#14438 = CARTESIAN_POINT ( 'NONE',  ( 91.82158438592159655, -16.11829626346125011, -16.11829626346154853 ) ) ;
#14439 = DIRECTION ( 'NONE',  ( -1.000000000000000000, -0.000000000000000000, -0.000000000000000000 ) ) ;
#14440 = CARTESIAN_POINT ( 'NONE',  ( -213.1075012329537230, 9.698598906450410340, 9.698598906450483170 ) ) ;
#14441 = EDGE_CURVE ( 'NONE', #15233, #5232, #18130, .T. ) ;
#14442 = CARTESIAN_POINT ( 'NONE',  ( 14.38125909742181818, -39.01709431150904095, -17.55144818341490165 ) ) ;
#14443 = CARTESIAN_POINT ( 'NONE',  ( 199.0199344320482453, 7.725485862940699278, 18.44984083464702351 ) ) ;
#14444 = CIRCLE ( 'NONE', #13999, 14.99999999999999645 ) ;
#14445 = EDGE_CURVE ( 'NONE', #15843, #19424, #5073, .T. ) ;
#14447 = CARTESIAN_POINT ( 'NONE',  ( -192.9588430854689989, -2.280704836619014309E-13, 54.46834944099972375 ) ) ;
#14446 = CARTESIAN_POINT ( 'NONE',  ( -280.0000000000000000, 14.14213562373108246, -14.14213562373078581 ) ) ;
#14448 = CARTESIAN_POINT ( 'NONE',  ( 163.1118516004056573, 37.29075403953132906, 19.27778845539275565 ) ) ;
#14449 = CARTESIAN_POINT ( 'NONE',  ( 23.64688638900486595, 46.70960658758650652, -13.78084749393357811 ) ) ;
#14450 = CARTESIAN_POINT ( 'NONE',  ( -30.26275506840324425, 41.69427246844628598, -40.00000000000002132 ) ) ;
#14451 = CARTESIAN_POINT ( 'NONE',  ( -280.0000000000000000, 19.99999999999996092, -0.000000000000000000 ) ) ;
#14452 = CARTESIAN_POINT ( 'NONE',  ( -91.56559293963834989, -16.03295912088706388, -16.03295912088710651 ) ) ;
#14453 = CARTESIAN_POINT ( 'NONE',  ( -5.866564133086563437, -46.35727274689649136, 13.69896896866318592 ) ) ;
#14454 = CARTESIAN_POINT ( 'NONE',  ( -162.0762913951021176, 41.69427287672986182, 40.00000000000002132 ) ) ;
#14455 = EDGE_LOOP ( 'NONE', ( #19267, #6106, #24770, #11923, #1661, #13687 ) ) ;
#14456 = LINE ( 'NONE', #20721, #20874 ) ;
#14457 = CARTESIAN_POINT ( 'NONE',  ( -213.1075012329537230, 9.698598906450410340, 9.698598906450483170 ) ) ;
#14458 = CARTESIAN_POINT ( 'NONE',  ( -5.859158571325972176, -23.09435402965430129, 42.46836465823860607 ) ) ;
#14459 = CARTESIAN_POINT ( 'NONE',  ( 8.556015491705554865, 24.84887822174884064, -44.89939803569809129 ) ) ;
#14460 = CARTESIAN_POINT ( 'NONE',  ( 199.0082207658673781, 0.6402583678929150146, -19.98857080023024579 ) ) ;
#14461 = CARTESIAN_POINT ( 'NONE',  ( -16.41654234031583570, -42.70586891223516091, -12.95560590424196690 ) ) ;
#14462 = CARTESIAN_POINT ( 'NONE',  ( 144.1620285550791323, -30.21661402164567889, 12.51613133675847678 ) ) ;
#14463 = CARTESIAN_POINT ( 'NONE',  ( -190.7346372394825380, -23.92885340724453158, 43.65255821758466936 ) ) ;
#14464 = CARTESIAN_POINT ( 'NONE',  ( 91.82158438592158234, -12.16597498399995203, -44.40256751092347542 ) ) ;
#14466 = CARTESIAN_POINT ( 'NONE',  ( 57.59792236341147031, 26.56190807104652052, 30.00663442387728708 ) ) ;
#14465 = CARTESIAN_POINT ( 'NONE',  ( -188.2957210513757218, 23.44847782072239184, -43.00408675155262728 ) ) ;
#14467 = CARTESIAN_POINT ( 'NONE',  ( 14.38125909742180220, 39.01709431150892016, 17.55144818341517166 ) ) ;
#14468 = CARTESIAN_POINT ( 'NONE',  ( -213.1075012329536946, -53.71589010951918652, -2.449293598294708485E-15 ) ) ;
#14469 = CARTESIAN_POINT ( 'NONE',  ( 151.7948205124836534, 6.767089262349056611, 40.00000000000002132 ) ) ;
#14470 = CARTESIAN_POINT ( 'NONE',  ( 19.06497207195981858, -39.99999999999987210, -14.19242893257882621 ) ) ;
#14471 = CARTESIAN_POINT ( 'NONE',  ( -238.4067589809705794, 28.96627169325315165, 28.96627169325329731 ) ) ;
#14472 = CARTESIAN_POINT ( 'NONE',  ( -88.37877758184212951, 20.15391234942320509, -8.026456973658891769 ) ) ;
#14473 = CARTESIAN_POINT ( 'NONE',  ( -192.9588430854690273, -10.23066800231931239, -66.79921049724377724 ) ) ;
#14474 = CARTESIAN_POINT ( 'NONE',  ( 200.0000000000000000, 42.42640687119290988, 14.14213562373111976 ) ) ;
#14475 = ORIENTED_EDGE ( 'NONE', *, *, #15195, .F. ) ;
#14476 = DIRECTION ( 'NONE',  ( 0.000000000000000000, -1.000000000000000000, 0.000000000000000000 ) ) ;
#14477 = AXIS2_PLACEMENT_3D ( 'NONE', #2718, #24801, #17066 ) ;
#14478 = CARTESIAN_POINT ( 'NONE',  ( -88.37877758183735466, 8.575405934691293197, 19.92653024471085033 ) ) ;
#14479 = CARTESIAN_POINT ( 'NONE',  ( -192.9588430854689705, -38.51493924976963967, 38.51493924976919914 ) ) ;
#14480 = CARTESIAN_POINT ( 'NONE',  ( -4.061681315507726708, -42.99867639910917916, -23.44498947467575789 ) ) ;
#14481 = ORIENTED_EDGE ( 'NONE', *, *, #9480, .T. ) ;
#14482 = CARTESIAN_POINT ( 'NONE',  ( 184.8905102610680444, -20.92133201514440799, 0.000000000000000000 ) ) ;
#14483 = CARTESIAN_POINT ( 'NONE',  ( -82.23726319249651340, -14.28014421912411080, -14.28014421912424581 ) ) ;
#14484 = ADVANCED_FACE ( 'NONE', ( #3772 ), #12148, .F. ) ;
#14485 = ORIENTED_EDGE ( 'NONE', *, *, #24547, .F. ) ;
#14486 = CARTESIAN_POINT ( 'NONE',  ( 199.9999999999996874, 18.57765777299087873, -3.990914148134230288 ) ) ;
#14487 = CARTESIAN_POINT ( 'NONE',  ( 22.27434459962515234, 13.86259002496867154, -47.22399357564341926 ) ) ;
#14488 = CARTESIAN_POINT ( 'NONE',  ( -188.2507053402904660, -42.99082124348477407, -23.43979243030716475 ) ) ;
#14489 = CARTESIAN_POINT ( 'NONE',  ( -30.26275506840324070, -40.00000000000003553, 1.694272468446120117 ) ) ;
#14490 = CARTESIAN_POINT ( 'NONE',  ( -192.9588430854690273, 54.46834944098218756, -40.00000000000002132 ) ) ;
#14491 = CARTESIAN_POINT ( 'NONE',  ( 146.6084372240433993, -24.48358557860353457, 24.48358557860296258 ) ) ;
#14492 = CARTESIAN_POINT ( 'NONE',  ( 199.0249982833957176, -5.192600369583379560, 19.31944532238548362 ) ) ;
#14493 = AXIS2_PLACEMENT_3D ( 'NONE', #15703, #23827, #24100 ) ;
#14494 = EDGE_CURVE ( 'NONE', #7095, #1180, #740, .T. ) ;
#14495 = CARTESIAN_POINT ( 'NONE',  ( 57.59792236341147742, -1.230234673553095937E-13, 37.56421063658186199 ) ) ;
#14496 = CARTESIAN_POINT ( 'NONE',  ( -198.0356074513804572, 39.99999999999992895, 15.37879056873084771 ) ) ;
#14497 = DIRECTION ( 'NONE',  ( 0.000000000000000000, 1.000000000000000000, 0.000000000000000000 ) ) ;
#14498 = FACE_OUTER_BOUND ( 'NONE', #4853, .T. ) ;
#14499 = CARTESIAN_POINT ( 'NONE',  ( -208.1127848780264742, -55.00245453010926866, 40.00000000000002132 ) ) ;
#14500 = CARTESIAN_POINT ( 'NONE',  ( 19.06497207195981858, -10.03556273973469715, 66.60410523465813526 ) ) ;
#14501 = CARTESIAN_POINT ( 'NONE',  ( -30.26275506840324070, 1.218738420030236455E-14, -1.694272468446259783 ) ) ;
#14502 = PLANE ( 'NONE',  #7251 ) ;
#14503 = CARTESIAN_POINT ( 'NONE',  ( 4.995406935893291767, 40.00000000000059686, -55.24977328853165659 ) ) ;
#14504 = CARTESIAN_POINT ( 'NONE',  ( -208.1127848780264742, -40.00000000000025580, 55.00245453014408525 ) ) ;
#14505 = CARTESIAN_POINT ( 'NONE',  ( 199.0262120803540995, -11.39568569719682145, 16.44280778893389439 ) ) ;
#14506 = CARTESIAN_POINT ( 'NONE',  ( -716.9846540392142060, 82.50000000000008527, 52.49999999999980105 ) ) ;
#14507 = CARTESIAN_POINT ( 'NONE',  ( -105.4741150117383341, -8.366608964593364561, -19.60045294982747777 ) ) ;
#14508 = CARTESIAN_POINT ( 'NONE',  ( -259.2033419157646676, -49.83842185052031937, -6.730120644403796426 ) ) ;
#14509 = ORIENTED_EDGE ( 'NONE', *, *, #4457, .T. ) ;
#14510 = CARTESIAN_POINT ( 'NONE',  ( 170.2234770963711128, -17.36149277827010096, 17.36149277826970660 ) ) ;
#14511 = CARTESIAN_POINT ( 'NONE',  ( 146.5090579137182374, 29.94463907179421369, -12.40347562390439329 ) ) ;
#14512 = CARTESIAN_POINT ( 'NONE',  ( 184.8905102610680444, -19.07866798485553872, -40.00000000000002132 ) ) ;
#14513 = CARTESIAN_POINT ( 'NONE',  ( -114.7252611291635702, 17.87002000140834568, -12.98773421616931856 ) ) ;
#14514 = CARTESIAN_POINT ( 'NONE',  ( 163.1118516004056573, -19.27778845538787422, 19.27778845538743724 ) ) ;
#14515 = ORIENTED_EDGE ( 'NONE', *, *, #9534, .F. ) ;
#14516 = ORIENTED_EDGE ( 'NONE', *, *, #2252, .T. ) ;
#14517 = VECTOR ( 'NONE', #18348, 1000.000000000000000 ) ;
#14518 = CARTESIAN_POINT ( 'NONE',  ( 199.9999999999999147, -5.232840745185569631, 18.27603213255494552 ) ) ;
#14519 = CARTESIAN_POINT ( 'NONE',  ( 118.9130007099546873, 10.68958087202350704, -25.80693111732284351 ) ) ;
#14520 = CARTESIAN_POINT ( 'NONE',  ( 21.60666276258909591, 18.00814241471010391, 43.47550165074856920 ) ) ;
#14521 = ORIENTED_EDGE ( 'NONE', *, *, #24689, .F. ) ;
#14522 = ADVANCED_FACE ( 'NONE', ( #20406 ), #16267, .F. ) ;
#14523 = EDGE_LOOP ( 'NONE', ( #7400, #19837, #1461, #20111 ) ) ;
#14524 = CARTESIAN_POINT ( 'NONE',  ( -238.4067589809705794, 0.6820004457340470561, 57.25054294065803617 ) ) ;
#14525 = CARTESIAN_POINT ( 'NONE',  ( 199.0168191192024949, -15.25344411108907572, -12.94054329384263724 ) ) ;
#14526 = CARTESIAN_POINT ( 'NONE',  ( -105.3846709043738628, 6.705972854959187934, 20.33574920591904700 ) ) ;
#14527 = CARTESIAN_POINT ( 'NONE',  ( 91.82158438592158234, -12.16597498397761967, -12.16597498397768007 ) ) ;
#14528 = CARTESIAN_POINT ( 'NONE',  ( -162.0762913951020892, 57.76657433537918251, 1.198031840455469066 ) ) ;
#14529 = CARTESIAN_POINT ( 'NONE',  ( -109.1264249741455927, -33.12752917269520481, -13.72187187123273411 ) ) ;
#14530 = EDGE_CURVE ( 'NONE', #4513, #19805, #11743, .T. ) ;
#14531 = ADVANCED_FACE ( 'NONE', ( #20270 ), #19619, .T. ) ;
#14532 = CARTESIAN_POINT ( 'NONE',  ( -99.31267923333118119, -8.544756979489637416, -20.62886818714801507 ) ) ;
#14533 = CARTESIAN_POINT ( 'NONE',  ( 170.2234770963711128, 1.955190573858485757E-13, -15.44714144992816074 ) ) ;
#14534 = CARTESIAN_POINT ( 'NONE',  ( 146.6084372240433709, 39.99999999999968026, 34.62501878078347772 ) ) ;
#14535 = CARTESIAN_POINT ( 'NONE',  ( -627.5046577674308992, 26.45751311064576683, 30.00000000000004974 ) ) ;
#14536 = VECTOR ( 'NONE', #5673, 1000.000000000000000 ) ;
#14537 = CARTESIAN_POINT ( 'NONE',  ( -210.0000000000000284, 63.70262460423102624, -57.69613583541415380 ) ) ;
#14538 = CARTESIAN_POINT ( 'NONE',  ( 199.0070875033960078, 19.58406838943379569, -4.039067077891903779 ) ) ;
#14539 = CARTESIAN_POINT ( 'NONE',  ( -188.3065677117054122, 13.82848612971594804, 46.99298756134906085 ) ) ;
#14540 = CARTESIAN_POINT ( 'NONE',  ( -30.26275506840324070, -1.198031551616016266, -1.198031551616031587 ) ) ;
#14541 = CARTESIAN_POINT ( 'NONE',  ( 98.29820294267436509, 14.14213562374297695, -14.14213562372651189 ) ) ;
#14542 = CARTESIAN_POINT ( 'NONE',  ( -86.96347745069643054, 15.38646221621763210, 41.18208027870604582 ) ) ;
#14543 = CARTESIAN_POINT ( 'NONE',  ( -190.0000000000000000, 52.50000000000007816, -52.49999999999999289 ) ) ;
#14544 = CARTESIAN_POINT ( 'NONE',  ( -198.0356074513804572, -10.87444709758429262, -67.44298959250878056 ) ) ;
#14545 = CARTESIAN_POINT ( 'NONE',  ( -651.9208163904479534, 37.70578118159719594, 24.56594063796493543 ) ) ;
#14546 = CARTESIAN_POINT ( 'NONE',  ( -56.48582580120559271, 9.153146818113576444, -0.000000000000000000 ) ) ;
#14547 = CARTESIAN_POINT ( 'NONE',  ( -86.96347745069644475, -15.38646221621807442, 15.38646221621768184 ) ) ;
#14548 = CARTESIAN_POINT ( 'NONE',  ( -30.26275506840324425, -1.694272468446265334, 40.00000000000002132 ) ) ;
#14549 = CARTESIAN_POINT ( 'NONE',  ( -617.6056806187223174, 29.79386004448080172, -33.72500239264033439 ) ) ;
#14550 = CARTESIAN_POINT ( 'NONE',  ( 19.06497207195980792, 40.00000000000059686, -54.19242893257802507 ) ) ;
#14551 = CARTESIAN_POINT ( 'NONE',  ( 199.0132069300353805, -9.958817830381372360, -17.35495257061628038 ) ) ;
#14552 = CARTESIAN_POINT ( 'NONE',  ( 140.2235668266256141, -12.60094438999861666, 30.42137084504290812 ) ) ;
#14553 = EDGE_LOOP ( 'NONE', ( #17132, #5236 ) ) ;
#14554 = ORIENTED_EDGE ( 'NONE', *, *, #11999, .T. ) ;
#14555 = CARTESIAN_POINT ( 'NONE',  ( 91.82158438592158234, -17.20528682183298486, 0.000000000000000000 ) ) ;
#14556 = CARTESIAN_POINT ( 'NONE',  ( 154.0339099654742654, 11.67508747798851587, 28.18615453125295645 ) ) ;
#14557 = CARTESIAN_POINT ( 'NONE',  ( 192.4448373802101173, 42.42640687116487896, 14.14213562375934075 ) ) ;
#14558 = DIRECTION ( 'NONE',  ( 0.7071067811865500152, 8.659560562354903276E-17, 0.7071067811865451302 ) ) ;
#14559 = CARTESIAN_POINT ( 'NONE',  ( -190.1935349183499397, -43.51927535257652835, -23.83022391594517586 ) ) ;
#14560 = CARTESIAN_POINT ( 'NONE',  ( -200.0000000000000000, -71.50000000000002842, 66.50000000000005684 ) ) ;
#14561 = CARTESIAN_POINT ( 'NONE',  ( 199.9999999999998863, -3.863658434880562265, -18.60611098383053630 ) ) ;
#14562 = CARTESIAN_POINT ( 'NONE',  ( 199.9999999999998863, 13.43021917686961331, -13.43983678748323918 ) ) ;
#14563 = CARTESIAN_POINT ( 'NONE',  ( 0.2972598230769990524, -18.14793986248671231, -38.42060263243687501 ) ) ;
#14564 = CARTESIAN_POINT ( 'NONE',  ( 192.4448373802100889, 14.14213562375873678, 14.14213562375894817 ) ) ;
#14565 = DIRECTION ( 'NONE',  ( 1.000000000000000000, 1.836970198721030427E-16, -0.000000000000000000 ) ) ;
#14566 = CARTESIAN_POINT ( 'NONE',  ( 192.4448373802100889, -1.741373372144848397E-13, 20.00000000003942091 ) ) ;
#14567 = CARTESIAN_POINT ( 'NONE',  ( -100.7734535825088500, -40.53558337403692491, 16.03295912088671571 ) ) ;
#14568 = CARTESIAN_POINT ( 'NONE',  ( -86.96347745069645896, 21.75974354311648895, -0.000000000000000000 ) ) ;
#14569 = CARTESIAN_POINT ( 'NONE',  ( 151.7948205124836250, -23.49921654116371883, 23.49921654116317526 ) ) ;
#14570 = CARTESIAN_POINT ( 'NONE',  ( 57.59792236341147031, 1.722363176415065089, -1.722363176415036445 ) ) ;
#14571 = CARTESIAN_POINT ( 'NONE',  ( 199.0084504823431359, 19.99625238461678478, -0.02475617773853401246 ) ) ;
#14572 = SHAPE_REPRESENTATION ( 'Baseplate', ( #21058 ), #4064 ) ;
#14574 = CARTESIAN_POINT ( 'NONE',  ( 0.2972598230770030492, -1.921041075453695163E-13, 54.33493731733936016 ) ) ;
#14573 = CARTESIAN_POINT ( 'NONE',  ( 57.59792236341147031, 26.56190807104720975, -26.56190807104655249 ) ) ;
#14575 = CARTESIAN_POINT ( 'NONE',  ( -56.48582580120559982, 50.09629031063956717, 6.472252184284792875 ) ) ;
#14576 = CARTESIAN_POINT ( 'NONE',  ( 23.17367289775668837, 42.91822977676283557, -23.38495170326041617 ) ) ;
#14577 = CARTESIAN_POINT ( 'NONE',  ( -100.7734535825088358, 17.32597176626809343, 2.449293598294708485E-15 ) ) ;
#14578 = CARTESIAN_POINT ( 'NONE',  ( -350.0000000000001137, -4.857225732735059864E-14, -21.53474504356805852 ) ) ;
#14579 = CARTESIAN_POINT ( 'NONE',  ( -162.0762913951021176, 1.694272876828294194, 40.00000000000002132 ) ) ;
#14580 = CARTESIAN_POINT ( 'NONE',  ( -70.35386311710972507, -23.12931224182874956, 8.707385197621585249 ) ) ;
#14581 = CARTESIAN_POINT ( 'NONE',  ( 200.0000000000000000, -20.00000000000006750, 40.00000000000002132 ) ) ;
#14582 = EDGE_LOOP ( 'NONE', ( #12621, #698, #22315, #18744, #24737 ) ) ;
#14583 = CARTESIAN_POINT ( 'NONE',  ( -200.0000000000000000, 43.94911113647449241, 34.07282666716778152 ) ) ;
#14584 = CARTESIAN_POINT ( 'NONE',  ( -105.3755690713226585, -43.67073346367983788, 12.89780903124397149 ) ) ;
#14585 = DIRECTION ( 'NONE',  ( 0.000000000000000000, -1.000000000000000000, 0.000000000000000000 ) ) ;
#14586 = EDGE_CURVE ( 'NONE', #18845, #22942, #7082, .T. ) ;
#14587 = CARTESIAN_POINT ( 'NONE',  ( -3.534370630407255742, 17.92707699455486292, -43.27979241395905774 ) ) ;
#14588 = CARTESIAN_POINT ( 'NONE',  ( 199.0260304748864257, -17.33599623264176870, 10.00424117181305128 ) ) ;
#14589 = CARTESIAN_POINT ( 'NONE',  ( 146.6084372240433993, -24.48358557860353457, 24.48358557860296258 ) ) ;
#14590 = CARTESIAN_POINT ( 'NONE',  ( -87.02123777076587885, -20.76518631980179563, 5.414077845906299480 ) ) ;
#14591 = CARTESIAN_POINT ( 'NONE',  ( -188.2652746676491233, -23.44263257803716627, 42.99511404081857080 ) ) ;
#14592 = CARTESIAN_POINT ( 'NONE',  ( 57.59792236341148453, -40.00000000000003553, 2.435789363417741438 ) ) ;
#14593 = CARTESIAN_POINT ( 'NONE',  ( -105.3755690713226585, -43.67073346367964604, -12.89780903124457545 ) ) ;
#14594 = CARTESIAN_POINT ( 'NONE',  ( 57.59792236341147031, 2.435789363418171760, 0.000000000000000000 ) ) ;
#14596 = CARTESIAN_POINT ( 'NONE',  ( -192.9588430854690273, 66.79921049724377724, -10.23066800231904239 ) ) ;
#14595 = CARTESIAN_POINT ( 'NONE',  ( -188.6890294954778824, 13.84869711777474954, -47.12920239600426697 ) ) ;
#14597 = CARTESIAN_POINT ( 'NONE',  ( 136.1360204305621266, -24.77266263493151044, 24.77266263493093135 ) ) ;
#14598 = CARTESIAN_POINT ( 'NONE',  ( 163.1118516004056573, -12.73709011382471878, -40.00000000000002132 ) ) ;
#14599 = CARTESIAN_POINT ( 'NONE',  ( 4.995406935893288214, 55.24977328853207581, 40.00000000000002132 ) ) ;
#14600 = CARTESIAN_POINT ( 'NONE',  ( -208.1127848780265026, 1.189126717069624012E-13, -15.00245453012669472 ) ) ;
#14601 = CARTESIAN_POINT ( 'NONE',  ( -213.1075012329537230, 37.98287015391228749, 37.98287015391245802 ) ) ;
#14602 = CARTESIAN_POINT ( 'NONE',  ( -100.0957100001388937, 20.56213589530717911, -8.517115559260082236 ) ) ;
#14603 = CARTESIAN_POINT ( 'NONE',  ( 136.1360204305621266, -3.511608612530630058, -3.511608612530719764 ) ) ;
#14604 = CARTESIAN_POINT ( 'NONE',  ( -114.7252611291633997, 3.452297386453677230, 21.81972725943348834 ) ) ;
#14605 = ORIENTED_EDGE ( 'NONE', *, *, #5075, .F. ) ;
#14606 = CARTESIAN_POINT ( 'NONE',  ( -162.0762913951021176, -27.08623940707624911, 29.48230308784761888 ) ) ;
#14607 = CARTESIAN_POINT ( 'NONE',  ( 192.4448373802101173, 14.14213562375862665, 42.42640687116509213 ) ) ;
#14608 = CARTESIAN_POINT ( 'NONE',  ( -3.786831587088177020, -47.08106124085814059, -13.84155926340365639 ) ) ;
#14609 = ORIENTED_EDGE ( 'NONE', *, *, #19308, .T. ) ;
#14610 = CARTESIAN_POINT ( 'NONE',  ( -716.9846540392142060, 66.50000000000009948, -71.50000000000005684 ) ) ;
#14611 = CARTESIAN_POINT ( 'NONE',  ( -200.0000000000000284, -30.70179486994606677, 44.88127304974057097 ) ) ;
#14612 = EDGE_LOOP ( 'NONE', ( #8267, #15549 ) ) ;
#14613 = CARTESIAN_POINT ( 'NONE',  ( 200.0000000000000853, 16.14603016630555743, -10.01676266068942667 ) ) ;
#14614 = DIRECTION ( 'NONE',  ( -1.000000000000000000, -1.836970198721024264E-16, 0.000000000000000000 ) ) ;
#14615 = CARTESIAN_POINT ( 'NONE',  ( -91.56559293963834989, -7.976292724337646577E-14, 17.32597176626811120 ) ) ;
#14616 = CARTESIAN_POINT ( 'NONE',  ( -238.4067589809705794, 40.96449428006337001, -40.00000000000002132 ) ) ;
#14617 = CARTESIAN_POINT ( 'NONE',  ( -210.0000000000000284, 57.47694228411666728, -64.52066607436458412 ) ) ;
#14618 = CARTESIAN_POINT ( 'NONE',  ( 199.0254609980498799, -7.058152949095585882, 18.72097443096651403 ) ) ;
#14619 = CARTESIAN_POINT ( 'NONE',  ( 0.2972598230770153171, -66.70487387989849992, -10.13633138497533004 ) ) ;
#14620 = CARTESIAN_POINT ( 'NONE',  ( 151.7948205124836250, 1.807796684091926154E-15, 6.767089262349031742 ) ) ;
#14621 = CARTESIAN_POINT ( 'NONE',  ( -86.96347745069645896, 40.00000000000008527, -21.75974354311636461 ) ) ;
#14622 = LINE ( 'NONE', #20761, #14689 ) ;
#14623 = CARTESIAN_POINT ( 'NONE',  ( -105.3755690713226585, 21.75974354311648185, -40.00000000000002132 ) ) ;
#14624 = CARTESIAN_POINT ( 'NONE',  ( 0.2972598230770129857, -54.33493731733936016, -40.00000000000002132 ) ) ;
#14625 = CARTESIAN_POINT ( 'NONE',  ( -86.96347745069643054, 15.38646221621763210, 41.18208027870604582 ) ) ;
#14626 = CARTESIAN_POINT ( 'NONE',  ( -259.2033419157646676, -1.473088368616265084E-13, 9.517827891722632216 ) ) ;
#14627 = FACE_OUTER_BOUND ( 'NONE', #19984, .T. ) ;
#14628 = CARTESIAN_POINT ( 'NONE',  ( -86.96347745069644475, 1.775309070576523494E-13, -18.24025645688352881 ) ) ;
#14629 = CARTESIAN_POINT ( 'NONE',  ( -192.9588430854689989, -2.280704836619014309E-13, 54.46834944099972375 ) ) ;
#14630 = CARTESIAN_POINT ( 'NONE',  ( 199.0260264921024316, -10.00558763687667962, 17.32375098348098419 ) ) ;
#14631 = CARTESIAN_POINT ( 'NONE',  ( 48.46158931187873975, -18.19743074333925748, 35.02055581498667181 ) ) ;
#14632 = FACE_OUTER_BOUND ( 'NONE', #11388, .T. ) ;
#14633 = CARTESIAN_POINT ( 'NONE',  ( -100.7734535825088358, -12.25131212657493052, 12.25131212657478130 ) ) ;
#14634 = VERTEX_POINT ( 'NONE', #25198 ) ;
#14635 = CARTESIAN_POINT ( 'NONE',  ( -62.79433447046256589, 24.94280497471530111, -11.74096317463568795 ) ) ;
#14636 = CARTESIAN_POINT ( 'NONE',  ( 135.5356265174577572, 30.20731421070355083, -12.51227922893884248 ) ) ;
#14637 = CARTESIAN_POINT ( 'NONE',  ( 19.06497207195980792, -14.19242893257839988, -40.00000000000002132 ) ) ;
#14638 = CARTESIAN_POINT ( 'NONE',  ( 190.0000000000000000, -35.78896085774750446, 82.49999999999998579 ) ) ;
#14639 = CARTESIAN_POINT ( 'NONE',  ( -188.2995950289364089, -43.00522595870943832, -23.44932284466036521 ) ) ;
#14640 = VERTEX_POINT ( 'NONE', #5098 ) ;
#14641 = VERTEX_POINT ( 'NONE', #25701 ) ;
#14642 = EDGE_CURVE ( 'NONE', #13720, #12829, #12639, .T. ) ;
#14643 = CARTESIAN_POINT ( 'NONE',  ( 200.0000000000000284, 4.005278531425509492, 18.58194003000864569 ) ) ;
#14644 = CARTESIAN_POINT ( 'NONE',  ( -88.38011429762325122, 8.298859915237940754, -20.03522015860023942 ) ) ;
#14645 = CARTESIAN_POINT ( 'NONE',  ( 20.17262239842997928, 18.14389419514546375, 43.80323544018629178 ) ) ;
#14646 = ORIENTED_EDGE ( 'NONE', *, *, #20204, .T. ) ;
#14647 = ORIENTED_EDGE ( 'NONE', *, *, #21180, .T. ) ;
#14648 = CARTESIAN_POINT ( 'NONE',  ( 57.59792236341147031, -1.722363176415032004, -1.722363176415048880 ) ) ;
#14649 = CARTESIAN_POINT ( 'NONE',  ( 199.0260304748864257, -17.33599623264176870, 10.00424117181305128 ) ) ;
#14650 = CARTESIAN_POINT ( 'NONE',  ( -105.2054292635174875, -16.16779360711802127, -14.22820282028660799 ) ) ;
#14651 = CARTESIAN_POINT ( 'NONE',  ( -208.1127848780264742, -17.67593391476659548, 38.89260858015730804 ) ) ;
#14652 = CARTESIAN_POINT ( 'NONE',  ( -210.0000000000000284, 0.000000000000000000, 0.000000000000000000 ) ) ;
#14653 = CARTESIAN_POINT ( 'NONE',  ( -102.2610585947573298, 5.898343112255980222E-14, -22.27377874548543701 ) ) ;
#14654 = CARTESIAN_POINT ( 'NONE',  ( 150.0000000000000284, -135.7889608577475258, 82.50000000000001421 ) ) ;
#14655 = CARTESIAN_POINT ( 'NONE',  ( -213.1075012329537230, 5.259461644596141978E-13, -53.71589010951915100 ) ) ;
#14656 = AXIS2_PLACEMENT_3D ( 'NONE', #20675, #4448, #8420 ) ;
#14657 = CARTESIAN_POINT ( 'NONE',  ( 91.82158438592158234, -1.633484621919921769E-13, 17.20528682183300262 ) ) ;
#14658 = CARTESIAN_POINT ( 'NONE',  ( -4.039451493210496125, 23.44932283416649454, 43.00522595894017286 ) ) ;
#14659 = DIRECTION ( 'NONE',  ( -1.000000000000000000, -1.836970198721030181E-16, -2.465190328815661892E-32 ) ) ;
#14660 = CARTESIAN_POINT ( 'NONE',  ( 199.0065089264240044, 19.04284699271596537, -6.106433644136123995 ) ) ;
#14661 = CARTESIAN_POINT ( 'NONE',  ( -189.6939181379233901, 18.01964634722543579, 43.50327460064161755 ) ) ;
#14662 = CARTESIAN_POINT ( 'NONE',  ( 184.8905102610680444, 14.79361573936375507, 14.79361573936398067 ) ) ;
#14663 = ADVANCED_FACE ( 'NONE', ( #23443 ), #21351, .T. ) ;
#14664 = LINE ( 'NONE', #6553, #14920 ) ;
#14665 = B_SPLINE_CURVE_WITH_KNOTS ( 'NONE', 3,
 ( #11696, #15558, #19821, #24081, #13565, #25826 ),
 .UNSPECIFIED., .F., .F.,
 ( 4, 2, 4 ),
 ( 0.3689590070116581244, 0.3867117631979620773, 0.4044645193949217843 ),
 .UNSPECIFIED. ) ;
#14666 = CARTESIAN_POINT ( 'NONE',  ( 199.9999999999999432, -14.14213562373093680, 14.14213562373082311 ) ) ;
#14667 = DIRECTION ( 'NONE',  ( 0.000000000000000000, 0.3656393565213325592, 0.9307566067252307507 ) ) ;
#14668 = AXIS2_PLACEMENT_3D ( 'NONE', #19880, #3393, #9903 ) ;
#14669 = CIRCLE ( 'NONE', #12991, 15.00000000000000178 ) ;
#14670 = CARTESIAN_POINT ( 'NONE',  ( 200.0000000000000000, 14.14213562373142352, -42.42640687119268961 ) ) ;
#14671 = CARTESIAN_POINT ( 'NONE',  ( -199.9999999999998579, 44.86878812508723513, -24.82633483071237634 ) ) ;
#14672 = CARTESIAN_POINT ( 'NONE',  ( 0.2972598230769983307, -14.33493731733933352, 0.000000000000000000 ) ) ;
#14673 = ADVANCED_FACE ( 'NONE', ( #1196 ), #6038, .T. ) ;
#14674 = CARTESIAN_POINT ( 'NONE',  ( 91.82158438592158234, 16.11829626348378142, 40.45024623143977749 ) ) ;
#14675 = CARTESIAN_POINT ( 'NONE',  ( 57.59792236341147031, 2.435789363418171760, 0.000000000000000000 ) ) ;
#14676 = CARTESIAN_POINT ( 'NONE',  ( -603.9947245077624984, 36.43016709300914613, -26.48061427247913002 ) ) ;
#14677 = B_SPLINE_CURVE_WITH_KNOTS ( 'NONE', 3,
 ( #17038, #4419, #559, #18640, #8664, #22775 ),
 .UNSPECIFIED., .F., .F.,
 ( 4, 2, 4 ),
 ( 0.000000000000000000, 0.004089908668607722744, 0.008179817337215445489 ),
 .UNSPECIFIED. ) ;
#14678 = CARTESIAN_POINT ( 'NONE',  ( 136.1360204305621551, -39.99999999999994316, -4.966164525587488221 ) ) ;
#14679 = ADVANCED_FACE ( 'NONE', ( #20277, #2187, #23989, #8285, #26012, #18265 ), #17861, .T. ) ;
#14680 = CARTESIAN_POINT ( 'NONE',  ( 199.0119150821959124, -7.654620711488286489, -18.47502128564530466 ) ) ;
#14681 = ADVANCED_FACE ( 'NONE', ( #7748 ), #20412, .F. ) ;
#14682 = CARTESIAN_POINT ( 'NONE',  ( -210.0000000000000284, -52.49999999999991473, 82.49999999999998579 ) ) ;
#14683 = EDGE_LOOP ( 'NONE', ( #2037, #7850, #7681, #1958 ) ) ;
#14684 = ORIENTED_EDGE ( 'NONE', *, *, #10872, .T. ) ;
#14685 = ORIENTED_EDGE ( 'NONE', *, *, #6062, .T. ) ;
#14686 = CARTESIAN_POINT ( 'NONE',  ( -208.1127848780264742, 55.00245453014418473, 40.00000000000002132 ) ) ;
#14687 = CARTESIAN_POINT ( 'NONE',  ( 147.2817042152898921, 12.35516179550106131, 29.82799917201331752 ) ) ;
#14688 = CIRCLE ( 'NONE', #3224, 5.000000000000007994 ) ;
#14689 = VECTOR ( 'NONE', #19025, 1000.000000000000000 ) ;
#14690 = CARTESIAN_POINT ( 'NONE',  ( -208.1127848780265026, 38.89260858015777700, -38.89260858015687461 ) ) ;
#14691 = CARTESIAN_POINT ( 'NONE',  ( -110.1003821002955476, -20.16525298256173926, 1.261039542895599830 ) ) ;
#14692 = PLANE ( 'NONE',  #20219 ) ;
#14693 = DIRECTION ( 'NONE',  ( -0.7071067811865499042, -0.7071067811865451302, 0.000000000000000000 ) ) ;
#14694 = CARTESIAN_POINT ( 'NONE',  ( 199.9999999999997726, 13.87428525677396607, -12.99608892921076198 ) ) ;
#14695 = VECTOR ( 'NONE', #10406, 1000.000000000000000 ) ;
#14696 = CARTESIAN_POINT ( 'NONE',  ( 200.0000000000000000, 12.98760816711885724, -13.88210512389335527 ) ) ;
#14697 = CARTESIAN_POINT ( 'NONE',  ( 163.1118516004056573, -47.56205970284945295, -9.006482792074823607 ) ) ;
#14698 = CARTESIAN_POINT ( 'NONE',  ( 151.7948205124835681, -4.785054706298876859, 51.78348778862533663 ) ) ;
#14699 = CARTESIAN_POINT ( 'NONE',  ( -114.4364955367327212, -20.04994829327665684, -8.644468109209087814 ) ) ;
#14700 = CARTESIAN_POINT ( 'NONE',  ( 57.59792236341146321, 40.00000000000000711, 2.435789363418579434 ) ) ;
#14701 = AXIS2_PLACEMENT_3D ( 'NONE', #15362, #11754, #13882 ) ;
#14702 = CARTESIAN_POINT ( 'NONE',  ( -83.21262154144250189, 33.12752917118434226, -13.72187187061452107 ) ) ;
#14703 = CARTESIAN_POINT ( 'NONE',  ( -280.0000000000000000, 19.99999999999996092, -0.000000000000000000 ) ) ;
#14704 = CARTESIAN_POINT ( 'NONE',  ( 0.2972598230769938343, 10.13633138497472252, 10.13633138497475628 ) ) ;
#14705 = CARTESIAN_POINT ( 'NONE',  ( 0.2972598230770153171, -66.70487387989861361, 10.13633138497438324 ) ) ;
#14706 = CARTESIAN_POINT ( 'NONE',  ( 199.0056809825925370, 17.31175780291549415, -10.02710580630489900 ) ) ;
#14708 = CARTESIAN_POINT ( 'NONE',  ( -105.3755690713226585, 39.99999999999993605, 18.24025645688366737 ) ) ;
#14707 = CARTESIAN_POINT ( 'NONE',  ( 192.4448373802101173, -14.14213562375826605, -42.42640687116518450 ) ) ;
#14709 = CLOSED_SHELL ( 'NONE', ( #22016, #6720, #612, #16473, #21026, #2980, #22589, #13376, #21593, #8672, #12237, #15396, #13129, #22165, #13346, #23462, #16453, #3812, #23084, #2016, #21489, #25442, #13658, #11112, #10304, #18234, #16295, #16957, #21985, #17209 ) ) ;
#14710 = CARTESIAN_POINT ( 'NONE',  ( 23.58679727197014842, 42.79169916605225410, -23.29637218065878201 ) ) ;
#14711 = CARTESIAN_POINT ( 'NONE',  ( -208.1127848780265026, 15.00245453012665564, 0.000000000000000000 ) ) ;
#14712 = CARTESIAN_POINT ( 'NONE',  ( -162.0762913951021176, 1.198031840315997298, 57.76657433523996588 ) ) ;
#14713 = CARTESIAN_POINT ( 'NONE',  ( 57.59792236341147031, -2.435789363418150000, 40.00000000000002132 ) ) ;
#14714 = CARTESIAN_POINT ( 'NONE',  ( -47.65341557551062834, -31.50022537346376694, 10.55973086694773855 ) ) ;
#14715 = CARTESIAN_POINT ( 'NONE',  ( 170.2234770963711128, -24.55285855007184281, 40.00000000000002132 ) ) ;
#14716 = EDGE_LOOP ( 'NONE', ( #2978, #24983, #17419, #957 ) ) ;
#14717 = CARTESIAN_POINT ( 'NONE',  ( -350.0000000000001137, -4.467814962633844109E-14, -31.79780246617542616 ) ) ;
#14718 = CARTESIAN_POINT ( 'NONE',  ( -192.9588430854690273, -18.05360324515454096, 38.51493924976936967 ) ) ;
#14719 = CARTESIAN_POINT ( 'NONE',  ( -4.421177063212223146, -13.80119274858222944, 46.85829989839683662 ) ) ;
#14720 = CARTESIAN_POINT ( 'NONE',  ( -5.379830816902851254, 23.18791234549835423, -42.60994460517710536 ) ) ;
#14721 = CARTESIAN_POINT ( 'NONE',  ( 199.0208257245452899, -19.09599194444923143, -5.955353076589812389 ) ) ;
#14722 = CARTESIAN_POINT ( 'NONE',  ( 170.2234770963711128, -17.36149277827010096, 17.36149277826970660 ) ) ;
#14723 = DIRECTION ( 'NONE',  ( 0.000000000000000000, 1.000000000000000000, 0.000000000000000000 ) ) ;
#14724 = CARTESIAN_POINT ( 'NONE',  ( -87.02142894580205734, 5.408203463865087102, 20.76642173393088342 ) ) ;
#14725 = CARTESIAN_POINT ( 'NONE',  ( -188.9266751785327756, -17.94050871568869354, 43.31221945728800193 ) ) ;
#14726 = CARTESIAN_POINT ( 'NONE',  ( -198.0356074513804572, -10.87444709759714634, -10.87444709759729911 ) ) ;
#14727 = CARTESIAN_POINT ( 'NONE',  ( 151.7948205124836534, -51.78348778862529400, -4.785054706299085581 ) ) ;
#14728 = DIRECTION ( 'NONE',  ( 0.000000000000000000, 1.000000000000000000, 0.000000000000000000 ) ) ;
#14730 = CARTESIAN_POINT ( 'NONE',  ( 91.82158438592158234, 16.11829626346161604, -16.11829626346121103 ) ) ;
#14729 = CARTESIAN_POINT ( 'NONE',  ( 136.1360204305621266, 24.77266263493104148, 24.77266263493145004 ) ) ;
#14731 = CARTESIAN_POINT ( 'NONE',  ( 184.8905102610680444, 13.49065550809757497, 43.07788698682593065 ) ) ;
#14732 = CARTESIAN_POINT ( 'NONE',  ( -208.1127848780264742, -55.00245453012676222, -2.449293598294708485E-15 ) ) ;
#14733 = CARTESIAN_POINT ( 'NONE',  ( 0.2972598230769930572, 54.33493731733936016, 2.449293598294708485E-15 ) ) ;
#14734 = CARTESIAN_POINT ( 'NONE',  ( 151.7948205124836534, -40.00000000000034817, 33.23291073765511072 ) ) ;
#14735 = CARTESIAN_POINT ( 'NONE',  ( 4.995406935893287326, 67.35176059882533650, 10.78321810390163549 ) ) ;
#14736 = CIRCLE ( 'NONE', #2000, 5.000000000000046185 ) ;
#14737 = CARTESIAN_POINT ( 'NONE',  ( -100.0968563617409330, 20.72609133245494917, -8.149320301549584755 ) ) ;
#14738 = CARTESIAN_POINT ( 'NONE',  ( 19.06497207195982568, -38.31983398719592770, -38.31983398719660272 ) ) ;
#14739 = CARTESIAN_POINT ( 'NONE',  ( -30.26275506840324070, -1.198031551616032919, 1.198031551616014712 ) ) ;
#14740 = VERTEX_POINT ( 'NONE', #11749 ) ;
#14741 = CARTESIAN_POINT ( 'NONE',  ( -259.2033419157646676, 49.83842185052027673, -6.730120644403441155 ) ) ;
#14742 = CARTESIAN_POINT ( 'NONE',  ( -190.6721700386038378, -13.94344193548887567, -47.76494742512097247 ) ) ;
#14743 = ADVANCED_FACE ( 'NONE', ( #20141 ), #24938, .T. ) ;
#14744 = CARTESIAN_POINT ( 'NONE',  ( -30.26275506840323359, -1.198031551616339341, 57.76657404653985139 ) ) ;
#14745 = CARTESIAN_POINT ( 'NONE',  ( -3.696864809816581943, -43.10456217110744603, -23.52297716615256817 ) ) ;
#14746 = ORIENTED_EDGE ( 'NONE', *, *, #16385, .T. ) ;
#14747 = CARTESIAN_POINT ( 'NONE',  ( -190.0000000000000000, 52.49999999999987210, 82.49999999999998579 ) ) ;
#14748 = CARTESIAN_POINT ( 'NONE',  ( 200.0000000000000853, 11.56430744387933274, -15.08818561847743922 ) ) ;
#14749 = CARTESIAN_POINT ( 'NONE',  ( -626.9846540392142060, 90.00000000000000000, 0.000000000000000000 ) ) ;
#14750 = CARTESIAN_POINT ( 'NONE',  ( 19.06497207195980792, 54.19242893257844429, 40.00000000000002132 ) ) ;
#14751 = CARTESIAN_POINT ( 'NONE',  ( 151.7948205124836250, -23.49921654116371883, 23.49921654116317526 ) ) ;
#14752 = CARTESIAN_POINT ( 'NONE',  ( 199.0156213727907186, 14.58859942632390094, 13.68185500382998576 ) ) ;
#14753 = EDGE_CURVE ( 'NONE', #15843, #61, #5654, .T. ) ;
#14754 = CARTESIAN_POINT ( 'NONE',  ( 200.0000000000000000, -42.42640687119290988, 14.14213562373064903 ) ) ;
#14755 = CARTESIAN_POINT ( 'NONE',  ( 4.995406935893305089, -40.00000000000021316, 55.24977328853194791 ) ) ;
#14756 = CARTESIAN_POINT ( 'NONE',  ( 4.995406935893283773, 39.99999999999997158, 15.24977328854846803 ) ) ;
#14757 = CARTESIAN_POINT ( 'NONE',  ( -3.071327051952984721, 47.32824404903822568, -13.87830843099591505 ) ) ;
#14758 = CARTESIAN_POINT ( 'NONE',  ( 57.59792236341147031, 2.435789363418170872, -40.00000000000002132 ) ) ;
#14759 = DIRECTION ( 'NONE',  ( 0.000000000000000000, 0.000000000000000000, 1.000000000000000000 ) ) ;
#14760 = CARTESIAN_POINT ( 'NONE',  ( -238.4067589809705510, -40.96449427998265946, -2.449293598294708485E-15 ) ) ;
#14761 = ADVANCED_FACE ( 'NONE', ( #13974, #11985, #20108 ), #18226, .T. ) ;
#14762 = CARTESIAN_POINT ( 'NONE',  ( -135.8532207217289738, -21.81201906317788186, 21.81201906317762962 ) ) ;
#14763 = CARTESIAN_POINT ( 'NONE',  ( 151.0853911467767432, -12.04115959307973505, -29.06993079631223154 ) ) ;
#14764 = CARTESIAN_POINT ( 'NONE',  ( -110.0368417077420418, 18.51665893310598676, -7.992411109433959382 ) ) ;
#14765 = CARTESIAN_POINT ( 'NONE',  ( -105.3755690713226585, 40.00000000000019185, -18.24025645688310249 ) ) ;
#14766 = CARTESIAN_POINT ( 'NONE',  ( -100.7734535825088500, 39.99999999999994316, 17.32597176626825686 ) ) ;
#14767 = CARTESIAN_POINT ( 'NONE',  ( -192.9588430854689989, 10.23066800230742679, 10.23066800230749607 ) ) ;
#14768 = DIRECTION ( 'NONE',  ( 0.9698969544100306539, 0.2249791742633133473, -0.09318942522595978495 ) ) ;
#14769 = CARTESIAN_POINT ( 'NONE',  ( -114.6318783467470723, -11.20407312246388720, 18.94416332742964926 ) ) ;
#14770 = CARTESIAN_POINT ( 'NONE',  ( 19.06497207195982568, -38.31983398719646061, 38.31983398719606271 ) ) ;
#14771 = ORIENTED_EDGE ( 'NONE', *, *, #18178, .T. ) ;
#14773 = CARTESIAN_POINT ( 'NONE',  ( 199.9999999999999432, -14.14213562373115884, 14.14213562373085153 ) ) ;
#14772 = CARTESIAN_POINT ( 'NONE',  ( 163.1118516004056573, 19.27778845538753316, 19.27778845538783870 ) ) ;
#14774 = CARTESIAN_POINT ( 'NONE',  ( 147.2817042152898637, 29.82799917201328554, -12.35516179550128157 ) ) ;
#14775 = CARTESIAN_POINT ( 'NONE',  ( -280.0000000000000568, -20.00000000000006395, -40.00000000000002132 ) ) ;
#14776 = EDGE_CURVE ( 'NONE', #8230, #24877, #18678, .T. ) ;
#14777 = CARTESIAN_POINT ( 'NONE',  ( -86.91014751117381820, -7.317915707774015566, -20.05881702300846925 ) ) ;
#14778 = CARTESIAN_POINT ( 'NONE',  ( 14.38125909742180752, 10.73282306404735387, -10.73282306404708919 ) ) ;
#14779 = EDGE_LOOP ( 'NONE', ( #22111, #20788, #22258, #11343, #5743, #19458, #20685 ) ) ;
#14780 = ORIENTED_EDGE ( 'NONE', *, *, #21855, .F. ) ;
#14781 = CARTESIAN_POINT ( 'NONE',  ( -190.0000000000000000, -66.50000000000001421, -66.50000000000005684 ) ) ;
#14782 = DIRECTION ( 'NONE',  ( 0.000000000000000000, 0.000000000000000000, -1.000000000000000000 ) ) ;
#14783 = CARTESIAN_POINT ( 'NONE',  ( 22.77497178454752458, 17.88345994150152762, 43.17449153292939457 ) ) ;
#14784 = ORIENTED_EDGE ( 'NONE', *, *, #13149, .F. ) ;
#14785 = VERTEX_POINT ( 'NONE', #14506 ) ;
#14786 = CARTESIAN_POINT ( 'NONE',  ( -100.7734535825088500, -16.03295912088716335, 40.53558337403673306 ) ) ;
#14787 = CARTESIAN_POINT ( 'NONE',  ( 199.0188446093723371, -17.48804260178791736, -9.712431339257729945 ) ) ;
#14788 = CARTESIAN_POINT ( 'NONE',  ( -105.2109270642729939, 1.359352815179485363, 21.45728911408426498 ) ) ;
#14789 = CARTESIAN_POINT ( 'NONE',  ( 19.06497207195981858, 10.03556273973424062, 66.60410523465820631 ) ) ;
#14790 = CARTESIAN_POINT ( 'NONE',  ( -105.4741150117382915, -19.60045294982753461, 8.366608964593266862 ) ) ;
#14791 = CARTESIAN_POINT ( 'NONE',  ( 192.4448373802101173, 39.99999999999998579, 19.99999999996075317 ) ) ;
#14792 = CARTESIAN_POINT ( 'NONE',  ( -210.0000000000000284, -61.50000000000001421, 66.50000000000005684 ) ) ;
#14793 = DIRECTION ( 'NONE',  ( 1.000000000000000000, 1.836970198721030181E-16, 0.000000000000000000 ) ) ;
#14794 = CARTESIAN_POINT ( 'NONE',  ( -259.2033419157646676, 40.00000000000029843, -30.48217210827696988 ) ) ;
#14795 = CARTESIAN_POINT ( 'NONE',  ( -100.7734535825088358, -2.560096224687585342E-13, 22.67402823373191723 ) ) ;
#14796 = CARTESIAN_POINT ( 'NONE',  ( -639.1748570899752622, 29.12792997464579869, 27.41590550727503839 ) ) ;
#14797 = CARTESIAN_POINT ( 'NONE',  ( -86.95492379317086318, -19.11844895728714988, -9.645497522856738115 ) ) ;
#14798 = CARTESIAN_POINT ( 'NONE',  ( 199.0128224874292471, 17.70345943908711561, 9.303337553156843853 ) ) ;
#14799 = CARTESIAN_POINT ( 'NONE',  ( -188.2870673237561050, 13.82722856953796864, 46.98612534495544679 ) ) ;
#14800 = CARTESIAN_POINT ( 'NONE',  ( -56.48582580120559982, -21.81201906317804173, 34.75652343174591152 ) ) ;
#14801 = CARTESIAN_POINT ( 'NONE',  ( -196.0240758340697198, -48.96019759410239658, 14.12332442061111237 ) ) ;
#14802 = CARTESIAN_POINT ( 'NONE',  ( 19.06497207195982568, -38.31983398719646061, 38.31983398719606271 ) ) ;
#14803 = DIRECTION ( 'NONE',  ( 0.000000000000000000, 1.000000000000000000, 0.000000000000000000 ) ) ;
#14804 = CARTESIAN_POINT ( 'NONE',  ( -100.7734535825088358, -12.25131212657475643, -12.25131212657495539 ) ) ;
#14805 = CARTESIAN_POINT ( 'NONE',  ( -639.6442031523718015, 30.97426854515512673, 32.64946120922897421 ) ) ;
#14806 = CARTESIAN_POINT ( 'NONE',  ( -83.21262154144250189, -33.12752917118400831, 13.72187187061544122 ) ) ;
#14807 = CARTESIAN_POINT ( 'NONE',  ( 57.59792236341147031, 26.56190807104652052, 30.00663442387728708 ) ) ;
#14808 = CARTESIAN_POINT ( 'NONE',  ( 192.4448373802101173, 20.00000000003945644, 40.00000000000002132 ) ) ;
#14809 = CARTESIAN_POINT ( 'NONE',  ( -575.0231298121466352, 90.00000000000000000, -25.00000000000201794 ) ) ;
#14810 = EDGE_LOOP ( 'NONE', ( #25077, #24549, #21812, #23929 ) ) ;
#14811 = CARTESIAN_POINT ( 'NONE',  ( -91.56559293963834989, -40.00000000000027711, 22.67402823373149801 ) ) ;
#14812 = CARTESIAN_POINT ( 'NONE',  ( 199.0084563976654977, 0.009091564791348882152, -19.99625984770770160 ) ) ;
#14813 = CARTESIAN_POINT ( 'NONE',  ( 164.1122551457365546, -10.10009781492445491, 24.38379312608483573 ) ) ;
#14814 = ORIENTED_EDGE ( 'NONE', *, *, #5708, .T. ) ;
#14815 = EDGE_LOOP ( 'NONE', ( #10395, #8001 ) ) ;
#14816 = CARTESIAN_POINT ( 'NONE',  ( 163.1118516004056573, 12.73709011382477918, 40.00000000000002132 ) ) ;
#14817 = AXIS2_PLACEMENT_3D ( 'NONE', #12941, #24928, #710 ) ;
#14818 = EDGE_CURVE ( 'NONE', #18174, #8800, #13063, .T. ) ;
#14819 = CARTESIAN_POINT ( 'NONE',  ( -114.6821015619773902, -21.58745106897183419, -4.467609313250024528 ) ) ;
#14820 = EDGE_CURVE ( 'NONE', #19333, #25051, #9808, .T. ) ;
#14821 = CARTESIAN_POINT ( 'NONE',  ( -200.0000000000000000, 55.16984130227019989, -4.865628651907604407 ) ) ;
#14822 = CARTESIAN_POINT ( 'NONE',  ( 14.38125909742181818, -40.00000000000007816, 15.17850393972619649 ) ) ;
#14823 = CARTESIAN_POINT ( 'NONE',  ( 199.9999999999998863, 12.98615309696526587, -13.88358464575571283 ) ) ;
#14824 = ADVANCED_FACE ( 'NONE', ( #6520, #25033, #6786, #4813, #6653, #2410 ), #680, .T. ) ;
#14825 = CARTESIAN_POINT ( 'NONE',  ( -105.2054292635175727, 7.329160573984922335E-13, -21.49321519473985020 ) ) ;
#14826 = CARTESIAN_POINT ( 'NONE',  ( -259.2033419157646676, -6.730120644403663199, 6.730120644403451813 ) ) ;
#14827 = CARTESIAN_POINT ( 'NONE',  ( -213.1075012329537230, -9.698598906450422774, -9.698598906450550672 ) ) ;
#14828 = CARTESIAN_POINT ( 'NONE',  ( -77.90255099906863734, -20.04994828524331396, -8.644468104250957907 ) ) ;
#14829 = CARTESIAN_POINT ( 'NONE',  ( 170.2234770963711128, -2.259079968736224833E-13, 24.55285855007187124 ) ) ;
#14830 = CARTESIAN_POINT ( 'NONE',  ( -100.0753760173601989, -8.149786832859113872, 20.72827493166387924 ) ) ;
#14831 = CARTESIAN_POINT ( 'NONE',  ( 23.37394308801976450, 13.80096434448266685, 46.80823611210199431 ) ) ;
#14832 = CARTESIAN_POINT ( 'NONE',  ( -213.1075012329537230, 37.98287015391228749, 37.98287015391245802 ) ) ;
#14833 = CARTESIAN_POINT ( 'NONE',  ( 151.7948205124836534, -33.06932595376343897, -23.49921654116042902 ) ) ;
#14834 = CARTESIAN_POINT ( 'NONE',  ( 199.0142575219002765, 16.25768778350697374, 11.67280966210075910 ) ) ;
#14836 = CARTESIAN_POINT ( 'NONE',  ( 57.59792236341147031, 1.908507979671054758E-14, -2.435789363418160658 ) ) ;
#14835 = CARTESIAN_POINT ( 'NONE',  ( -105.3755690713226727, -15.38646221621807619, 15.38646221621768362 ) ) ;
#14837 = CARTESIAN_POINT ( 'NONE',  ( 60.14720761588395703, 33.22245024480380238, -10.94158980388390923 ) ) ;
#14838 = CARTESIAN_POINT ( 'NONE',  ( 0.2972598230769930017, 14.33493731733933352, -40.00000000000002132 ) ) ;
#14839 = CARTESIAN_POINT ( 'NONE',  ( -30.26275506840324070, -27.08623969584595770, 29.48230279907789608 ) ) ;
#14840 = CARTESIAN_POINT ( 'NONE',  ( 170.2234770963711128, -24.55285855007184281, 40.00000000000002132 ) ) ;
#14841 = AXIS2_PLACEMENT_3D ( 'NONE', #10681, #573, #8678 ) ;
#14842 = VERTEX_POINT ( 'NONE', #21032 ) ;
#14843 = CARTESIAN_POINT ( 'NONE',  ( -2.557884977116120506, -47.52441970262191262, 13.90734923102589704 ) ) ;
#14844 = CARTESIAN_POINT ( 'NONE',  ( 19.06497207195980792, 14.19242893257840699, 40.00000000000002132 ) ) ;
#14845 = ORIENTED_EDGE ( 'NONE', *, *, #23306, .T. ) ;
#14846 = LINE ( 'NONE', #8867, #12802 ) ;
#14847 = FACE_OUTER_BOUND ( 'NONE', #2866, .T. ) ;
#14848 = CARTESIAN_POINT ( 'NONE',  ( -3.838270362644687239, -17.89317813950069436, 43.19795333834606765 ) ) ;
#14849 = CARTESIAN_POINT ( 'NONE',  ( -238.4067589809705794, 28.96627169325324758, -27.60227080167054581 ) ) ;
#14850 = CARTESIAN_POINT ( 'NONE',  ( -3.921555385249997805, 23.47492146734898810, -43.03974577853578154 ) ) ;
#14851 = CARTESIAN_POINT ( 'NONE',  ( 199.0263554293247523, -15.04073044714995611, 13.19117051905602089 ) ) ;
#14852 = CARTESIAN_POINT ( 'NONE',  ( 0.2972598230769938343, 10.13633138497486286, -10.13633138497461594 ) ) ;
#14853 = EDGE_CURVE ( 'NONE', #555, #19588, #14898, .T. ) ;
#14854 = CARTESIAN_POINT ( 'NONE',  ( -77.90255099906769942, -20.29001641120677846, -8.064892378658084837 ) ) ;
#14855 = DIRECTION ( 'NONE',  ( 0.000000000000000000, 1.000000000000000000, 0.000000000000000000 ) ) ;
#14856 = CARTESIAN_POINT ( 'NONE',  ( -188.3392995398617700, -13.83024151208848807, 47.00482667599631270 ) ) ;
#14857 = CARTESIAN_POINT ( 'NONE',  ( -91.56559293963836410, 16.03295912088692177, 16.03295912088721664 ) ) ;
#14858 = CIRCLE ( 'NONE', #19121, 14.99999999999999822 ) ;
#14859 = CARTESIAN_POINT ( 'NONE',  ( 4.995406935893301537, -10.78321810390187530, 67.35176059882529387 ) ) ;
#14860 = CARTESIAN_POINT ( 'NONE',  ( -30.26275506840324070, 1.198031551616030033, -1.198031551616006496 ) ) ;
#14861 = CARTESIAN_POINT ( 'NONE',  ( -213.1075012329537230, 18.58567234101174037, -37.98287015391222354 ) ) ;
#14863 = CARTESIAN_POINT ( 'NONE',  ( -105.3755690713226585, 41.18208027870575449, 15.38646221621837107 ) ) ;
#14862 = CARTESIAN_POINT ( 'NONE',  ( 14.38125909742181285, -10.73282306404712472, -10.73282306404731301 ) ) ;
#14864 = CARTESIAN_POINT ( 'NONE',  ( 151.7948205124836250, -23.49921654116371883, 23.49921654116317526 ) ) ;
#14865 = CARTESIAN_POINT ( 'NONE',  ( 151.7948205124835681, 33.23291073765556547, 40.00000000000002132 ) ) ;
#14866 = CARTESIAN_POINT ( 'NONE',  ( 136.1360204305621551, 4.966164525587093870, -40.00000000000002132 ) ) ;
#14867 = CARTESIAN_POINT ( 'NONE',  ( 4.995406935893283773, 39.06748935135195211, -17.50105314357185193 ) ) ;
#14868 = FACE_OUTER_BOUND ( 'NONE', #2280, .T. ) ;
#14869 = CARTESIAN_POINT ( 'NONE',  ( -198.0356074513804288, -39.15871834505882276, -39.15871834505946936 ) ) ;
#14870 = CARTESIAN_POINT ( 'NONE',  ( -184.9729924864769259, 45.83719276903030959, -13.59277144553964689 ) ) ;
#14871 = VERTEX_POINT ( 'NONE', #4677 ) ;
#14872 = CARTESIAN_POINT ( 'NONE',  ( -91.56559293963834989, -16.03295912088716335, 40.53558337403673306 ) ) ;
#14873 = CARTESIAN_POINT ( 'NONE',  ( -82.23726319249649919, -14.28014421912411080, -14.28014421912425114 ) ) ;
#14874 = CARTESIAN_POINT ( 'NONE',  ( -208.1127848780264742, -38.89260858015758515, 38.89260858015713751 ) ) ;
#14875 = CARTESIAN_POINT ( 'NONE',  ( -4.031723327955770486, -43.00750292060831725, -23.45082932595563818 ) ) ;
#14876 = ORIENTED_EDGE ( 'NONE', *, *, #14186, .F. ) ;
#14877 = CARTESIAN_POINT ( 'NONE',  ( -726.9846540392142060, -82.49999999999991473, -52.49999999999977973 ) ) ;
#14878 = CARTESIAN_POINT ( 'NONE',  ( -105.2054292635175869, -15.19799821370180126, -15.19799821370278892 ) ) ;
#14879 = VECTOR ( 'NONE', #2030, 1000.000000000000000 ) ;
#14880 = CARTESIAN_POINT ( 'NONE',  ( 199.9999999999997726, 7.546454185142647653, -17.43816512261951956 ) ) ;
#14881 = CARTESIAN_POINT ( 'NONE',  ( 7.307793755307390171, 14.18010697691907929, -49.33439594495632008 ) ) ;
#14882 = CARTESIAN_POINT ( 'NONE',  ( 170.2234770963711128, 15.44714144992818738, 40.00000000000002132 ) ) ;
#14883 = CARTESIAN_POINT ( 'NONE',  ( 170.2234770963711128, -17.36149277827010096, 17.36149277826970660 ) ) ;
#14884 = CARTESIAN_POINT ( 'NONE',  ( 199.0193391886810446, 8.833261569310058903, 17.94623560139499574 ) ) ;
#14885 = CARTESIAN_POINT ( 'NONE',  ( 146.6084372240433709, -3.800685668859084210, 52.76785682606516303 ) ) ;
#14886 = CARTESIAN_POINT ( 'NONE',  ( 200.0000000000000000, -40.00000000000005684, 19.99999999999978328 ) ) ;
#14887 = CARTESIAN_POINT ( 'NONE',  ( -162.0762913951020892, 39.99999999999985079, 41.69427287692695216 ) ) ;
#14888 = CARTESIAN_POINT ( 'NONE',  ( -198.0012279766649783, -24.77357825137635317, -44.79720171007490848 ) ) ;
#14889 = CARTESIAN_POINT ( 'NONE',  ( -192.9588430854690273, -54.46834944101725284, -40.00000000000002132 ) ) ;
#14891 = CARTESIAN_POINT ( 'NONE',  ( 0.2972598230769976091, -10.13633138497479180, 10.13633138497468522 ) ) ;
#14890 = CARTESIAN_POINT ( 'NONE',  ( 22.77497178454834881, -17.88345994150125051, -43.17449153292930220 ) ) ;
#14892 = CARTESIAN_POINT ( 'NONE',  ( 170.2234770963711128, -15.44714144992812876, -2.449293598294708485E-15 ) ) ;
#14893 = CARTESIAN_POINT ( 'NONE',  ( 151.7948205124835681, 51.78348778862537927, 4.785054706298732086 ) ) ;
#14894 = CARTESIAN_POINT ( 'NONE',  ( 155.4809970915716804, -11.45899766888342164, -27.66446758342039658 ) ) ;
#14895 = CARTESIAN_POINT ( 'NONE',  ( -114.6297772182939951, 11.19545617573264451, -18.93772329698290235 ) ) ;
#14896 = CARTESIAN_POINT ( 'NONE',  ( 146.6084372240433709, 40.00000000000010658, -5.374981219216549810 ) ) ;
#14897 = CARTESIAN_POINT ( 'NONE',  ( -30.26275506840324070, 1.198031551616013601, 1.198031551616023371 ) ) ;
#14898 = LINE ( 'NONE', #4288, #4140 ) ;
#14899 = CARTESIAN_POINT ( 'NONE',  ( 180.0000000000000000, -71.50000000000002842, -66.50000000000005684 ) ) ;
#14900 = CARTESIAN_POINT ( 'NONE',  ( -105.3755690713226727, -12.89780903124413847, 12.89780903124398037 ) ) ;
#14901 = ORIENTED_EDGE ( 'NONE', *, *, #7653, .F. ) ;
#14903 = CARTESIAN_POINT ( 'NONE',  ( -47.65341557548335061, 31.50022537338118767, -10.55973086711139786 ) ) ;
#14902 = DIRECTION ( 'NONE',  ( 0.000000000000000000, -0.6739498806388345420, -0.7387770694782699321 ) ) ;
#14904 = DIRECTION ( 'NONE',  ( -1.000000000000000000, 0.000000000000000000, 0.000000000000000000 ) ) ;
#14905 = CARTESIAN_POINT ( 'NONE',  ( -100.7734535825088358, -17.32597176626813251, -2.449293598294708485E-15 ) ) ;
#14906 = CARTESIAN_POINT ( 'NONE',  ( -163.5815475691942709, -35.61501186087241422, 18.59457173339187364 ) ) ;
#14907 = DIRECTION ( 'NONE',  ( 0.000000000000000000, 0.000000000000000000, 1.000000000000000000 ) ) ;
#14908 = ORIENTED_EDGE ( 'NONE', *, *, #24102, .T. ) ;
#14909 = VERTEX_POINT ( 'NONE', #23038 ) ;
#14910 = CARTESIAN_POINT ( 'NONE',  ( 200.0000000000000000, -11.58160531504706547, 15.07837909557420275 ) ) ;
#14911 = CARTESIAN_POINT ( 'NONE',  ( -210.0000000000000284, 71.50000000000011369, -66.50000000000005684 ) ) ;
#14912 = VERTEX_POINT ( 'NONE', #18901 ) ;
#14913 = ORIENTED_EDGE ( 'NONE', *, *, #16396, .F. ) ;
#14914 = PRODUCT_DEFINITION ( 'UNKNOWN', '', #7447, #23345 ) ;
#14915 = CARTESIAN_POINT ( 'NONE',  ( -238.4067589809705794, -27.60227080167069147, 28.96627169325319429 ) ) ;
#14916 = CARTESIAN_POINT ( 'NONE',  ( 199.0230409161751197, -19.98726064469808961, -0.8218112272605428981 ) ) ;
#14917 = AXIS2_PLACEMENT_3D ( 'NONE', #9398, #17628, #5535 ) ;
#14918 = CARTESIAN_POINT ( 'NONE',  ( -105.3174603216987890, -18.50736914802315880, -10.86220755232618096 ) ) ;
#14919 = CARTESIAN_POINT ( 'NONE',  ( -238.4067589809705794, -27.60227080167069147, 28.96627169325319429 ) ) ;
#14920 = VECTOR ( 'NONE', #15065, 1000.000000000000000 ) ;
#14921 = CARTESIAN_POINT ( 'NONE',  ( -362.0709805440841365, -4.857225732735059864E-14, 9.999999999999998224 ) ) ;
#14922 = CARTESIAN_POINT ( 'NONE',  ( -91.56559293963836410, 39.99999999999994316, 17.32597176626825330 ) ) ;
#14923 = CIRCLE ( 'NONE', #3442, 5.000000000000004441 ) ;
#14924 = AXIS2_PLACEMENT_3D ( 'NONE', #9450, #19684, #21563 ) ;
#14925 = DIRECTION ( 'NONE',  ( 0.000000000000000000, 1.321694076934715579E-16, 1.000000000000000000 ) ) ;
#14926 = CARTESIAN_POINT ( 'NONE',  ( -88.37877758185183552, -8.026456973205808865, -20.15391234962195810 ) ) ;
#14927 = EDGE_CURVE ( 'NONE', #12388, #7311, #9219, .T. ) ;
#14928 = CARTESIAN_POINT ( 'NONE',  ( 91.82158438592159655, -40.00000000000017764, 17.20528682183258340 ) ) ;
#14929 = CARTESIAN_POINT ( 'NONE',  ( 0.2972598230769883387, 40.00000000000017053, -14.33493731733891607 ) ) ;
#14930 = CARTESIAN_POINT ( 'NONE',  ( -210.0000000000000284, 69.29737539576900929, -75.30386416458597409 ) ) ;
#14931 = CARTESIAN_POINT ( 'NONE',  ( 200.0000000000000000, 66.50000000000009948, -66.50000000000005684 ) ) ;
#14932 = CARTESIAN_POINT ( 'NONE',  ( 199.0120816426991155, 18.34336195414084969, 7.966874786652939910 ) ) ;
#14933 = CARTESIAN_POINT ( 'NONE',  ( -188.4701769959665967, 13.83721050406949793, 47.05181236278358625 ) ) ;
#14934 = B_SPLINE_CURVE_WITH_KNOTS ( 'NONE', 3,
 ( #18256, #14404, #2435, #10284, #8276, #16401 ),
 .UNSPECIFIED., .F., .F.,
 ( 4, 2, 4 ),
 ( -6.000000002263262234E-08, 0.03937727647057992497, 0.07875461294115987387 ),
 .UNSPECIFIED. ) ;
#14935 = CARTESIAN_POINT ( 'NONE',  ( -105.3755690713226727, 15.38646221621771737, 15.38646221621800514 ) ) ;
#14936 = DIRECTION ( 'NONE',  ( 0.000000000000000000, 1.000000000000000000, 0.000000000000000000 ) ) ;
#14937 = CARTESIAN_POINT ( 'NONE',  ( -105.3755690713226585, 43.67073346367970288, 12.89780903124427702 ) ) ;
#14938 = CARTESIAN_POINT ( 'NONE',  ( -77.90255099906768521, -20.04994828523974348, 8.644468104261179064 ) ) ;
#14939 = AXIS2_PLACEMENT_3D ( 'NONE', #4657, #531, #4529 ) ;
#14940 = CARTESIAN_POINT ( 'NONE',  ( -259.2033419157646676, 6.730120644403918995, -49.83842185052024831 ) ) ;
#14941 = CARTESIAN_POINT ( 'NONE',  ( -645.5937089524366002, 33.84884618228691977, 29.66287758167644384 ) ) ;
#14942 = CARTESIAN_POINT ( 'NONE',  ( -199.9999999999997726, -24.82633483071077762, 44.86878812508861358 ) ) ;
#14943 = CARTESIAN_POINT ( 'NONE',  ( 151.7948205124836250, -23.49921654116371883, 23.49921654116317526 ) ) ;
#14944 = B_SPLINE_CURVE_WITH_KNOTS ( 'NONE', 3,
 ( #25012, #20610, #6765, #12894, #24744, #16346, #22482, #2661, #22615, #24478, #4261, #10766 ),
 .UNSPECIFIED., .F., .F.,
 ( 4, 2, 2, 2, 2, 4 ),
 ( 2.733202585622216256E-15, 0.004698945756009177514, 0.007048418634012399743, 0.009397891512015622839, 0.01409683726802202566, 0.01879578302402842849 ),
 .UNSPECIFIED. ) ;
#14945 = CARTESIAN_POINT ( 'NONE',  ( 163.1118516004056573, -12.73709011382472589, 40.00000000000002132 ) ) ;
#14946 = CARTESIAN_POINT ( 'NONE',  ( -600.8818656075578701, 38.48738506407975990, 23.32272707864667183 ) ) ;
#14947 = ORIENTED_EDGE ( 'NONE', *, *, #23589, .T. ) ;
#14948 = CARTESIAN_POINT ( 'NONE',  ( 151.7948205124836250, 1.012150473917908975E-13, -6.767089262349031742 ) ) ;
#14949 = CARTESIAN_POINT ( 'NONE',  ( 199.9999999999999432, -14.14213562373096345, -14.14213562373104871 ) ) ;
#14950 = CARTESIAN_POINT ( 'NONE',  ( 104.1600437297060608, -8.548029201781588426, 20.63676802900535634 ) ) ;
#14951 = ORIENTED_EDGE ( 'NONE', *, *, #6156, .F. ) ;
#14952 = EDGE_LOOP ( 'NONE', ( #18466, #15081, #4390, #13987 ) ) ;
#14953 = ORIENTED_EDGE ( 'NONE', *, *, #25263, .T. ) ;
#14954 = CARTESIAN_POINT ( 'NONE',  ( 170.2234770963711128, 15.44714144992818738, 40.00000000000002132 ) ) ;
#14955 = CARTESIAN_POINT ( 'NONE',  ( 170.0000000000000000, 30.00000000000007105, 0.000000000000000000 ) ) ;
#14956 = AXIS2_PLACEMENT_3D ( 'NONE', #21936, #11419, #25940 ) ;
#14957 = B_SPLINE_CURVE_WITH_KNOTS ( 'NONE', 3,
 ( #25023, #2399, #13038, #6776, #14888, #18758 ),
 .UNSPECIFIED., .F., .F.,
 ( 4, 2, 4 ),
 ( -5.998616620282925083E-08, 0.005995031700373402127, 0.01199012338691300694 ),
 .UNSPECIFIED. ) ;
#14958 = CARTESIAN_POINT ( 'NONE',  ( -114.6659165474202524, -21.50057250525921759, -4.804252803513915815 ) ) ;
#14959 = CARTESIAN_POINT ( 'NONE',  ( -200.0000000000000000, 53.44529986889376261, -10.02640517461949088 ) ) ;
#14960 = CARTESIAN_POINT ( 'NONE',  ( 0.2972598230769957217, -4.999556039334937811E-14, 14.33493731733933352 ) ) ;
#14961 = CARTESIAN_POINT ( 'NONE',  ( 200.0000000000002842, 4.912815075579886503, -18.35721014059308942 ) ) ;
#14962 = CARTESIAN_POINT ( 'NONE',  ( 199.9999999999999147, -4.322471944100380270, -18.50700405022334394 ) ) ;
#14963 = CARTESIAN_POINT ( 'NONE',  ( -208.1127848780264742, 10.60833733268383483, -67.17687982760675425 ) ) ;
#14964 = CARTESIAN_POINT ( 'NONE',  ( -213.1075012329537230, -9.698598906450422774, -9.698598906450550672 ) ) ;
#14965 = CARTESIAN_POINT ( 'NONE',  ( -102.4332189563017153, 20.29361511516604466, 8.405890610281785413 ) ) ;
#14966 = CARTESIAN_POINT ( 'NONE',  ( 192.4448373802101173, 40.00000000000026290, -19.99999999996018474 ) ) ;
#14967 = CARTESIAN_POINT ( 'NONE',  ( 4.995406935893293543, -10.78321810388990265, -10.78321810389009272 ) ) ;
#14968 = CARTESIAN_POINT ( 'NONE',  ( -3.486753633152349874, 13.85715877881432334, 47.18604396268653289 ) ) ;
#14969 = CARTESIAN_POINT ( 'NONE',  ( -91.56559293963834989, -12.25131212657492874, 12.25131212657477953 ) ) ;
#14970 = CARTESIAN_POINT ( 'NONE',  ( 199.0084341825046579, 19.99614386575786895, -0.06800903924364970488 ) ) ;
#14972 = CARTESIAN_POINT ( 'NONE',  ( -56.48582580120559271, 2.158176344243877536E-14, -9.153146818113587102 ) ) ;
#14971 = CARTESIAN_POINT ( 'NONE',  ( 14.38125909742180752, 10.73282306404735387, -10.73282306404708919 ) ) ;
#14973 = CIRCLE ( 'NONE', #21762, 5.000000000000004441 ) ;
#14974 = DIRECTION ( 'NONE',  ( 0.000000000000000000, 1.000000000000000000, 0.000000000000000000 ) ) ;
#14975 = CARTESIAN_POINT ( 'NONE',  ( 4.995406935893294431, -17.50105314357198694, 39.06748935135188816 ) ) ;
#14976 = CARTESIAN_POINT ( 'NONE',  ( -105.3755690713226585, -21.75974354311652448, 40.00000000000002132 ) ) ;
#14977 = EDGE_LOOP ( 'NONE', ( #24317, #16487, #2197, #9862 ) ) ;
#14978 = CARTESIAN_POINT ( 'NONE',  ( 6.762329110759959683, -44.82519229649959414, 18.56720258519549915 ) ) ;
#14979 = CARTESIAN_POINT ( 'NONE',  ( -91.56559293963834989, -22.67402823373193499, -40.00000000000002132 ) ) ;
#14980 = CARTESIAN_POINT ( 'NONE',  ( -105.3841681040940443, 19.11869201643232330, -9.644852623852500528 ) ) ;
#14981 = CARTESIAN_POINT ( 'NONE',  ( 146.6084372240433709, -24.48358557860329299, 32.08495691632052882 ) ) ;
#14982 = CARTESIAN_POINT ( 'NONE',  ( -7.297127544299105928, -22.81351773423399010, 42.04314499754483592 ) ) ;
#14983 = CARTESIAN_POINT ( 'NONE',  ( -87.00234866557609337, 20.64508794607625930, -5.655436908802629503 ) ) ;
#14984 = CARTESIAN_POINT ( 'NONE',  ( -39.81953879993383794, 11.17638696932933584, -34.34246706536494287 ) ) ;
#14985 = CARTESIAN_POINT ( 'NONE',  ( 199.0263429660336385, -15.25543418246514982, 12.94225785457335753 ) ) ;
#14986 = CARTESIAN_POINT ( 'NONE',  ( 163.1118516004056573, -19.27778845538787422, 19.27778845538743724 ) ) ;
#14987 = CARTESIAN_POINT ( 'NONE',  ( -678.9461782662772293, 90.00000000000000000, 25.00000000000157385 ) ) ;
#14988 = FACE_OUTER_BOUND ( 'NONE', #20214, .T. ) ;
#14989 = CARTESIAN_POINT ( 'NONE',  ( -192.1964066538514544, -24.16259023442852083, 43.96877160662082673 ) ) ;
#14990 = CARTESIAN_POINT ( 'NONE',  ( -192.9588430854690273, 18.05360324515473280, -38.51493924976924177 ) ) ;
#14991 = CARTESIAN_POINT ( 'NONE',  ( -162.0762913951021176, 27.08623940707598265, 29.48230308784781428 ) ) ;
#14992 = CARTESIAN_POINT ( 'NONE',  ( 184.8905102610680444, -43.07788698682556827, -13.49065550809859104 ) ) ;
#14993 = CARTESIAN_POINT ( 'NONE',  ( -86.96347745069645896, 43.67073346367988762, -12.89780903124366418 ) ) ;
#14995 = CARTESIAN_POINT ( 'NONE',  ( -30.26275506840323715, 29.48230279907829754, -29.48230279907758344 ) ) ;
#14994 = CARTESIAN_POINT ( 'NONE',  ( -86.96347745069645896, 43.67073346367988762, -12.89780903124366418 ) ) ;
#14996 = CARTESIAN_POINT ( 'NONE',  ( -213.1075012329537230, 37.98287015391280619, -37.98287015391192512 ) ) ;
#14997 = CARTESIAN_POINT ( 'NONE',  ( -192.9588430854689989, 14.46834944099965981, 0.000000000000000000 ) ) ;
#14998 = CARTESIAN_POINT ( 'NONE',  ( 57.59792236341147031, -1.722363176415032004, -1.722363176415048880 ) ) ;
#14999 = EDGE_CURVE ( 'NONE', #21146, #15984, #21952, .T. ) ;
#15000 = CARTESIAN_POINT ( 'NONE',  ( -575.0231298121445889, 75.00000000000000000, 34.99999999999821654 ) ) ;
#15001 = B_SPLINE_CURVE_WITH_KNOTS ( 'NONE', 3,
 ( #3476, #21326, #23692, #21444, #3219, #13324, #1098, #11325, #13082, #19441, #13204, #1228, #5220, #9333, #17442, #25836, #21571, #11574, #19315, #2969, #19568, #3344, #9208, #17564, #25580, #1359, #7580, #9458, #7326, #15440, #5470, #15567, #3098, #25702 ),
 .UNSPECIFIED., .F., .F.,
 ( 4, 2, 2, 2, 2, 2, 2, 2, 2, 2, 2, 2, 2, 2, 2, 2, 4 ),
 ( -5.298243351200284084E-05, 0.01887868273877495867, 0.02834451532491844006, 0.03071097347145433296, 0.03307743161799021892, 0.03544388976452611528, 0.03781034791106200471, 0.04254326420413379051, 0.04727618049720556243, 0.04964263864374145879, 0.05200909679027735516, 0.05674201308334905769, 0.05910847122988491242, 0.06029170030315288142, 0.06147492937642085042, 0.06620784566949271255, 0.07567367825563642292 ),
 .UNSPECIFIED. ) ;
#15002 = CARTESIAN_POINT ( 'NONE',  ( 91.82158438592156813, -16.11829626348459144, 40.45024623143943643 ) ) ;
#15003 = EDGE_CURVE ( 'NONE', #4168, #8967, #4549, .T. ) ;
#15004 = CARTESIAN_POINT ( 'NONE',  ( -151.4802849339473028, 33.96623543943421453, -11.09498666339088224 ) ) ;
#15005 = VERTEX_POINT ( 'NONE', #20906 ) ;
#15006 = CARTESIAN_POINT ( 'NONE',  ( 184.8905102610680444, -14.79361573936389540, 41.77492675555996016 ) ) ;
#15007 = CARTESIAN_POINT ( 'NONE',  ( -86.86493150571121191, -19.77569912839188149, -7.943527260495856446 ) ) ;
#15008 = CARTESIAN_POINT ( 'NONE',  ( -56.48582580120558561, 6.472252184283903809, 50.09629031063968796 ) ) ;
#15009 = DIRECTION ( 'NONE',  ( 1.000000000000000000, 1.836970198721030427E-16, -0.000000000000000000 ) ) ;
#15010 = EDGE_CURVE ( 'NONE', #21905, #9342, #12377, .T. ) ;
#15011 = EDGE_CURVE ( 'NONE', #19936, #17205, #2277, .T. ) ;
#15012 = ORIENTED_EDGE ( 'NONE', *, *, #19065, .F. ) ;
#15013 = DIRECTION ( 'NONE',  ( 0.000000000000000000, -1.000000000000000000, 0.000000000000000000 ) ) ;
#15014 = CARTESIAN_POINT ( 'NONE',  ( -105.2272268089240157, -13.17799186901662445, -17.01573394474107204 ) ) ;
#15015 = CARTESIAN_POINT ( 'NONE',  ( 199.9999999999998579, 18.35745069958362308, -4.904641354906189576 ) ) ;
#15016 = DIRECTION ( 'NONE',  ( 0.000000000000000000, -1.000000000000000000, 0.000000000000000000 ) ) ;
#15017 = CARTESIAN_POINT ( 'NONE',  ( -56.48582580120559982, 30.84685318188643421, 40.00000000000002132 ) ) ;
#15018 = CARTESIAN_POINT ( 'NONE',  ( 83.11963132829231427, 10.90660717629898180, -23.63628489317784798 ) ) ;
#15019 = CARTESIAN_POINT ( 'NONE',  ( 199.0166590359707754, 13.17187519532568984, 15.05399639075651130 ) ) ;
#15020 = CARTESIAN_POINT ( 'NONE',  ( -213.1075012329537230, -9.698598906450422774, -9.698598906450550672 ) ) ;
#15021 = CARTESIAN_POINT ( 'NONE',  ( -135.8532207217289738, 39.99999999999989342, 30.84685318188660474 ) ) ;
#15022 = CARTESIAN_POINT ( 'NONE',  ( -238.4067589809705794, 39.99999999999997158, 0.9644942799827220803 ) ) ;
#15023 = DIRECTION ( 'NONE',  ( 0.000000000000000000, -1.000000000000000000, 0.000000000000000000 ) ) ;
#15024 = CARTESIAN_POINT ( 'NONE',  ( 4.995406935893294431, -15.24977328854832415, -40.00000000000002132 ) ) ;
#15026 = CARTESIAN_POINT ( 'NONE',  ( -608.6974641285738699, 32.13523715135190884, 23.85639593633560196 ) ) ;
#15025 = CARTESIAN_POINT ( 'NONE',  ( 25.62979979008176556, -13.63460241475589285, -45.99287499156992709 ) ) ;
#15027 = CARTESIAN_POINT ( 'NONE',  ( -213.1075012329537230, -13.71589010951915810, 0.000000000000000000 ) ) ;
#15028 = CARTESIAN_POINT ( 'NONE',  ( 170.2234770963711128, 45.64576402573181468, 10.92277846919223627 ) ) ;
#15029 = CARTESIAN_POINT ( 'NONE',  ( -259.2033419157646676, 39.99999999999987921, 9.517827891723049660 ) ) ;
#15030 = CARTESIAN_POINT ( 'NONE',  ( -110.0737093975827321, 17.41451009901375002, -10.28294049092901297 ) ) ;
#15031 = CARTESIAN_POINT ( 'NONE',  ( 19.06497207195982924, -39.99999999999945288, -54.19242893257885640 ) ) ;
#15032 = CARTESIAN_POINT ( 'NONE',  ( 14.38125909742180752, 10.73282306404720465, 10.73282306404724018 ) ) ;
#15033 = CARTESIAN_POINT ( 'NONE',  ( -4.039451493210483690, -43.00522595894025812, 23.44932283416647323 ) ) ;
#15034 = CARTESIAN_POINT ( 'NONE',  ( -198.0356074513804572, 39.15871834505887250, 17.40982414986519089 ) ) ;
#15035 = CARTESIAN_POINT ( 'NONE',  ( -238.4067589809705794, -0.6820004458488042598, 57.25054294077229855 ) ) ;
#15036 = EDGE_LOOP ( 'NONE', ( #21580, #22914, #7147, #10361 ) ) ;
#15038 = CARTESIAN_POINT ( 'NONE',  ( -5.304449574949627433, 42.80137191221132298, -17.72890873421417623 ) ) ;
#15037 = CARTESIAN_POINT ( 'NONE',  ( 136.1360204305621266, 24.77266263493104148, 24.77266263493145004 ) ) ;
#15039 = CARTESIAN_POINT ( 'NONE',  ( 155.4809970915716519, 27.66446758342043566, -11.45899766888336124 ) ) ;
#15040 = CARTESIAN_POINT ( 'NONE',  ( 170.2234770963711128, -15.44714144992813409, 40.00000000000002132 ) ) ;
#15041 = CARTESIAN_POINT ( 'NONE',  ( -114.7469200037858172, 17.46524160228967304, -13.55861222481908612 ) ) ;
#15042 = CARTESIAN_POINT ( 'NONE',  ( -194.4222775679850770, 44.35790405182663676, -24.44979664543170372 ) ) ;
#15043 = ORIENTED_EDGE ( 'NONE', *, *, #22501, .F. ) ;
#15044 = ORIENTED_EDGE ( 'NONE', *, *, #19387, .T. ) ;
#15045 = CARTESIAN_POINT ( 'NONE',  ( 199.9999999999999716, 1.537950039062797591, 18.94885247980957743 ) ) ;
#15046 = CARTESIAN_POINT ( 'NONE',  ( 98.29820294272414571, 7.653668647302724004, 18.47759065022804137 ) ) ;
#15047 = ORIENTED_EDGE ( 'NONE', *, *, #7657, .F. ) ;
#15048 = ORIENTED_EDGE ( 'NONE', *, *, #4106, .T. ) ;
#15049 =( BOUNDED_SURFACE ( )  B_SPLINE_SURFACE ( 3, 3, ( 
 ( #6329, #7683, #2349, #10462, #23791, #11814, #1717, #354, #23921, #17930, #8458, #24708, #6463, #22707, #19669, #9556, #13678, #9116, #6727, #20714, #22972, #15101, #11119, #6857, #756, #12856, #16845, #5012, #18707, #18843 ),
 ( #490, #8727, #24839, #19104, #1013, #19233, #23236, #16707, #2480, #10592, #12585, #8597, #4750, #8860, #14839, #6590, #14975, #23362, #17227, #20974, #21108, #10732, #7121, #3012, #12715, #25367, #2755, #2887, #621, #24978 ),
 ( #25234, #888, #12986, #13117, #6986, #23109, #10858, #14712, #22844, #15231, #4619, #20843, #8997, #2618, #17101, #18977, #16972, #10995, #25108, #4881, #21238, #19482, #17481, #9767, #5261, #5387, #17868, #11485, #13244, #7621 ),
 ( #17357, #15867, #26018, #3650, #7242, #19740, #21486, #1528, #3137, #1147, #3518, #9251, #17605, #11618, #9372, #25623, #7755, #7369, #9500, #15481, #3260, #23862, #11756, #5139, #25748, #1399, #19613, #13492, #7496, #23608 ),
 ( #25877, #19876, #21613, #5640, #13746, #11239, #25493, #21369, #15607, #15363, #23731, #3387, #21872, #19357, #5512, #13614, #23486, #9634, #21743, #17736, #15736, #1658, #13363, #11364, #1268, #8427, #12161, #3929, #4197, #6174 ),
 ( #26289, #16418, #14020, #16012, #10426, #24279, #12027, #12290, #10303, #3787, #20549, #20283, #18409, #9899, #57, #22421, #14419, #12420, #6301, #20418, #23995, #10168, #5776, #14153, #13883, #4059, #18003, #14284, #22549, #20147 ),
 ( #4330, #184, #1795, #22017, #11890, #20010, #26149, #16146, #2062, #8028, #7893, #18271, #24138, #2318, #6048, #2195, #22149, #18544, #326, #5911, #1925, #10032, #18141, #22285, #8167, #16280, #24408, #8291, #24546, #14949 ) ),
 .UNSPECIFIED., .T., .F., .F. ) 
 B_SPLINE_SURFACE_WITH_KNOTS ( ( 4, 3, 4 ),
 ( 4, 2, 2, 2, 2, 2, 2, 2, 2, 2, 2, 2, 2, 2, 4 ),
 ( 0.000000000000000000, 0.5000000000000000000, 1.000000000000000000 ),
 ( 0.000000000000000000, 0.1357259735107005372, 0.1651108541090157700, 0.1944957347073310028, 0.3598804999793158710, 0.3867117631979620773, 0.4135430264166082281, 0.5789277916885930964, 0.6062785021374117456, 0.6336292125862302838, 0.8508620842112317728, 0.8814014469398914198, 0.9119408096685510667, 0.9559704048342755334, 1.000000000000000000 ),
 .UNSPECIFIED. ) 
 GEOMETRIC_REPRESENTATION_ITEM ( )  RATIONAL_B_SPLINE_SURFACE ( (
 ( 1.000000000000000000, 1.000000000000000000, 1.000000000000000000, 1.000000000000000000, 1.000000000000000000, 1.000000000000000000, 1.000000000000000000, 1.000000000000000000, 1.000000000000000000, 1.000000000000000000, 1.000000000000000000, 1.000000000000000000, 1.000000000000000000, 1.000000000000000000, 1.000000000000000000, 1.000000000000000000, 1.000000000000000000, 1.000000000000000000, 1.000000000000000000, 1.000000000000000000, 1.000000000000000000, 1.000000000000000000, 1.000000000000000000, 1.000000000000000000, 1.000000000000000000, 1.000000000000000000, 1.000000000000000000, 1.000000000000000000, 1.000000000000000000, 1.000000000000000000),
 ( 0.3333333333333333703, 0.3333333333333333703, 0.3333333333333333703, 0.3333333333333333703, 0.3333333333333333703, 0.3333333333333333703, 0.3333333333333333703, 0.3333333333333333703, 0.3333333333333333703, 0.3333333333333333703, 0.3333333333333333703, 0.3333333333333333703, 0.3333333333333333703, 0.3333333333333333703, 0.3333333333333333703, 0.3333333333333333703, 0.3333333333333333703, 0.3333333333333333703, 0.3333333333333333703, 0.3333333333333333703, 0.3333333333333333703, 0.3333333333333333703, 0.3333333333333333703, 0.3333333333333333703, 0.3333333333333333703, 0.3333333333333333703, 0.3333333333333333703, 0.3333333333333333703, 0.3333333333333333703, 0.3333333333333333703),
 ( 0.3333333333333333703, 0.3333333333333333703, 0.3333333333333333703, 0.3333333333333333703, 0.3333333333333333703, 0.3333333333333333703, 0.3333333333333333703, 0.3333333333333333703, 0.3333333333333333703, 0.3333333333333333703, 0.3333333333333333703, 0.3333333333333333703, 0.3333333333333333703, 0.3333333333333333703, 0.3333333333333333703, 0.3333333333333333703, 0.3333333333333333703, 0.3333333333333333703, 0.3333333333333333703, 0.3333333333333333703, 0.3333333333333333703, 0.3333333333333333703, 0.3333333333333333703, 0.3333333333333333703, 0.3333333333333333703, 0.3333333333333333703, 0.3333333333333333703, 0.3333333333333333703, 0.3333333333333333703, 0.3333333333333333703),
 ( 1.000000000000000000, 1.000000000000000000, 1.000000000000000000, 1.000000000000000000, 1.000000000000000000, 1.000000000000000000, 1.000000000000000000, 1.000000000000000000, 1.000000000000000000, 1.000000000000000000, 1.000000000000000000, 1.000000000000000000, 1.000000000000000000, 1.000000000000000000, 1.000000000000000000, 1.000000000000000000, 1.000000000000000000, 1.000000000000000000, 1.000000000000000000, 1.000000000000000000, 1.000000000000000000, 1.000000000000000000, 1.000000000000000000, 1.000000000000000000, 1.000000000000000000, 1.000000000000000000, 1.000000000000000000, 1.000000000000000000, 1.000000000000000000, 1.000000000000000000),
 ( 0.3333333333333333703, 0.3333333333333333703, 0.3333333333333333703, 0.3333333333333333703, 0.3333333333333333703, 0.3333333333333333703, 0.3333333333333333703, 0.3333333333333333703, 0.3333333333333333703, 0.3333333333333333703, 0.3333333333333333703, 0.3333333333333333703, 0.3333333333333333703, 0.3333333333333333703, 0.3333333333333333703, 0.3333333333333333703, 0.3333333333333333703, 0.3333333333333333703, 0.3333333333333333703, 0.3333333333333333703, 0.3333333333333333703, 0.3333333333333333703, 0.3333333333333333703, 0.3333333333333333703, 0.3333333333333333703, 0.3333333333333333703, 0.3333333333333333703, 0.3333333333333333703, 0.3333333333333333703, 0.3333333333333333703),
 ( 0.3333333333333333703, 0.3333333333333333703, 0.3333333333333333703, 0.3333333333333333703, 0.3333333333333333703, 0.3333333333333333703, 0.3333333333333333703, 0.3333333333333333703, 0.3333333333333333703, 0.3333333333333333703, 0.3333333333333333703, 0.3333333333333333703, 0.3333333333333333703, 0.3333333333333333703, 0.3333333333333333703, 0.3333333333333333703, 0.3333333333333333703, 0.3333333333333333703, 0.3333333333333333703, 0.3333333333333333703, 0.3333333333333333703, 0.3333333333333333703, 0.3333333333333333703, 0.3333333333333333703, 0.3333333333333333703, 0.3333333333333333703, 0.3333333333333333703, 0.3333333333333333703, 0.3333333333333333703, 0.3333333333333333703),
 ( 1.000000000000000000, 1.000000000000000000, 1.000000000000000000, 1.000000000000000000, 1.000000000000000000, 1.000000000000000000, 1.000000000000000000, 1.000000000000000000, 1.000000000000000000, 1.000000000000000000, 1.000000000000000000, 1.000000000000000000, 1.000000000000000000, 1.000000000000000000, 1.000000000000000000, 1.000000000000000000, 1.000000000000000000, 1.000000000000000000, 1.000000000000000000, 1.000000000000000000, 1.000000000000000000, 1.000000000000000000, 1.000000000000000000, 1.000000000000000000, 1.000000000000000000, 1.000000000000000000, 1.000000000000000000, 1.000000000000000000, 1.000000000000000000, 1.000000000000000000) ) ) 
 REPRESENTATION_ITEM ( '' )  SURFACE ( )  );
#15050 = CARTESIAN_POINT ( 'NONE',  ( 130.8568914410475088, -52.36146031193419503, 4.207082182989537955 ) ) ;
#15051 = CARTESIAN_POINT ( 'NONE',  ( 199.0231033154536817, -19.99336494683761956, -0.6578043788800663760 ) ) ;
#15052 = CARTESIAN_POINT ( 'NONE',  ( -110.1017491837607594, -1.278135197250002353, 20.19444236855598973 ) ) ;
#15053 = CARTESIAN_POINT ( 'NONE',  ( -192.9588430854690273, -18.05360324515454096, 38.51493924976936967 ) ) ;
#15054 = CARTESIAN_POINT ( 'NONE',  ( 19.06497207195980792, 10.03556273973433299, 10.03556273973436319 ) ) ;
#15055 = CARTESIAN_POINT ( 'NONE',  ( 184.8905102610680444, -3.509827109981123710E-14, 19.07866798485558490 ) ) ;
#15056 = CARTESIAN_POINT ( 'NONE',  ( -199.9999999999999716, -14.87399974031237093, 48.57705986237296969 ) ) ;
#15057 = CARTESIAN_POINT ( 'NONE',  ( -86.86493150571116928, 19.60045294882758071, -8.366608963953975575 ) ) ;
#15058 = CARTESIAN_POINT ( 'NONE',  ( -280.0000000000000000, -2.609240458947769655E-13, 20.00000000000001421 ) ) ;
#15059 = CARTESIAN_POINT ( 'NONE',  ( -86.96347745069644475, 1.775309070576523494E-13, -18.24025645688352881 ) ) ;
#15060 = CARTESIAN_POINT ( 'NONE',  ( -105.4741150117382773, -19.60045294982755593, 8.366608964593277520 ) ) ;
#15061 = DIRECTION ( 'NONE',  ( 0.000000000000000000, 1.000000000000000000, 0.000000000000000000 ) ) ;
#15062 = CARTESIAN_POINT ( 'NONE',  ( 199.0054082256929746, 12.16974446990029790, -15.87805152391047159 ) ) ;
#15063 = CARTESIAN_POINT ( 'NONE',  ( -197.4154352059659630, 24.72550168627608258, 44.73190714600578843 ) ) ;
#15064 = CARTESIAN_POINT ( 'NONE',  ( -86.96347745069644475, 15.38646221621772092, 15.38646221621800336 ) ) ;
#15065 = DIRECTION ( 'NONE',  ( -1.303213150798907793E-16, 1.000000000000000000, -1.682156097916904081E-16 ) ) ;
#15066 = CARTESIAN_POINT ( 'NONE',  ( -86.96347745069644475, 15.38646221621793586, -15.38646221621778842 ) ) ;
#15067 = CARTESIAN_POINT ( 'NONE',  ( -77.65358652877148415, 21.60549460849031433, -4.394725072386959752 ) ) ;
#15068 = CARTESIAN_POINT ( 'NONE',  ( 184.8905102610680444, 14.79361573936424890, -41.77492675555986068 ) ) ;
#15069 = PLANE ( 'NONE',  #25318 ) ;
#15070 = CARTESIAN_POINT ( 'NONE',  ( 18.89824403360311678, 24.18164459663371346, 43.99464769172828937 ) ) ;
#15071 = EDGE_LOOP ( 'NONE', ( #2727, #12088 ) ) ;
#15072 = CARTESIAN_POINT ( 'NONE',  ( -259.2033419157646676, 21.55415060305790931, 35.01439189186571355 ) ) ;
#15073 = CARTESIAN_POINT ( 'NONE',  ( 0.2972598230769983307, -14.33493731733933352, 0.000000000000000000 ) ) ;
#15074 = CARTESIAN_POINT ( 'NONE',  ( -607.9053911579920850, 34.11567477793045100, 29.34757030018079860 ) ) ;
#15075 = ORIENTED_EDGE ( 'NONE', *, *, #21671, .F. ) ;
#15076 = CARTESIAN_POINT ( 'NONE',  ( -86.96347745069644475, 1.775309070576523494E-13, -18.24025645688352881 ) ) ;
#15077 = CARTESIAN_POINT ( 'NONE',  ( 199.0114802890556120, -6.820031933092490561, -18.79972423194800513 ) ) ;
#15078 = DIRECTION ( 'NONE',  ( 0.000000000000000000, 0.000000000000000000, -1.000000000000000000 ) ) ;
#15079 = VERTEX_POINT ( 'NONE', #416 ) ;
#15080 = EDGE_LOOP ( 'NONE', ( #12686, #6078, #11553, #24248 ) ) ;
#15081 = ORIENTED_EDGE ( 'NONE', *, *, #5110, .F. ) ;
#15082 = CARTESIAN_POINT ( 'NONE',  ( 14.38125909742180752, 55.17850393972636880, 2.449293598294708485E-15 ) ) ;
#15083 = EDGE_CURVE ( 'NONE', #2915, #17336, #24632, .T. ) ;
#15084 = CARTESIAN_POINT ( 'NONE',  ( -317.0000000000000568, -4.857225732735059864E-14, 0.000000000000000000 ) ) ;
#15085 = CARTESIAN_POINT ( 'NONE',  ( -199.9999999999999716, 55.16984130226958172, 2.449293598294708091E-15 ) ) ;
#15086 = CARTESIAN_POINT ( 'NONE',  ( 130.8568914410475372, 1.429239637432775288E-13, -34.05028731879788495 ) ) ;
#15087 = CARTESIAN_POINT ( 'NONE',  ( 199.9999999999999147, -4.475453068641236598, -18.46865746885900705 ) ) ;
#15088 = DIRECTION ( 'NONE',  ( 0.000000000000000000, -1.000000000000000000, 0.000000000000000000 ) ) ;
#15089 = CARTESIAN_POINT ( 'NONE',  ( 184.8905102610680444, -14.79361573936399665, 14.79361573936367158 ) ) ;
#15090 = CARTESIAN_POINT ( 'NONE',  ( 0.2972598230769976091, -10.13633138497465147, -10.13633138497482733 ) ) ;
#15091 = CARTESIAN_POINT ( 'NONE',  ( -110.0738128638427753, -17.41070106609949519, -10.28999680567891417 ) ) ;
#15092 = CARTESIAN_POINT ( 'NONE',  ( 151.7948205124836250, 1.012150473917908975E-13, -6.767089262349031742 ) ) ;
#15093 = CARTESIAN_POINT ( 'NONE',  ( 184.8905102610680444, 14.79361573936375507, 14.79361573936398067 ) ) ;
#15094 = CARTESIAN_POINT ( 'NONE',  ( 18.89824444022306338, 14.00990882958421224, 48.20791849611957502 ) ) ;
#15095 = ADVANCED_FACE ( 'NONE', ( #18633 ), #2684, .F. ) ;
#15096 = CARTESIAN_POINT ( 'NONE',  ( -91.56559293963834989, 16.03295912088683650, 40.53558337403684675 ) ) ;
#15097 = CARTESIAN_POINT ( 'NONE',  ( 199.0119184457754500, 18.47239636957207409, 7.660959720935172967 ) ) ;
#15099 = CARTESIAN_POINT ( 'NONE',  ( 151.7948205124836250, 1.439163438361279259E-13, -33.23291073765553705 ) ) ;
#15098 = CARTESIAN_POINT ( 'NONE',  ( 163.1118516004056573, -19.27778845539181063, -37.29075403953176959 ) ) ;
#15100 = CARTESIAN_POINT ( 'NONE',  ( 14.38125909742180752, 15.17850393972634038, -40.00000000000002132 ) ) ;
#15101 = CARTESIAN_POINT ( 'NONE',  ( 130.8568914410475372, -24.07718906447222551, -24.07718906447233209 ) ) ;
#15102 = CARTESIAN_POINT ( 'NONE',  ( -238.4067589809705794, 0.9644942799825385604, 40.00000000000002132 ) ) ;
#15103 = ORIENTED_EDGE ( 'NONE', *, *, #1436, .T. ) ;
#15104 = CARTESIAN_POINT ( 'NONE',  ( 22.17571259161223196, -47.24006242885573670, 13.86510691867743716 ) ) ;
#15105 =( GEOMETRIC_REPRESENTATION_CONTEXT ( 3 ) GLOBAL_UNCERTAINTY_ASSIGNED_CONTEXT ( ( #8043 ) ) GLOBAL_UNIT_ASSIGNED_CONTEXT ( ( #13101, #12966, #19214 ) ) REPRESENTATION_CONTEXT ( 'NONE', 'WORKASPACE' ) );
#15106 = CARTESIAN_POINT ( 'NONE',  ( 151.7948205124836250, 6.767089262349059275, 2.449293598294708485E-15 ) ) ;
#15107 = B_SPLINE_CURVE_WITH_KNOTS ( 'NONE', 3,
 ( #1151, #14980, #9256, #5265, #762, #11126, #13250, #13367 ),
 .UNSPECIFIED., .F., .F.,
 ( 4, 2, 2, 4 ),
 ( 0.0002282271114959515861, 0.004312393619948575417, 0.006354476874174890856, 0.008396560128401207163 ),
 .UNSPECIFIED. ) ;
#15108 = DIRECTION ( 'NONE',  ( 1.000000000000000000, 1.836970198721030181E-16, 0.000000000000000000 ) ) ;
#15109 = CARTESIAN_POINT ( 'NONE',  ( -192.9588430854690273, 10.23066800231970319, 66.79921049724369198 ) ) ;
#15110 = CARTESIAN_POINT ( 'NONE',  ( -280.0000000000000568, -40.00000000000000000, -20.00000000000015277 ) ) ;
#15111 = CARTESIAN_POINT ( 'NONE',  ( -77.66892440555722033, 21.52311491811582300, -4.720041493164197632 ) ) ;
#15112 = AXIS2_PLACEMENT_3D ( 'NONE', #9645, #8041, #24292 ) ;
#15113 = AXIS2_PLACEMENT_3D ( 'NONE', #17627, #17504, #13769 ) ;
#15114 = AXIS2_PLACEMENT_3D ( 'NONE', #24122, #9752, #24392 ) ;
#15115 = CARTESIAN_POINT ( 'NONE',  ( 200.0000000000000000, 12.97704027674654270, 13.88623514161034045 ) ) ;
#15116 = CARTESIAN_POINT ( 'NONE',  ( 23.23834162558064165, -13.80856396592285762, -46.85950693578323722 ) ) ;
#15117 = CARTESIAN_POINT ( 'NONE',  ( 199.9999999999999147, -11.82758851212937579, 14.88619241608240529 ) ) ;
#15118 = CARTESIAN_POINT ( 'NONE',  ( 136.1360204305621551, 3.511608612530062512, 53.05693388239318864 ) ) ;
#15119 = CARTESIAN_POINT ( 'NONE',  ( -82.28159816595656650, -19.22531893655055768, 6.254964767081538923 ) ) ;
#15120 = CYLINDRICAL_SURFACE ( 'NONE', #16850, 4.999999999999962697 ) ;
#15121 = FACE_OUTER_BOUND ( 'NONE', #6859, .T. ) ;
#15122 = CARTESIAN_POINT ( 'NONE',  ( 192.4448373802100889, -1.741373372144848397E-13, 20.00000000003942091 ) ) ;
#15123 = CARTESIAN_POINT ( 'NONE',  ( 19.06497207195981858, -10.03556273973469715, 66.60410523465813526 ) ) ;
#15124 = CARTESIAN_POINT ( 'NONE',  ( -82.26533530499490610, 10.28306516078108146, -17.41444274468024034 ) ) ;
#15125 = CARTESIAN_POINT ( 'NONE',  ( 146.6084372240433993, 24.48358557860307272, 24.48358557860347418 ) ) ;
#15126 = AXIS2_PLACEMENT_3D ( 'NONE', #21072, #25205, #4981 ) ;
#15128 = CARTESIAN_POINT ( 'NONE',  ( 19.06497207195981147, 38.31983398719673772, -38.31983398719579981 ) ) ;
#15127 = CARTESIAN_POINT ( 'NONE',  ( -109.1264249741456780, -33.12752917268968389, 13.72187187124619712 ) ) ;
#15129 = CARTESIAN_POINT ( 'NONE',  ( -86.96347745069644475, -15.38646221621738164, -41.18208027870615240 ) ) ;
#15130 = CARTESIAN_POINT ( 'NONE',  ( -30.26275506840324425, 41.69427246844628598, -40.00000000000002132 ) ) ;
#15131 = CARTESIAN_POINT ( 'NONE',  ( 14.38125909742180220, 39.01709431150916885, -17.55144818341463164 ) ) ;
#15132 = CARTESIAN_POINT ( 'NONE',  ( -238.4067589809705794, -4.716212492215116094E-14, 0.9644942799825824142 ) ) ;
#15133 = CARTESIAN_POINT ( 'NONE',  ( -238.4067589809705794, -28.96627169325352469, 27.60227080167035041 ) ) ;
#15134 = CARTESIAN_POINT ( 'NONE',  ( -190.0000000000000000, 1.836970198721033928E-15, 0.000000000000000000 ) ) ;
#15135 = ORIENTED_EDGE ( 'NONE', *, *, #23619, .F. ) ;
#15136 = AXIS2_PLACEMENT_3D ( 'NONE', #21655, #9416, #5297 ) ;
#15137 = CARTESIAN_POINT ( 'NONE',  ( -86.96347745069644475, 12.89780903124401057, 12.89780903124407629 ) ) ;
#15138 = CARTESIAN_POINT ( 'NONE',  ( -77.90255099906769942, 20.29001641120678201, -8.064892378658056415 ) ) ;
#15139 = CARTESIAN_POINT ( 'NONE',  ( -30.26275506840325136, 27.08623969584573388, 29.48230279907808793 ) ) ;
#15140 = CARTESIAN_POINT ( 'NONE',  ( -8.255580677125012201, -45.52720393892308692, -13.52904896324569251 ) ) ;
#15141 = VERTEX_POINT ( 'NONE', #18768 ) ;
#15142 = DIRECTION ( 'NONE',  ( -1.000000000000000000, -1.836970198721030181E-16, 0.000000000000000000 ) ) ;
#15143 = CARTESIAN_POINT ( 'NONE',  ( 199.9999999999999716, -9.233471789954972309, -16.61280101608961246 ) ) ;
#15144 = EDGE_CURVE ( 'NONE', #19457, #5443, #8656, .T. ) ;
#15145 = CARTESIAN_POINT ( 'NONE',  ( 151.7948205124836534, -33.23291073765550863, -40.00000000000002132 ) ) ;
#15146 = CARTESIAN_POINT ( 'NONE',  ( 83.07250971299875175, 9.939191265075709936, -23.99533035167571882 ) ) ;
#15147 = CARTESIAN_POINT ( 'NONE',  ( 199.0099419815959436, 19.67222971740176618, 3.604179563970075773 ) ) ;
#15148 =( BOUNDED_SURFACE ( )  B_SPLINE_SURFACE ( 3, 2, ( 
 ( #25850, #9868, #5613 ),
 ( #20251, #15706, #4029 ),
 ( #7857, #12127, #7594 ),
 ( #10134, #15978, #13719 ),
 ( #18238, #25986, #8133 ),
 ( #1629, #23830, #20118 ),
 ( #1896, #19978, #5879 ),
 ( #15837, #23, #21844 ),
 ( #14124, #19708, #17838 ),
 ( #16250, #3489, #7725 ) ),
 .UNSPECIFIED., .F., .F., .F. ) 
 B_SPLINE_SURFACE_WITH_KNOTS ( ( 4, 2, 2, 2, 4 ),
 ( 3, 3 ),
 ( 0.04143701731387906817, 0.04847035109426007377, 0.05022868453935531996, 0.05198701798445057309, 0.05550368487464107936 ),
 ( 0.000000000000000000, 1.000000000000000000 ),
 .UNSPECIFIED. ) 
 GEOMETRIC_REPRESENTATION_ITEM ( )  RATIONAL_B_SPLINE_SURFACE ( (
 ( 1.000000000000000000, 0.9541700779530978282, 1.000000000000000000),
 ( 1.000000000000000000, 0.9520138072646129324, 1.000000000000000000),
 ( 1.000000000000000000, 0.9503242346225281301, 1.000000000000000000),
 ( 1.000000000000000000, 0.9488844900984083619, 1.000000000000000000),
 ( 1.000000000000000000, 0.9486296596065902920, 1.000000000000000000),
 ( 1.000000000000000000, 0.9481942170211746790, 1.000000000000000000),
 ( 1.000000000000000000, 0.9480132043933685582, 1.000000000000000000),
 ( 1.000000000000000000, 0.9475791817278753637, 1.000000000000000000),
 ( 1.000000000000000000, 0.9474351099635109907, 1.000000000000000000),
 ( 1.000000000000000000, 0.9474350314971535791, 1.000000000000000000) ) ) 
 REPRESENTATION_ITEM ( '' )  SURFACE ( )  );
#15149 = EDGE_CURVE ( 'NONE', #495, #20259, #7501, .T. ) ;
#15150 = CARTESIAN_POINT ( 'NONE',  ( -238.4067589809705794, -0.6820004457913585449, -0.6820004457913265705 ) ) ;
#15151 = CARTESIAN_POINT ( 'NONE',  ( 136.1360204305621551, 40.00000000000017053, -35.03383547441281820 ) ) ;
#15153 = VECTOR ( 'NONE', #8385, 1000.000000000000000 ) ;
#15152 = CARTESIAN_POINT ( 'NONE',  ( -135.8532207217289738, 7.002209520526292428E-15, -9.153146818113572891 ) ) ;
#15154 = CYLINDRICAL_SURFACE ( 'NONE', #6610, 10.00000000000004796 ) ;
#15155 = CARTESIAN_POINT ( 'NONE',  ( 19.06497207195982924, -54.19242893257843008, -40.00000000000002132 ) ) ;
#15157 = CARTESIAN_POINT ( 'NONE',  ( -602.8008298560588401, 35.84274269654262923, 17.77774983073336657 ) ) ;
#15156 = CARTESIAN_POINT ( 'NONE',  ( 22.31419732600015138, -17.93420418956245399, -43.29699898481643316 ) ) ;
#15158 = ADVANCED_FACE ( 'NONE', ( #25673 ), #5193, .F. ) ;
#15159 = CARTESIAN_POINT ( 'NONE',  ( 163.1118516004056573, -12.73709011382472589, 40.00000000000002132 ) ) ;
#15160 = EDGE_CURVE ( 'NONE', #17045, #1596, #14736, .T. ) ;
#15161 = CARTESIAN_POINT ( 'NONE',  ( -100.7734535825088500, 16.03295912088713848, -16.03295912088698927 ) ) ;
#15162 = CARTESIAN_POINT ( 'NONE',  ( -30.26275506840324425, 40.00000000000044764, -41.69427246844585255 ) ) ;
#15163 = CARTESIAN_POINT ( 'NONE',  ( -114.4940140761915330, 9.297404372810827766, -19.81979918804517737 ) ) ;
#15164 = CARTESIAN_POINT ( 'NONE',  ( 130.8568914410475088, -40.00000000000036238, 34.05028731879746573 ) ) ;
#15165 = CARTESIAN_POINT ( 'NONE',  ( 199.0251223662492635, -5.665586242881555101, 19.18612710904600149 ) ) ;
#15166 = DIRECTION ( 'NONE',  ( 1.000000000000000000, 1.836970198721030181E-16, 0.000000000000000000 ) ) ;
#15167 = CARTESIAN_POINT ( 'NONE',  ( 57.59792236341147031, -1.722363176415055985, 1.722363176415024677 ) ) ;
#15168 = CARTESIAN_POINT ( 'NONE',  ( 91.82158438592159655, 12.16597498400028776, 44.40256751092339016 ) ) ;
#15169 = VERTEX_POINT ( 'NONE', #13048 ) ;
#15171 = CARTESIAN_POINT ( 'NONE',  ( -3.856733984653753389, 43.19294614843423830, -17.89110409353217079 ) ) ;
#15170 = CARTESIAN_POINT ( 'NONE',  ( -77.59212294118373165, 2.762334042793177513, -21.93719684953127569 ) ) ;
#15172 = CARTESIAN_POINT ( 'NONE',  ( 4.995406935893294431, -15.24977328854832415, 40.00000000000002132 ) ) ;
#15173 =( NAMED_UNIT ( * ) PLANE_ANGLE_UNIT ( ) SI_UNIT ( $, .RADIAN. ) );
#15174 = CARTESIAN_POINT ( 'NONE',  ( -190.0144222802798879, 43.47820992357031145, -23.79986276082225771 ) ) ;
#15175 = DIRECTION ( 'NONE',  ( 1.000000000000000000, 0.000000000000000000, 0.000000000000000000 ) ) ;
#15176 = ORIENTED_EDGE ( 'NONE', *, *, #6891, .F. ) ;
#15177 = VERTEX_POINT ( 'NONE', #5067 ) ;
#15178 = CARTESIAN_POINT ( 'NONE',  ( -30.26275506840324070, -1.198031551616032919, 1.198031551616014712 ) ) ;
#15179 = CARTESIAN_POINT ( 'NONE',  ( -210.0000000000000284, 52.49999999999987210, 82.49999999999998579 ) ) ;
#15180 = ORIENTED_EDGE ( 'NONE', *, *, #5749, .F. ) ;
#15181 = VECTOR ( 'NONE', #20695, 1000.000000000000000 ) ;
#15182 = EDGE_LOOP ( 'NONE', ( #17536, #19138, #23271, #7558 ) ) ;
#15183 = CARTESIAN_POINT ( 'NONE',  ( 199.9999999999996021, 1.536416165433052594, 18.94899354046687279 ) ) ;
#15184 = DIRECTION ( 'NONE',  ( 0.000000000000000000, 0.000000000000000000, 1.000000000000000000 ) ) ;
#15185 = CARTESIAN_POINT ( 'NONE',  ( 57.59792236341147031, -1.722363176415123043, 54.84617931850879557 ) ) ;
#15186 = CARTESIAN_POINT ( 'NONE',  ( -56.48582580120559271, -6.472252184284187138, -6.472252184284199572 ) ) ;
#15187 = CARTESIAN_POINT ( 'NONE',  ( -238.4067589809705794, 39.99999999999997158, 0.9644942799827220803 ) ) ;
#15188 = FACE_OUTER_BOUND ( 'NONE', #6523, .T. ) ;
#15189 = DIRECTION ( 'NONE',  ( 0.000000000000000000, 1.000000000000000000, 0.000000000000000000 ) ) ;
#15190 = CARTESIAN_POINT ( 'NONE',  ( -91.56559293963834989, -40.00000000000027711, 22.67402823373149801 ) ) ;
#15191 = CARTESIAN_POINT ( 'NONE',  ( -238.4067589809705794, 3.877349844572403567E-13, -40.96449427998260973 ) ) ;
#15192 = CARTESIAN_POINT ( 'NONE',  ( 190.0000000000001137, 3.490243377569959927E-14, 0.000000000000000000 ) ) ;
#15193 = CARTESIAN_POINT ( 'NONE',  ( -208.1127848780264742, -67.17687982763172272, 10.60833733270744617 ) ) ;
#15194 = CARTESIAN_POINT ( 'NONE',  ( -200.0000000000000568, 22.84381638316583008, -44.98788141756660508 ) ) ;
#15195 = EDGE_CURVE ( 'NONE', #9216, #12216, #5334, .T. ) ;
#15196 = CARTESIAN_POINT ( 'NONE',  ( -194.4222775680397319, 24.44979664543011566, 44.35790405183560381 ) ) ;
#15197 = CARTESIAN_POINT ( 'NONE',  ( -105.4741150117389168, 7.943527260764259523, 19.77569912954497866 ) ) ;
#15198 = CARTESIAN_POINT ( 'NONE',  ( -188.5332420855862097, -47.07509783859007513, 13.84065984181806819 ) ) ;
#15199 = DIRECTION ( 'NONE',  ( 1.000000000000000000, 1.836970198721030181E-16, 0.000000000000000000 ) ) ;
#15200 = CARTESIAN_POINT ( 'NONE',  ( -82.26674357278778871, -17.37244534973704191, 10.27857254525268083 ) ) ;
#15201 = CARTESIAN_POINT ( 'NONE',  ( -208.1127848780264742, -38.89260858015753541, 17.67593391476614784 ) ) ;
#15202 = CARTESIAN_POINT ( 'NONE',  ( -648.3187378681612927, 35.39633748653459122, -27.83271332065643122 ) ) ;
#15203 = CARTESIAN_POINT ( 'NONE',  ( 170.0000000000000000, 12.70659020859108601, -21.59613885783087284 ) ) ;
#15204 = ORIENTED_EDGE ( 'NONE', *, *, #1664, .T. ) ;
#15205 = CARTESIAN_POINT ( 'NONE',  ( -208.1127848780264742, 67.17687982763172272, -10.60833733270698254 ) ) ;
#15206 = CARTESIAN_POINT ( 'NONE',  ( 169.9999999999999716, 22.62041470344888339, -9.369682556672254137 ) ) ;
#15207 =( BOUNDED_SURFACE ( )  B_SPLINE_SURFACE ( 3, 2, ( 
 ( #16634, #14764, #10787 ),
 ( #18764, #6913, #4810 ),
 ( #12912, #15030, #17155 ),
 ( #23160, #24763, #6516 ),
 ( #9050, #13045, #2537 ),
 ( #19032, #22764, #548 ),
 ( #6649, #20767, #4939 ),
 ( #8785, #2936, #10655 ),
 ( #16898, #4544, #11046 ),
 ( #12642, #25289, #16760 ),
 ( #7046, #24894, #22894 ),
 ( #14895, #12775, #25030 ),
 ( #4673, #2680, #6783 ),
 ( #23035, #9173, #5064 ),
 ( #15163, #17286, #25420 ),
 ( #23288, #3065, #13170 ) ),
 .UNSPECIFIED., .F., .F., .F. ) 
 B_SPLINE_SURFACE_WITH_KNOTS ( ( 4, 2, 2, 2, 2, 2, 2, 4 ),
 ( 3, 3 ),
 ( 0.04143342415525530509, 0.04844520228004854656, 0.05195109134244516036, 0.05545698040484178110, 0.06246875852963501563, 0.06422170306083332947, 0.06597464759203164331, 0.06948053665442825710 ),
 ( 0.000000000000000000, 1.000000000000000000 ),
 .UNSPECIFIED. ) 
 GEOMETRIC_REPRESENTATION_ITEM ( )  RATIONAL_B_SPLINE_SURFACE ( (
 ( 1.000000000000000000, 0.9541700777564544600, 1.000000000000000000),
 ( 1.000000000000000000, 0.9520170179167380953, 1.000000000000000000),
 ( 1.000000000000000000, 0.9503264940257962756, 1.000000000000000000),
 ( 1.000000000000000000, 0.9485966650361820074, 1.000000000000000000),
 ( 1.000000000000000000, 0.9481601953988942899, 1.000000000000000000),
 ( 1.000000000000000000, 0.9475786562870265328, 1.000000000000000000),
 ( 1.000000000000000000, 0.9474333041668372424, 1.000000000000000000),
 ( 1.000000000000000000, 0.9474385324107064132, 1.000000000000000000),
 ( 1.000000000000000000, 0.9480205960585557090, 1.000000000000000000),
 ( 1.000000000000000000, 0.9494433550395547927, 1.000000000000000000),
 ( 1.000000000000000000, 0.9497628485354062677, 1.000000000000000000),
 ( 1.000000000000000000, 0.9504717112743313878, 1.000000000000000000),
 ( 1.000000000000000000, 0.9508623530679617408, 1.000000000000000000),
 ( 1.000000000000000000, 0.9521262215771475468, 1.000000000000000000),
 ( 1.000000000000000000, 0.9530922057181885343, 1.000000000000000000),
 ( 1.000000000000000000, 0.9541700777564462443, 1.000000000000000000) ) ) 
 REPRESENTATION_ITEM ( '' )  SURFACE ( )  );
#15208 = DIRECTION ( 'NONE',  ( -1.000000000000000000, 0.000000000000000000, 0.000000000000000000 ) ) ;
#15209 = ORIENTED_EDGE ( 'NONE', *, *, #24791, .F. ) ;
#15210 = CARTESIAN_POINT ( 'NONE',  ( -208.1127848780264742, -39.99999999999948841, -55.00245453010965235 ) ) ;
#15211 = CARTESIAN_POINT ( 'NONE',  ( 199.0176169432867255, -16.21418787309026754, -11.73480061161339272 ) ) ;
#15212 = CARTESIAN_POINT ( 'NONE',  ( -53.37769371738607305, 13.65853730965348589, 27.95780717557936157 ) ) ;
#15213 = ORIENTED_EDGE ( 'NONE', *, *, #15610, .F. ) ;
#15214 = ORIENTED_EDGE ( 'NONE', *, *, #3287, .T. ) ;
#15215 = CARTESIAN_POINT ( 'NONE',  ( -162.0762913951020892, 41.69427287682832173, 2.449293598294708485E-15 ) ) ;
#15216 = UNCERTAINTY_MEASURE_WITH_UNIT (LENGTH_MEASURE( 1.000000000000000082E-05 ), #10800, 'distance_accuracy_value', 'NONE');
#15217 = CARTESIAN_POINT ( 'NONE',  ( -175.9235640284969122, -12.95568063919091273, 42.70623598242575270 ) ) ;
#15218 = CARTESIAN_POINT ( 'NONE',  ( 14.38125909742181108, -5.035366881890652543E-14, 15.17850393972633682 ) ) ;
#15219 = CARTESIAN_POINT ( 'NONE',  ( 200.0000000000001990, -15.45587892757197146, -11.06220582312848144 ) ) ;
#15220 = CARTESIAN_POINT ( 'NONE',  ( -17.28139728231351313, -12.88180358351685406, -42.38047544416907186 ) ) ;
#15221 = CARTESIAN_POINT ( 'NONE',  ( -280.0000000000000568, 14.14213562373127431, -42.42640687119274645 ) ) ;
#15222 = CARTESIAN_POINT ( 'NONE',  ( -110.0961830520393505, -15.97565819499239481, -12.41691170628179286 ) ) ;
#15223 = CARTESIAN_POINT ( 'NONE',  ( 91.82158438592159655, -39.99999999999976552, -22.79471317813512599 ) ) ;
#15224 = DIRECTION ( 'NONE',  ( 0.000000000000000000, -1.682156097916904081E-16, -1.000000000000000000 ) ) ;
#15225 = CARTESIAN_POINT ( 'NONE',  ( 136.1360204305621266, 35.03383547441298163, -40.00000000000002132 ) ) ;
#15226 = CARTESIAN_POINT ( 'NONE',  ( 184.8905102610680444, -41.77492675555986779, -14.79361573936407304 ) ) ;
#15227 = CARTESIAN_POINT ( 'NONE',  ( 163.1118516004056573, 27.26290988616876021, -40.00000000000002132 ) ) ;
#15229 = CARTESIAN_POINT ( 'NONE',  ( -192.9588430854690273, 39.99999999999992895, 14.46834944099983922 ) ) ;
#15228 = CARTESIAN_POINT ( 'NONE',  ( 200.0000000000000000, -14.14213562373046784, -42.42640687119298804 ) ) ;
#15230 = CARTESIAN_POINT ( 'NONE',  ( 151.7948205124836250, -33.23291073765550863, 0.000000000000000000 ) ) ;
#15231 = CARTESIAN_POINT ( 'NONE',  ( -105.3755690713226585, -15.38646221621796251, 41.18208027870593924 ) ) ;
#15232 = CARTESIAN_POINT ( 'NONE',  ( -238.4067589809705794, 40.96449427998256709, 2.449293598294708485E-15 ) ) ;
#15233 = VERTEX_POINT ( 'NONE', #7419 ) ;
#15234 = CARTESIAN_POINT ( 'NONE',  ( 19.94008347562200711, -43.76810615267664417, 24.01421467034317914 ) ) ;
#15235 = CARTESIAN_POINT ( 'NONE',  ( -259.2033419157646676, 30.48217210827735713, -40.00000000000002132 ) ) ;
#15236 = CARTESIAN_POINT ( 'NONE',  ( 200.0000000000000000, 60.27431767988573341, -73.32453023895050137 ) ) ;
#15237 = CARTESIAN_POINT ( 'NONE',  ( 170.2234770963711128, -45.64576402573183600, 10.92277846919191653 ) ) ;
#15238 = B_SPLINE_CURVE_WITH_KNOTS ( 'NONE', 3,
 ( #13432, #25436, #17422, #11183, #21309, #7434, #7310, #23675, #13557, #21683, #3457, #25563 ),
 .UNSPECIFIED., .F., .F.,
 ( 4, 2, 2, 2, 2, 4 ),
 ( 2.797157557069881010E-17, 0.004680202113614255650, 0.009360404227228483545, 0.01170050528403559879, 0.01404060634084271231, 0.01872080845445698097 ),
 .UNSPECIFIED. ) ;
#15239 = CARTESIAN_POINT ( 'NONE',  ( -192.9588430854690273, -40.00000000000011369, 14.46834944099955855 ) ) ;
#15240 = CARTESIAN_POINT ( 'NONE',  ( 200.0000000000000000, 66.50000000000009948, -66.50000000000005684 ) ) ;
#15241 = EDGE_CURVE ( 'NONE', #9502, #7420, #5394, .T. ) ;
#15242 = CARTESIAN_POINT ( 'NONE',  ( 7.340276806054849779, -14.17250878947572446, -49.28408872342600944 ) ) ;
#15243 = CARTESIAN_POINT ( 'NONE',  ( 199.9999999999998863, -2.178116022715518074, 18.88665387132288487 ) ) ;
#15244 = CARTESIAN_POINT ( 'NONE',  ( -649.3705987078609496, 34.65645333158514774, -19.97733489359173120 ) ) ;
#15245 = EDGE_CURVE ( 'NONE', #15766, #3292, #1854, .T. ) ;
#15246 = CARTESIAN_POINT ( 'NONE',  ( -87.11138134864528126, -2.725552644157975379, -21.34736238710377521 ) ) ;
#15247 = CARTESIAN_POINT ( 'NONE',  ( -100.7734535825088500, 12.25131212657428748, 44.31723036834913643 ) ) ;
#15248 = VECTOR ( 'NONE', #13873, 1000.000000000000000 ) ;
#15249 = CARTESIAN_POINT ( 'NONE',  ( -100.7734535825088500, 44.31723036834907958, -12.25131212657445801 ) ) ;
#15250 = EDGE_CURVE ( 'NONE', #15670, #11173, #23788, .T. ) ;
#15251 = CARTESIAN_POINT ( 'NONE',  ( -135.8532207217289738, 34.75652343174594705, 21.81201906317792449 ) ) ;
#15252 = CARTESIAN_POINT ( 'NONE',  ( -83.28983882461061228, -25.45044590560980424, -25.45044590561024478 ) ) ;
#15253 = CARTESIAN_POINT ( 'NONE',  ( -238.4067589809705794, 27.60227080167080160, -28.96627169325299533 ) ) ;
#15255 = CARTESIAN_POINT ( 'NONE',  ( -259.2033419157646676, -35.01439189186523748, -21.55415060305881170 ) ) ;
#15254 = CARTESIAN_POINT ( 'NONE',  ( 0.2972598230769976091, -10.13633138497465147, -10.13633138497482733 ) ) ;
#15256 = CARTESIAN_POINT ( 'NONE',  ( 200.0000000000000000, 42.42640687119267540, 14.14213562373153543 ) ) ;
#15257 = CIRCLE ( 'NONE', #12774, 15.00000000000000000 ) ;
#15258 = CARTESIAN_POINT ( 'NONE',  ( -162.0762913951020892, 1.694272876828294194, 0.000000000000000000 ) ) ;
#15259 = FACE_OUTER_BOUND ( 'NONE', #4987, .T. ) ;
#15260 = CARTESIAN_POINT ( 'NONE',  ( -91.56559293963834989, 6.234561990864368500E-14, -22.67402823373191723 ) ) ;
#15261 = CARTESIAN_POINT ( 'NONE',  ( -105.3755690713226585, -12.89780903124444578, 43.67073346367968156 ) ) ;
#15262 = CARTESIAN_POINT ( 'NONE',  ( -188.3508614409174129, 43.15762572182595136, -17.87647389380071772 ) ) ;
#15263 = ORIENTED_EDGE ( 'NONE', *, *, #1668, .F. ) ;
#15264 = CARTESIAN_POINT ( 'NONE',  ( -198.0356074513804572, 39.15871834505901461, 39.15871834505919935 ) ) ;
#15265 = DIRECTION ( 'NONE',  ( -1.000000000000000000, 0.000000000000000000, 0.000000000000000000 ) ) ;
#15266 = CARTESIAN_POINT ( 'NONE',  ( 11.38508063392505321, 14.17561098846279144, 49.30460303391076593 ) ) ;
#15267 = CARTESIAN_POINT ( 'NONE',  ( -86.86493150571114086, -19.77569912839162569, 7.943527260496431985 ) ) ;
#15268 = VERTEX_POINT ( 'NONE', #7550 ) ;
#15269 = DIRECTION ( 'NONE',  ( 0.000000000000000000, -1.000000000000000000, 0.000000000000000000 ) ) ;
#15270 = CARTESIAN_POINT ( 'NONE',  ( 200.0000000000002558, -1.250172057809772586, -18.97074946354465652 ) ) ;
#15271 = CARTESIAN_POINT ( 'NONE',  ( 22.89002945277442791, -17.87003923493671920, 43.14209108112122237 ) ) ;
#15272 = VECTOR ( 'NONE', #24509, 1000.000000000000000 ) ;
#15273 = FACE_OUTER_BOUND ( 'NONE', #3197, .T. ) ;
#15274 = CARTESIAN_POINT ( 'NONE',  ( 199.0056246187962188, 17.07746298573517052, -10.40099104823843312 ) ) ;
#15275 = CARTESIAN_POINT ( 'NONE',  ( 98.29820294270304259, -18.47759065022024672, 7.653668647299475047 ) ) ;
#15276 = CARTESIAN_POINT ( 'NONE',  ( 0.2972598230769957217, -4.999556039334937811E-14, 14.33493731733933352 ) ) ;
#15277 = CARTESIAN_POINT ( 'NONE',  ( -87.02160325129693774, -5.407498138847803837, 20.76752817463990652 ) ) ;
#15278 = CARTESIAN_POINT ( 'NONE',  ( 5.009865950673472845, 49.09576456953151080, -14.14399394884951455 ) ) ;
#15279 = CARTESIAN_POINT ( 'NONE',  ( -100.7734535825088358, -17.32597176626813251, -2.449293598294708485E-15 ) ) ;
#15281 = CARTESIAN_POINT ( 'NONE',  ( -56.48582580120559271, 6.472252184284211118, -6.472252184284153387 ) ) ;
#15280 = CARTESIAN_POINT ( 'NONE',  ( 21.80824205439828134, -23.67346680102911094, -43.30754100652708871 ) ) ;
#15282 = CARTESIAN_POINT ( 'NONE',  ( 146.6084372240433709, 34.62501878078307982, 40.00000000000002132 ) ) ;
#15283 = CARTESIAN_POINT ( 'NONE',  ( -259.2033419157646676, 9.517827891722584255, -0.000000000000000000 ) ) ;
#15284 = CARTESIAN_POINT ( 'NONE',  ( 184.8905102610680444, -1.851754852062639767E-13, 20.92133201514444352 ) ) ;
#15285 = CARTESIAN_POINT ( 'NONE',  ( -213.1075012329537230, -39.99999999999948841, -53.71589010950208376 ) ) ;
#15286 = CIRCLE ( 'NONE', #1641, 5.000000000000004441 ) ;
#15287 = CARTESIAN_POINT ( 'NONE',  ( 121.8729990817667641, -26.81364411578696405, -11.10657504940452611 ) ) ;
#15288 = CARTESIAN_POINT ( 'NONE',  ( 4.995406935893289102, 10.78321810389013002, -10.78321810388986712 ) ) ;
#15289 = ORIENTED_EDGE ( 'NONE', *, *, #18838, .F. ) ;
#15291 = CARTESIAN_POINT ( 'NONE',  ( -3.439026802539385752, 43.30533194338906355, -17.93765581402026754 ) ) ;
#15290 = CARTESIAN_POINT ( 'NONE',  ( 0.2972598230769976091, -10.13633138497465147, -10.13633138497482733 ) ) ;
#15292 = CARTESIAN_POINT ( 'NONE',  ( 199.9999999999999432, -19.99999999999988987, -2.449293598294708485E-15 ) ) ;
#15293 = ADVANCED_FACE ( 'NONE', ( #26344 ), #18617, .T. ) ;
#15294 = MECHANICAL_DESIGN_GEOMETRIC_PRESENTATION_REPRESENTATION (  '', ( #442 ), #12327 ) ;
#15295 = CARTESIAN_POINT ( 'NONE',  ( -188.3392535381850621, 43.01687576774367727, -23.45796413246022638 ) ) ;
#15296 = CARTESIAN_POINT ( 'NONE',  ( -974.1419610881682729, -3.002497395983190491E-14, -4.489167474665349580E-14 ) ) ;
#15297 = ORIENTED_EDGE ( 'NONE', *, *, #1499, .F. ) ;
#15298 = VERTEX_POINT ( 'NONE', #24026 ) ;
#15299 = CARTESIAN_POINT ( 'NONE',  ( 180.0000000000000000, -35.78896085774750446, 65.91016826501511616 ) ) ;
#15300 = PLANE ( 'NONE',  #11492 ) ;
#15301 = CARTESIAN_POINT ( 'NONE',  ( 136.1360204305621266, 1.473277640373554421E-13, -35.03383547441296741 ) ) ;
#15302 = ORIENTED_EDGE ( 'NONE', *, *, #13619, .T. ) ;
#15303 = CARTESIAN_POINT ( 'NONE',  ( 199.9999999999998579, -4.480715147297966716, 18.47471730767352938 ) ) ;
#15304 = CARTESIAN_POINT ( 'NONE',  ( -188.2995950289364373, 13.82811170417132196, 46.99046209955516673 ) ) ;
#15305 = ADVANCED_FACE ( 'NONE', ( #17766 ), #23369, .F. ) ;
#15306 = CARTESIAN_POINT ( 'NONE',  ( -100.7734535825088500, 40.53558337403677569, -16.03295912088699993 ) ) ;
#15307 = CARTESIAN_POINT ( 'NONE',  ( 180.0000000000000000, -66.50000000000001421, 66.50000000000005684 ) ) ;
#15308 = CARTESIAN_POINT ( 'NONE',  ( -208.1127848780265026, -9.061048840815752106E-14, 15.00245453012669472 ) ) ;
#15309 = CARTESIAN_POINT ( 'NONE',  ( 0.4226707250629958557, -14.03458789212657720, 48.37218667320259868 ) ) ;
#15310 = CARTESIAN_POINT ( 'NONE',  ( -210.0000000000000284, 60.27431767988564104, -73.32453023895048716 ) ) ;
#15311 = AXIS2_PLACEMENT_3D ( 'NONE', #9197, #5459, #9573 ) ;
#15312 = CARTESIAN_POINT ( 'NONE',  ( 57.59792236341149163, -39.99999999999961631, -37.56421063658228832 ) ) ;
#15313 = CARTESIAN_POINT ( 'NONE',  ( -198.0356074513804572, 5.461327841961909642E-13, -55.37879056873073580 ) ) ;
#15314 = CARTESIAN_POINT ( 'NONE',  ( -110.0574180503312363, -18.01801597171421676, 9.169691069511660686 ) ) ;
#15315 = CARTESIAN_POINT ( 'NONE',  ( -238.4067589809705794, -57.25054294065807881, 0.6820004457338858517 ) ) ;
#15316 = CARTESIAN_POINT ( 'NONE',  ( 192.4448373802101173, 40.00000000000012790, -20.00000000003928236 ) ) ;
#15317 = DIRECTION ( 'NONE',  ( -1.000000000000000000, -0.000000000000000000, -0.000000000000000000 ) ) ;
#15318 = CARTESIAN_POINT ( 'NONE',  ( 210.0000000000000284, 61.50000000000009948, -66.50000000000005684 ) ) ;
#15319 = B_SPLINE_CURVE_WITH_KNOTS ( 'NONE', 3,
 ( #12527, #15056, #16528, #24790, #20526, #4701, #20661, #22922, #12808, #24656, #838, #20930, #4434, #22662 ),
 .UNSPECIFIED., .F., .F.,
 ( 4, 2, 2, 2, 2, 2, 4 ),
 ( 1.734723475976806902E-18, 0.002941681445496980695, 0.004412522168245476897, 0.005883362890993972666, 0.008825044336490964203, 0.01029588505923946344, 0.01176672578198796268 ),
 .UNSPECIFIED. ) ;
#15320 = CYLINDRICAL_SURFACE ( 'NONE', #918, 34.99999999999999289 ) ;
#15321 = CARTESIAN_POINT ( 'NONE',  ( 4.995406935893293543, -10.78321810389005364, 10.78321810388994173 ) ) ;
#15322 = CARTESIAN_POINT ( 'NONE',  ( -77.90255099906779890, -8.644468104261020969, 20.04994828523974704 ) ) ;
#15323 = CARTESIAN_POINT ( 'NONE',  ( -86.96347745069644475, 12.89780903124401057, 12.89780903124407629 ) ) ;
#15324 = CARTESIAN_POINT ( 'NONE',  ( 199.9999999999999432, -14.14213562373073607, -14.14213562373102206 ) ) ;
#15325 = CARTESIAN_POINT ( 'NONE',  ( -144.0562696876088182, -10.50947022294722011, -31.27040355054280951 ) ) ;
#15326 = CARTESIAN_POINT ( 'NONE',  ( 170.0000000000000000, 15.47746304364920356, -19.80854622259135311 ) ) ;
#15327 = ORIENTED_EDGE ( 'NONE', *, *, #11555, .T. ) ;
#15328 = CARTESIAN_POINT ( 'NONE',  ( 163.1118516004056573, 9.006482792069759213, -9.006482792069505194 ) ) ;
#15329 = CYLINDRICAL_SURFACE ( 'NONE', #3500, 30.00000000000004974 ) ;
#15330 = EDGE_CURVE ( 'NONE', #18515, #13337, #6507, .T. ) ;
#15331 = CARTESIAN_POINT ( 'NONE',  ( -609.3084111456423670, 33.35105114729260833, 30.21346475632024209 ) ) ;
#15332 = ORIENTED_EDGE ( 'NONE', *, *, #5390, .F. ) ;
#15333 = CARTESIAN_POINT ( 'NONE',  ( 14.38125909742181108, 1.616281842095393922E-13, -15.17850393972633682 ) ) ;
#15334 = CARTESIAN_POINT ( 'NONE',  ( 199.0179802867041019, -16.61558597860446440, -11.15304595324047554 ) ) ;
#15335 = CARTESIAN_POINT ( 'NONE',  ( -2.937533998796872048, -43.32931883107630711, 23.68967259549630455 ) ) ;
#15336 = AXIS2_PLACEMENT_3D ( 'NONE', #23446, #1616, #9335 ) ;
#15337 = ORIENTED_EDGE ( 'NONE', *, *, #3381, .T. ) ;
#15338 = ORIENTED_EDGE ( 'NONE', *, *, #12641, .F. ) ;
#15339 = CARTESIAN_POINT ( 'NONE',  ( -259.2033419157646676, -21.55415060305824326, -35.01439189186556433 ) ) ;
#15340 = CARTESIAN_POINT ( 'NONE',  ( 163.1118516004056573, -1.695744499706194789E-14, 12.73709011382475254 ) ) ;
#15341 = EDGE_CURVE ( 'NONE', #18786, #15843, #10428, .T. ) ;
#15342 = EDGE_CURVE ( 'NONE', #3040, #8031, #1291, .T. ) ;
#15343 = FACE_OUTER_BOUND ( 'NONE', #7179, .T. ) ;
#15344 = PRODUCT_DEFINITION_CONTEXT ( 'detailed design', #2056, 'design' ) ;
#15345 = CARTESIAN_POINT ( 'NONE',  ( -198.0356074513804572, 39.15871834505956173, -39.15871834505865223 ) ) ;
#15346 = DIRECTION ( 'NONE',  ( 0.000000000000000000, 0.000000000000000000, 1.000000000000000000 ) ) ;
#15347 = CARTESIAN_POINT ( 'NONE',  ( 199.9999999999997442, -19.00693066143141152, -0.3125757794583984839 ) ) ;
#15348 = CIRCLE ( 'NONE', #6842, 5.000000000000004441 ) ;
#15349 = CARTESIAN_POINT ( 'NONE',  ( -83.21262154144247347, -13.72187187061530977, 33.12752917118402962 ) ) ;
#15350 = CIRCLE ( 'NONE', #3902, 5.000000000000004441 ) ;
#15351 = CARTESIAN_POINT ( 'NONE',  ( -47.65341557553326624, -14.80716566697267211, -29.74088027399182010 ) ) ;
#15352 = CARTESIAN_POINT ( 'NONE',  ( 19.06497207195981858, -10.03556273973377166, -66.60410523465827737 ) ) ;
#15353 = CARTESIAN_POINT ( 'NONE',  ( 98.29820294267423719, -14.14213562374330024, 14.14213562372619926 ) ) ;
#15354 = CARTESIAN_POINT ( 'NONE',  ( -105.3755690713226727, 1.741486606973311632E-13, -18.24025645688352881 ) ) ;
#15355 = CARTESIAN_POINT ( 'NONE',  ( 210.0000000000000284, 63.70262460423112572, -57.69613583541415380 ) ) ;
#15356 = CARTESIAN_POINT ( 'NONE',  ( 4.995406935893294431, -15.24977328854832415, 40.00000000000002132 ) ) ;
#15357 = CARTESIAN_POINT ( 'NONE',  ( -213.1075012329537230, -13.71589010951915810, -40.00000000000002132 ) ) ;
#15358 = CARTESIAN_POINT ( 'NONE',  ( -192.9588430854690273, 18.05360324515418924, 38.51493924976949756 ) ) ;
#15359 = CARTESIAN_POINT ( 'NONE',  ( -86.96347745069643054, -18.24025645688353947, -40.00000000000002132 ) ) ;
#15361 = CARTESIAN_POINT ( 'NONE',  ( -198.0356074513804572, 39.99999999999992895, 15.37879056873084771 ) ) ;
#15360 = CARTESIAN_POINT ( 'NONE',  ( 98.29820294272737158, 12.38338430224885656, 15.90088694521805301 ) ) ;
#15362 = CARTESIAN_POINT ( 'NONE',  ( -190.0000000000000000, -52.49999999999970868, 82.49999999999998579 ) ) ;
#15363 = CARTESIAN_POINT ( 'NONE',  ( -105.3755690713226585, 41.18208027870598187, -15.38646221621779731 ) ) ;
#15364 = CARTESIAN_POINT ( 'NONE',  ( 146.6084372240433993, 5.374981219216999229, 2.449293598294708485E-15 ) ) ;
#15365 = ORIENTED_EDGE ( 'NONE', *, *, #3611, .F. ) ;
#15366 = CARTESIAN_POINT ( 'NONE',  ( 23.26364522860174944, -42.89098160628003598, 23.36474233297283121 ) ) ;
#15367 = VECTOR ( 'NONE', #10539, 1000.000000000000000 ) ;
#15368 = CARTESIAN_POINT ( 'NONE',  ( 190.0000000000000000, 52.49999999999987210, 82.49999999999998579 ) ) ;
#15369 = CARTESIAN_POINT ( 'NONE',  ( 14.38125909742181463, 10.73282306405862485, 67.30136555898259587 ) ) ;
#15370 = CARTESIAN_POINT ( 'NONE',  ( 136.1360204305621266, 1.473277640373554421E-13, -35.03383547441296741 ) ) ;
#15371 = CARTESIAN_POINT ( 'NONE',  ( -77.56706372485132306, 22.07323241864502350, 1.630297477738017475 ) ) ;
#15372 = CARTESIAN_POINT ( 'NONE',  ( -8.255580677152625668, 22.62611236875380882, -41.75907689858282623 ) ) ;
#15373 = CARTESIAN_POINT ( 'NONE',  ( 199.9999999999998010, 4.909892096549036467, 18.36538930945351566 ) ) ;
#15374 = CARTESIAN_POINT ( 'NONE',  ( -634.0640263162007386, 27.37139587162865340, -29.17014862255485852 ) ) ;
#15375 = CARTESIAN_POINT ( 'NONE',  ( -77.79459117303389348, -6.798990169609631096, -20.85444474317636221 ) ) ;
#15376 = CARTESIAN_POINT ( 'NONE',  ( -280.0000000000000568, 14.14213562373038968, 42.42640687119305198 ) ) ;
#15377 = CARTESIAN_POINT ( 'NONE',  ( -238.4067589809705794, -28.96627169325303797, -28.96627169325349627 ) ) ;
#15378 = CARTESIAN_POINT ( 'NONE',  ( -280.0000000000000000, 14.14213562373098299, -14.14213562373088706 ) ) ;
#15379 = CARTESIAN_POINT ( 'NONE',  ( 4.995406935893289102, 10.78321810389013002, -10.78321810388986712 ) ) ;
#15380 = CARTESIAN_POINT ( 'NONE',  ( 91.82158438592159655, 12.16597498400091304, -44.40256751092321963 ) ) ;
#15381 = CIRCLE ( 'NONE', #3934, 5.000000000000004441 ) ;
#15383 = CARTESIAN_POINT ( 'NONE',  ( 163.1118516004056573, -19.27778845539181063, -37.29075403953176959 ) ) ;
#15382 = CARTESIAN_POINT ( 'NONE',  ( 192.4448373802101173, 14.14213562375922884, -42.42640687116488607 ) ) ;
#15384 = CARTESIAN_POINT ( 'NONE',  ( 57.59792236341147031, 26.56190807104720975, -26.56190807104655249 ) ) ;
#15385 = CARTESIAN_POINT ( 'NONE',  ( -105.3895334812081046, -9.637394427343657810, 19.08270859417689636 ) ) ;
#15386 = CARTESIAN_POINT ( 'NONE',  ( 190.0000000000000000, -61.50000000000001421, -66.50000000000005684 ) ) ;
#15387 = CARTESIAN_POINT ( 'NONE',  ( 151.7948205124835681, -4.785054706298876859, 51.78348778862533663 ) ) ;
#15388 = CARTESIAN_POINT ( 'NONE',  ( -188.2506440019887464, 42.99080317017362063, -23.43978047293228073 ) ) ;
#15389 = EDGE_LOOP ( 'NONE', ( #2065, #25432, #24, #7589 ) ) ;
#15390 = CARTESIAN_POINT ( 'NONE',  ( -192.9588430854690273, 38.51493924976939098, -18.05360324515436687 ) ) ;
#15391 = CARTESIAN_POINT ( 'NONE',  ( -77.90255099906777048, -20.04994828523985362, -8.644468104260763397 ) ) ;
#15392 = CARTESIAN_POINT ( 'NONE',  ( 23.64688638900176798, 13.78084749393323705, 46.70960658758804129 ) ) ;
#15393 = CARTESIAN_POINT ( 'NONE',  ( -7.726389047727876047, -42.14052505959300987, -17.45517700519032900 ) ) ;
#15394 = ORIENTED_EDGE ( 'NONE', *, *, #12837, .F. ) ;
#15395 = CARTESIAN_POINT ( 'NONE',  ( -174.2681662547478822, -39.26785901283194136, 16.26527976840799639 ) ) ;
#15396 = ADVANCED_FACE ( 'NONE', ( #25150 ), #5426, .T. ) ;
#15397 = CARTESIAN_POINT ( 'NONE',  ( 199.9999999999997442, 1.230017881244859446, -18.96210773722240361 ) ) ;
#15398 = CARTESIAN_POINT ( 'NONE',  ( 27.79909650601494064, -22.43832426414681080, 41.49206490658713875 ) ) ;
#15399 = CARTESIAN_POINT ( 'NONE',  ( 170.0000000000427178, -17.64300463311358769, 17.64300463311318268 ) ) ;
#15400 = CARTESIAN_POINT ( 'NONE',  ( 199.0055651108938832, 16.81514173603054374, -10.81990435933588302 ) ) ;
#15401 = CARTESIAN_POINT ( 'NONE',  ( -100.0753760173616058, -20.41987330121787636, -8.894334231739460250 ) ) ;
#15402 = CARTESIAN_POINT ( 'NONE',  ( -56.48582580120559982, 39.99999999999990763, 30.84685318188658698 ) ) ;
#15403 = CARTESIAN_POINT ( 'NONE',  ( -83.21262154144264400, 13.72187187061491720, -33.12752917118420726 ) ) ;
#15404 = CARTESIAN_POINT ( 'NONE',  ( -199.9999999999999432, -21.40989205436278908, -45.24754806069001489 ) ) ;
#15405 = CARTESIAN_POINT ( 'NONE',  ( -135.8532207217289454, -30.84685318188649106, 40.00000000000002132 ) ) ;
#15407 = FACE_OUTER_BOUND ( 'NONE', #26291, .T. ) ;
#15406 = CARTESIAN_POINT ( 'NONE',  ( 67.79414719528381283, -10.30785037377898661, -30.31905270957335929 ) ) ;
#15408 = CARTESIAN_POINT ( 'NONE',  ( 4.995406935893294431, -15.24977328854832415, 40.00000000000002132 ) ) ;
#15409 = CARTESIAN_POINT ( 'NONE',  ( -162.0762913951020892, -1.694272876828353702, 0.000000000000000000 ) ) ;
#15410 = CARTESIAN_POINT ( 'NONE',  ( 146.6084372240433709, 39.99999999999968026, 34.62501878078347772 ) ) ;
#15411 = CARTESIAN_POINT ( 'NONE',  ( -259.2033419157646676, -40.00000000000017053, 9.517827891722212996 ) ) ;
#15412 = CARTESIAN_POINT ( 'NONE',  ( 156.1976257969618587, -27.38429663762786248, -11.34294706335341196 ) ) ;
#15413 = ORIENTED_EDGE ( 'NONE', *, *, #12425, .F. ) ;
#15415 = CARTESIAN_POINT ( 'NONE',  ( -4.112199523539852741, 42.98379141459112418, -23.43514144949442723 ) ) ;
#15414 = FACE_OUTER_BOUND ( 'NONE', #5618, .T. ) ;
#15416 = CARTESIAN_POINT ( 'NONE',  ( 136.1360204305621551, -4.966164525587043244, 40.00000000000002132 ) ) ;
#15417 = CARTESIAN_POINT ( 'NONE',  ( -126.6834154282210108, -24.89646316986487662, 9.107266658309272955 ) ) ;
#15418 = CARTESIAN_POINT ( 'NONE',  ( -188.4265004370459735, 43.04236487214743789, -23.47686928852965593 ) ) ;
#15419 = DIRECTION ( 'NONE',  ( 1.000000000000000000, 0.000000000000000000, 0.000000000000000000 ) ) ;
#15420 = EDGE_LOOP ( 'NONE', ( #18144, #24107, #16744, #2825 ) ) ;
#15421 = ORIENTED_EDGE ( 'NONE', *, *, #19531, .T. ) ;
#15422 = CARTESIAN_POINT ( 'NONE',  ( -96.93773665439012177, -20.58457565566412129, 9.001171854901890867 ) ) ;
#15423 = CARTESIAN_POINT ( 'NONE',  ( 133.2080217031554525, 12.38638889282743527, -29.90338805389109922 ) ) ;
#15424 = LINE ( 'NONE', #11429, #21106 ) ;
#15425 = EDGE_LOOP ( 'NONE', ( #14289, #10430, #25654, #1332, #10866 ) ) ;
#15426 = CARTESIAN_POINT ( 'NONE',  ( 200.0000000000000000, 2.003163845861910097, 18.90332168644373567 ) ) ;
#15427 = DIRECTION ( 'NONE',  ( 1.750717563385751339E-16, -0.9530462522498560629, -0.3028247695821853491 ) ) ;
#15428 = CARTESIAN_POINT ( 'NONE',  ( 130.8568914410475088, 32.49135343045483637, -24.07718906446901030 ) ) ;
#15429 = CARTESIAN_POINT ( 'NONE',  ( -716.9846540392142060, 52.49999999999991473, -82.49999999999998579 ) ) ;
#15430 = CARTESIAN_POINT ( 'NONE',  ( -86.96347745069644475, 5.999880687339585546E-14, -21.75974354311649961 ) ) ;
#15431 = DIRECTION ( 'NONE',  ( -1.000000000000000000, -1.836970198721030181E-16, -0.000000000000000000 ) ) ;
#15432 = DIRECTION ( 'NONE',  ( 0.000000000000000000, -0.9767746502210199466, 0.2142691827715878239 ) ) ;
#15433 = DIRECTION ( 'NONE',  ( 0.000000000000000000, -1.000000000000000000, 0.000000000000000000 ) ) ;
#15434 = CARTESIAN_POINT ( 'NONE',  ( -208.1127848780264742, -39.99999999999948841, -55.00245453010965235 ) ) ;
#15435 = CARTESIAN_POINT ( 'NONE',  ( 163.1118516004056573, 1.658263919738574066E-13, -12.73709011382475254 ) ) ;
#15436 = CARTESIAN_POINT ( 'NONE',  ( -82.23879574654692703, 15.18736141609909751, 13.32665427271416014 ) ) ;
#15437 = CARTESIAN_POINT ( 'NONE',  ( 19.06497207195981147, -10.03556273973439517, 10.03556273973429214 ) ) ;
#15438 = CARTESIAN_POINT ( 'NONE',  ( -213.1075012329537230, -8.703598725189323045E-14, 13.71589010951911902 ) ) ;
#15439 = CARTESIAN_POINT ( 'NONE',  ( 163.1118516004056573, 19.27778845538780317, -19.27778845538757224 ) ) ;
#15440 = CARTESIAN_POINT ( 'NONE',  ( 158.3379117892986585, 26.51167085133952739, 10.98149362779641791 ) ) ;
#15441 = CARTESIAN_POINT ( 'NONE',  ( -77.90255099906859471, -8.644468104251766150, 20.04994828524300843 ) ) ;
#15442 = CARTESIAN_POINT ( 'NONE',  ( -626.9846540392140923, 26.45751311064577749, 30.00000000000005329 ) ) ;
#15443 = CARTESIAN_POINT ( 'NONE',  ( -77.79459117301121296, -19.55393134993891380, 9.938707241634757494 ) ) ;
#15444 = CARTESIAN_POINT ( 'NONE',  ( 184.8905102610680444, -43.07788698682576722, 13.49065550809799063 ) ) ;
#15445 = CARTESIAN_POINT ( 'NONE',  ( -135.8532207217289738, -21.81201906317806305, 34.75652343174590442 ) ) ;
#15446 = CARTESIAN_POINT ( 'NONE',  ( -649.9986597873944447, 36.44533412639378867, -26.46011044280707836 ) ) ;
#15447 = EDGE_CURVE ( 'NONE', #12932, #3239, #16002, .T. ) ;
#15448 = CARTESIAN_POINT ( 'NONE',  ( -626.9846540392142060, 105.0000000000000000, 46.18033988749894547 ) ) ;
#15449 = ORIENTED_EDGE ( 'NONE', *, *, #12722, .T. ) ;
#15450 = CARTESIAN_POINT ( 'NONE',  ( -192.9588430854690273, 10.23066800229588758, -66.79921049721882298 ) ) ;
#15451 = CARTESIAN_POINT ( 'NONE',  ( -200.0000000000000000, -71.50000000000002842, -66.50000000000005684 ) ) ;
#15452 = CARTESIAN_POINT ( 'NONE',  ( -109.1264249741456780, -13.72187187121290108, 33.12752917270401554 ) ) ;
#15453 = EDGE_LOOP ( 'NONE', ( #7730, #15640, #12516, #22475 ) ) ;
#15454 = DIRECTION ( 'NONE',  ( 0.000000000000000000, 0.000000000000000000, -1.000000000000000000 ) ) ;
#15455 = CARTESIAN_POINT ( 'NONE',  ( -3.901164313503183045, -23.47934491069901597, 43.04571088859064787 ) ) ;
#15456 = CARTESIAN_POINT ( 'NONE',  ( -77.90255099907078318, 8.064892378657827265, 20.29001641120558830 ) ) ;
#15457 = VERTEX_POINT ( 'NONE', #3425 ) ;
#15458 = ORIENTED_EDGE ( 'NONE', *, *, #9390, .T. ) ;
#15459 = CARTESIAN_POINT ( 'NONE',  ( -200.5022929845067949, -44.86988025226713717, -18.58571294254476314 ) ) ;
#15460 = CARTESIAN_POINT ( 'NONE',  ( 57.59792236341147742, -1.230234673553095937E-13, 37.56421063658186199 ) ) ;
#15461 = CARTESIAN_POINT ( 'NONE',  ( -89.91646883266054147, -20.29783361042684575, -8.407637968085085234 ) ) ;
#15462 = EDGE_CURVE ( 'NONE', #7987, #3167, #17704, .T. ) ;
#15463 = CARTESIAN_POINT ( 'NONE',  ( 184.5686700507837656, 13.43430831934472103, -13.43430831934435510 ) ) ;
#15464 = CARTESIAN_POINT ( 'NONE',  ( -91.56559293963834989, -40.00000000000009948, 17.32597176626796553 ) ) ;
#15465 = CARTESIAN_POINT ( 'NONE',  ( 200.0000000000000568, -11.58056098922197563, -15.07187815445410806 ) ) ;
#15466 = PLANE ( 'NONE',  #12193 ) ;
#15467 = CARTESIAN_POINT ( 'NONE',  ( -77.90022806218901508, -8.352332316461509976, -20.16431395584806907 ) ) ;
#15468 = CARTESIAN_POINT ( 'NONE',  ( 130.8568914410475372, 24.07718906447210472, 24.07718906447249907 ) ) ;
#15469 = DIRECTION ( 'NONE',  ( 0.000000000000000000, 0.6739498806388345420, 0.7387770694782699321 ) ) ;
#15470 = CARTESIAN_POINT ( 'NONE',  ( -198.0356074513804572, -39.99999999999948130, -55.37879056874863437 ) ) ;
#15471 = CARTESIAN_POINT ( 'NONE',  ( -105.2054292635175585, -21.49321519473986442, -7.030298963786045751E-29 ) ) ;
#15472 = CARTESIAN_POINT ( 'NONE',  ( -213.1075012329537230, -13.71589010951915810, 40.00000000000002132 ) ) ;
#15473 = CARTESIAN_POINT ( 'NONE',  ( -213.1075012329537230, -53.71589010953668719, -40.00000000000002132 ) ) ;
#15474 = ADVANCED_FACE ( 'NONE', ( #19402 ), #17013, .T. ) ;
#15475 = EDGE_CURVE ( 'NONE', #11726, #17509, #603, .T. ) ;
#15476 = CARTESIAN_POINT ( 'NONE',  ( -86.96347745069644475, 15.38646221621793586, -15.38646221621778842 ) ) ;
#15477 = CARTESIAN_POINT ( 'NONE',  ( -162.0762913951021176, -1.694272876828353702, -40.00000000000002132 ) ) ;
#15479 = DIRECTION ( 'NONE',  ( 0.9352143323239480166, -0.1355013636715377279, -0.3271292299062040776 ) ) ;
#15478 = CARTESIAN_POINT ( 'NONE',  ( -678.9461782662772293, 75.00000000000000000, 30.00000000000158096 ) ) ;
#15480 = CARTESIAN_POINT ( 'NONE',  ( 19.06497207195981147, 1.521599808664285085E-13, -14.19242893257840521 ) ) ;
#15481 = CARTESIAN_POINT ( 'NONE',  ( 57.59792236341147031, 26.56190807104684382, 26.56190807104692553 ) ) ;
#15482 = CARTESIAN_POINT ( 'NONE',  ( -259.2033419157646676, 30.48217210827734647, 2.449293598294708485E-15 ) ) ;
#15483 = ORIENTED_EDGE ( 'NONE', *, *, #3391, .F. ) ;
#15484 = CARTESIAN_POINT ( 'NONE',  ( 25.05785482535806707, -42.53113694076518669, 17.61697374403330585 ) ) ;
#15485 = DIRECTION ( 'NONE',  ( 0.000000000000000000, 1.000000000000000000, 0.000000000000000000 ) ) ;
#15486 = CARTESIAN_POINT ( 'NONE',  ( 0.2972598230769959993, 38.42060263243659080, 38.42060263243672580 ) ) ;
#15487 = CARTESIAN_POINT ( 'NONE',  ( -208.1127848780265026, -9.061048840815752106E-14, 15.00245453012669472 ) ) ;
#15488 = CARTESIAN_POINT ( 'NONE',  ( -87.13563633338503678, 21.50639108511650122, -1.206565891102790777 ) ) ;
#15489 = CARTESIAN_POINT ( 'NONE',  ( 3.854699808470068767, -14.12217777258740270, -48.95177852071788038 ) ) ;
#15490 = CARTESIAN_POINT ( 'NONE',  ( 200.0000000000000000, 9.224923989862913842, 16.61864493261536424 ) ) ;
#15491 = CARTESIAN_POINT ( 'NONE',  ( -86.86493150571118349, -19.77569912839185307, -7.943527260495925724 ) ) ;
#15492 = CARTESIAN_POINT ( 'NONE',  ( -87.13348102042543530, -1.376917454623202364, -21.49232615835870419 ) ) ;
#15493 = CARTESIAN_POINT ( 'NONE',  ( -198.0356074513804572, 10.87444709759730088, -10.87444709759707173 ) ) ;
#15494 = CARTESIAN_POINT ( 'NONE',  ( -100.7734535825088358, -12.25131212657475643, -12.25131212657495539 ) ) ;
#15495 = CARTESIAN_POINT ( 'NONE',  ( -110.1004897823566324, 20.16745930835667266, -1.096875637590350339 ) ) ;
#15496 = CARTESIAN_POINT ( 'NONE',  ( -86.86493150571114086, -8.366608963953616751, 19.60045294882772993 ) ) ;
#15497 = CARTESIAN_POINT ( 'NONE',  ( -198.0356074513804572, -10.87444709758429262, -67.44298959250878056 ) ) ;
#15499 = CARTESIAN_POINT ( 'NONE',  ( -208.1127848780264742, -17.67593391476605547, -38.89260858015755673 ) ) ;
#15498 = CARTESIAN_POINT ( 'NONE',  ( -259.2033419157646676, 6.730120644403918995, -49.83842185052024831 ) ) ;
#15500 = CARTESIAN_POINT ( 'NONE',  ( 91.82158438592158234, 16.11829626346161604, -16.11829626346121103 ) ) ;
#15501 = DIRECTION ( 'NONE',  ( 0.000000000000000000, 0.000000000000000000, 1.000000000000000000 ) ) ;
#15502 = CYLINDRICAL_SURFACE ( 'NONE', #25136, 5.000000000000011546 ) ;
#15503 = CARTESIAN_POINT ( 'NONE',  ( 130.8568914410475088, -39.99999999999988631, -34.05028731879802706 ) ) ;
#15504 = AXIS2_PLACEMENT_3D ( 'NONE', #24119, #15589, #7604 ) ;
#15505 = CARTESIAN_POINT ( 'NONE',  ( -208.1127848780264742, -38.89260858015753541, 17.67593391476614784 ) ) ;
#15506 = AXIS2_PLACEMENT_3D ( 'NONE', #878, #5505, #5379 ) ;
#15507 = CARTESIAN_POINT ( 'NONE',  ( -259.2033419157646676, 30.48217210827734647, 2.449293598294708485E-15 ) ) ;
#15508 = ORIENTED_EDGE ( 'NONE', *, *, #2899, .T. ) ;
#15509 = CARTESIAN_POINT ( 'NONE',  ( -259.2033419157646676, 21.55415060305839958, -35.01439189186541512 ) ) ;
#15510 = CARTESIAN_POINT ( 'NONE',  ( 200.0000000000000000, 72.72568232011447265, -59.67546976104962653 ) ) ;
#15511 = CARTESIAN_POINT ( 'NONE',  ( 67.67011021022710793, 12.13550330113689668, 29.29769665552182545 ) ) ;
#15512 = CARTESIAN_POINT ( 'NONE',  ( -5.296937277115072007, -42.80341339122408328, -17.72975434250616544 ) ) ;
#15513 = ORIENTED_EDGE ( 'NONE', *, *, #14530, .T. ) ;
#15514 = DIRECTION ( 'NONE',  ( 0.000000000000000000, -0.3656393565653344724, -0.9307566067079450223 ) ) ;
#15515 = CARTESIAN_POINT ( 'NONE',  ( 200.0000000000001421, -12.54320094651582451, -14.29122475987005458 ) ) ;
#15516 = CARTESIAN_POINT ( 'NONE',  ( 67.90397382975598362, -14.12691053344105541, 28.69135535066940434 ) ) ;
#15517 = CARTESIAN_POINT ( 'NONE',  ( 98.29820294268672853, 19.47931871582185792, 5.235283165533769711 ) ) ;
#15518 = CARTESIAN_POINT ( 'NONE',  ( 199.0058386706367912, 17.79887573832666092, -9.116163937183429766 ) ) ;
#15519 = AXIS2_PLACEMENT_3D ( 'NONE', #6707, #22953, #4865 ) ;
#15520 = CARTESIAN_POINT ( 'NONE',  ( 104.1600437297061319, -20.63676802948826960, 8.548029200615774315 ) ) ;
#15521 = B_SPLINE_CURVE_WITH_KNOTS ( 'NONE', 3,
 ( #248, #8627, #2381, #22346, #10762, #14742, #4256, #22610, #16607, #22873, #6104, #20877 ),
 .UNSPECIFIED., .F., .F.,
 ( 4, 2, 2, 2, 2, 4 ),
 ( 2.860979249076398407E-17, 0.005971652981263952074, 0.008957479471895872167, 0.01045039271721183091, 0.01119684933986976778, 0.01194330596252770292 ),
 .UNSPECIFIED. ) ;
#15522 = CARTESIAN_POINT ( 'NONE',  ( 130.8568914410475088, 40.00000000000002842, 5.949712681206834830 ) ) ;
#15523 = CARTESIAN_POINT ( 'NONE',  ( 146.6084372240433993, 1.478241399363601114E-13, -34.62501878078305850 ) ) ;
#15524 = CYLINDRICAL_SURFACE ( 'NONE', #1955, 30.00000000000000711 ) ;
#15525 = CARTESIAN_POINT ( 'NONE',  ( -100.7734535825088500, 22.67402823373189946, 40.00000000000002132 ) ) ;
#15527 = CARTESIAN_POINT ( 'NONE',  ( -599.0136856033758477, 38.50067712691970456, -10.89074244889556731 ) ) ;
#15526 = CARTESIAN_POINT ( 'NONE',  ( -151.4802930568654062, 16.17241674359067360, -31.86309827670526929 ) ) ;
#15528 = CARTESIAN_POINT ( 'NONE',  ( -280.0000000000000568, 19.99999999999996092, 40.00000000000002132 ) ) ;
#15530 = CARTESIAN_POINT ( 'NONE',  ( 4.995406935893294431, -15.24977328854832415, -40.00000000000002132 ) ) ;
#15529 = CONICAL_SURFACE ( 'NONE', #19792, 20.53474504356812247, 0.7853981633974725929 ) ;
#15531 = CARTESIAN_POINT ( 'NONE',  ( -192.9588430854689989, 14.46834944099965981, 0.000000000000000000 ) ) ;
#15532 = CARTESIAN_POINT ( 'NONE',  ( 14.38125909742180220, 40.00000000000017764, -15.17850393972591760 ) ) ;
#15533 = CARTESIAN_POINT ( 'NONE',  ( 130.8568914410475088, -39.99999999999992895, -5.949712681207114606 ) ) ;
#15534 = CARTESIAN_POINT ( 'NONE',  ( -77.90255099906769942, -20.04994828523962269, 8.644468104261498809 ) ) ;
#15535 = ORIENTED_EDGE ( 'NONE', *, *, #631, .T. ) ;
#15537 = CARTESIAN_POINT ( 'NONE',  ( -4.439300432586643197, 46.85201324744569717, -13.79990882516952055 ) ) ;
#15536 = PLANE ( 'NONE',  #3081 ) ;
#15538 = CARTESIAN_POINT ( 'NONE',  ( -30.26275506840323004, -41.69427246844629309, 40.00000000000002132 ) ) ;
#15539 = CARTESIAN_POINT ( 'NONE',  ( -238.4067589809705794, 0.6820004457912851592, -0.6820004457913123597 ) ) ;
#15540 = CARTESIAN_POINT ( 'NONE',  ( -200.4317933031570078, 44.88237357214676138, -24.83634732651982446 ) ) ;
#15541 =( LENGTH_UNIT ( ) NAMED_UNIT ( * ) SI_UNIT ( .MILLI., .METRE. ) );
#15542 = ORIENTED_EDGE ( 'NONE', *, *, #15241, .F. ) ;
#15543 = VERTEX_POINT ( 'NONE', #17143 ) ;
#15544 = AXIS2_PLACEMENT_3D ( 'NONE', #12226, #24876, #24479 ) ;
#15545 = CARTESIAN_POINT ( 'NONE',  ( -94.58366989427446470, -20.58370269626843907, 9.000605044545363143 ) ) ;
#15546 = LINE ( 'NONE', #7560, #12799 ) ;
#15547 = EDGE_LOOP ( 'NONE', ( #10270, #28 ) ) ;
#15548 = ORIENTED_EDGE ( 'NONE', *, *, #8335, .T. ) ;
#15549 = ORIENTED_EDGE ( 'NONE', *, *, #21663, .T. ) ;
#15550 = CARTESIAN_POINT ( 'NONE',  ( 199.9999999999998010, -4.783743133932452096, 18.39862578376663294 ) ) ;
#15551 = DIRECTION ( 'NONE',  ( 1.000000000000000000, -1.836970198721030181E-16, -0.000000000000000000 ) ) ;
#15552 = EDGE_CURVE ( 'NONE', #15800, #9742, #1306, .T. ) ;
#15553 = CIRCLE ( 'NONE', #17679, 5.000000000000004441 ) ;
#15554 = CARTESIAN_POINT ( 'NONE',  ( 136.1360204305621266, 3.511608612530704665, 3.511608612530695339 ) ) ;
#15555 = LINE ( 'NONE', #15429, #17436 ) ;
#15556 = CARTESIAN_POINT ( 'NONE',  ( -208.1127848780265026, -9.061048840815752106E-14, 15.00245453012669472 ) ) ;
#15557 = FACE_OUTER_BOUND ( 'NONE', #10522, .T. ) ;
#15558 = CARTESIAN_POINT ( 'NONE',  ( -102.2610585947572872, -2.520905002189730703E-13, 22.27377874548543701 ) ) ;
#15559 = EDGE_CURVE ( 'NONE', #23081, #15005, #9155, .T. ) ;
#15560 = CARTESIAN_POINT ( 'NONE',  ( 200.0000000000000000, 72.72568232011447265, -59.67546976104962653 ) ) ;
#15561 = LINE ( 'NONE', #6339, #19600 ) ;
#15562 = CARTESIAN_POINT ( 'NONE',  ( -86.96347745069645896, 40.00000000000019895, -18.24025645688310249 ) ) ;
#15563 = CARTESIAN_POINT ( 'NONE',  ( -114.7824662269369327, -14.65611376398954135, 16.64100530753757567 ) ) ;
#15564 = CARTESIAN_POINT ( 'NONE',  ( -91.56559293963836410, 16.03295912088714203, -16.03295912088699282 ) ) ;
#15565 = CARTESIAN_POINT ( 'NONE',  ( -105.3755690713226727, 5.661656051307470077E-14, -21.75974354311649961 ) ) ;
#15566 = CARTESIAN_POINT ( 'NONE',  ( -135.8532207217289738, 6.472252184284186249, -6.472252184284142729 ) ) ;
#15567 = CARTESIAN_POINT ( 'NONE',  ( 164.1122551457364693, 24.38379312608498850, 10.10009781492419911 ) ) ;
#15568 = ADVANCED_FACE ( 'NONE', ( #15273 ), #26092, .T. ) ;
#15569 = FACE_OUTER_BOUND ( 'NONE', #6136, .T. ) ;
#15570 = CARTESIAN_POINT ( 'NONE',  ( 170.2234770963711128, 17.36149277827004411, -17.36149277826983095 ) ) ;
#15571 = CARTESIAN_POINT ( 'NONE',  ( -56.48582580120558561, -40.00000000000000000, -9.153146818113723882 ) ) ;
#15572 = CARTESIAN_POINT ( 'NONE',  ( -30.26275506840324070, 1.198031551615912571, 57.76657404653985139 ) ) ;
#15573 = CARTESIAN_POINT ( 'NONE',  ( -192.9588430854690273, -66.79921049721887982, -10.23066800229569040 ) ) ;
#15574 = CARTESIAN_POINT ( 'NONE',  ( -661.6652239365027981, 44.75196652329666591, -4.756359218591798665 ) ) ;
#15575 = CARTESIAN_POINT ( 'NONE',  ( -102.2610585947572872, 15.74993999358138907, 15.74993999358168040 ) ) ;
#15576 = ORIENTED_EDGE ( 'NONE', *, *, #24110, .T. ) ;
#15577 = CARTESIAN_POINT ( 'NONE',  ( 19.06497207195980792, 66.60410523465830579, -10.03556273973354251 ) ) ;
#15578 = B_SPLINE_CURVE_WITH_KNOTS ( 'NONE', 3,
 ( #12207, #18319, #4373, #2365, #18593, #14333, #20733, #2501 ),
 .UNSPECIFIED., .F., .F.,
 ( 4, 2, 2, 4 ),
 ( 0.008396560128401207163, 0.01250087472271541912, 0.01455303201987252423, 0.01660518931702962761 ),
 .UNSPECIFIED. ) ;
#15579 = CARTESIAN_POINT ( 'NONE',  ( 170.0000000000000000, 19.80854622259149878, -15.47746304364901171 ) ) ;
#15580 = DIRECTION ( 'NONE',  ( 0.000000000000000000, 0.000000000000000000, -1.000000000000000000 ) ) ;
#15581 = ORIENTED_EDGE ( 'NONE', *, *, #25881, .T. ) ;
#15582 = CARTESIAN_POINT ( 'NONE',  ( 57.59792236341148453, -40.00000000000003553, 2.435789363417741438 ) ) ;
#15583 = CARTESIAN_POINT ( 'NONE',  ( 199.0212986000439059, -19.41582075653976958, -4.984890382579185264 ) ) ;
#15584 = CARTESIAN_POINT ( 'NONE',  ( -199.9999999999999432, 14.17215463606722459, -49.28189405767596298 ) ) ;
#15585 = EDGE_LOOP ( 'NONE', ( #6759, #8090, #7466, #24813 ) ) ;
#15586 = ORIENTED_EDGE ( 'NONE', *, *, #14753, .F. ) ;
#15587 = CARTESIAN_POINT ( 'NONE',  ( -200.4318156386385965, -44.88237417767405191, -24.83634777281914197 ) ) ;
#15588 = CARTESIAN_POINT ( 'NONE',  ( 130.8568914410475088, 40.00000000000002842, 5.949712681206834830 ) ) ;
#15589 = DIRECTION ( 'NONE',  ( 1.000000000000000000, 1.836970198721030181E-16, -0.000000000000000000 ) ) ;
#15590 = CARTESIAN_POINT ( 'NONE',  ( -259.2033419157646676, 21.55415060305860209, -21.55415060305812602 ) ) ;
#15591 = CARTESIAN_POINT ( 'NONE',  ( -100.7734535825088500, -40.00000000000009948, 17.32597176626796909 ) ) ;
#15592 = CARTESIAN_POINT ( 'NONE',  ( 199.9999999999998295, -7.847915761074617080, -17.31000481134407565 ) ) ;
#15593 = CARTESIAN_POINT ( 'NONE',  ( 136.1360204305621266, 1.473277640373554421E-13, -35.03383547441296741 ) ) ;
#15594 = FACE_OUTER_BOUND ( 'NONE', #1753, .T. ) ;
#15595 = CARTESIAN_POINT ( 'NONE',  ( -91.56559293963834989, -16.03295912088728414, 16.03295912088688269 ) ) ;
#15596 = CARTESIAN_POINT ( 'NONE',  ( -135.8532207217289738, 6.472252184284583265, -50.09629031063960980 ) ) ;
#15597 = CARTESIAN_POINT ( 'NONE',  ( -105.2110227778633202, -21.45666521040888597, 1.366831978263496117 ) ) ;
#15598 = CARTESIAN_POINT ( 'NONE',  ( -280.0000000000000000, -2.609240458947769655E-13, 20.00000000000001421 ) ) ;
#15599 = FACE_BOUND ( 'NONE', #7600, .T. ) ;
#15600 = CARTESIAN_POINT ( 'NONE',  ( -135.8532207217289738, 9.153146818113548022, 40.00000000000002132 ) ) ;
#15601 = CARTESIAN_POINT ( 'NONE',  ( 57.59792236341148453, -37.56421063658185489, -40.00000000000002132 ) ) ;
#15602 = CARTESIAN_POINT ( 'NONE',  ( -105.3755690713226727, 15.38646221621793231, -15.38646221621779020 ) ) ;
#15603 = CARTESIAN_POINT ( 'NONE',  ( 200.0000000000000000, 20.00000000000013856, -40.00000000000002132 ) ) ;
#15605 = CYLINDRICAL_SURFACE ( 'NONE', #25904, 5.000000000000095035 ) ;
#15604 = CARTESIAN_POINT ( 'NONE',  ( 151.7948205124836250, -23.49921654116371883, 23.49921654116317526 ) ) ;
#15606 = CARTESIAN_POINT ( 'NONE',  ( 192.4448373802100889, -1.741373372144848397E-13, 20.00000000003942091 ) ) ;
#15607 = CARTESIAN_POINT ( 'NONE',  ( -135.8532207217289738, 50.09629031063965243, -6.472252184284084109 ) ) ;
#15608 = CARTESIAN_POINT ( 'NONE',  ( 192.4448373802101173, 19.99999999996063949, 40.00000000000002132 ) ) ;
#15609 = ORIENTED_EDGE ( 'NONE', *, *, #6710, .T. ) ;
#15610 = EDGE_CURVE ( 'NONE', #12795, #13332, #13897, .T. ) ;
#15611 = CARTESIAN_POINT ( 'NONE',  ( 83.06440094986135136, -24.44702070088743540, 9.006081069514475956 ) ) ;
#15612 = LINE ( 'NONE', #21618, #18052 ) ;
#15613 = CARTESIAN_POINT ( 'NONE',  ( 19.06497207195980792, 66.60410523465817789, 10.03556273973446800 ) ) ;
#15614 = CARTESIAN_POINT ( 'NONE',  ( -135.8532207217289738, -1.351063376314938213E-13, 30.84685318188645553 ) ) ;
#15615 = CARTESIAN_POINT ( 'NONE',  ( -30.26275506840325136, 29.48230279907760121, 27.08623969584625613 ) ) ;
#15616 = EDGE_CURVE ( 'NONE', #21778, #4752, #5022, .T. ) ;
#15617 = CARTESIAN_POINT ( 'NONE',  ( -162.0762913951021176, 1.694272876828294194, -40.00000000000002132 ) ) ;
#15618 = PLANE ( 'NONE',  #23262 ) ;
#15619 = CARTESIAN_POINT ( 'NONE',  ( 199.9999999999998010, -4.783743133932452096, 18.39862578376663294 ) ) ;
#15620 = CARTESIAN_POINT ( 'NONE',  ( 170.0000000000001421, 9.369682556672135121, 22.62041470344889760 ) ) ;
#15621 = CARTESIAN_POINT ( 'NONE',  ( 14.38125909742180752, 10.73282306404735387, -10.73282306404708919 ) ) ;
#15622 = CARTESIAN_POINT ( 'NONE',  ( 91.82158438592156813, 40.45024623143973486, -16.11829626348390931 ) ) ;
#15623 = CARTESIAN_POINT ( 'NONE',  ( 57.59792236341147031, 1.722363176415065089, -1.722363176415036445 ) ) ;
#15624 = CARTESIAN_POINT ( 'NONE',  ( -86.95438060894043986, 9.637778285144355195, -19.12135828296647588 ) ) ;
#15625 = CARTESIAN_POINT ( 'NONE',  ( 184.8905102610680444, 14.79361573936424890, -41.77492675555986068 ) ) ;
#15627 = CARTESIAN_POINT ( 'NONE',  ( 184.8905102610680444, -43.07788698682556827, -13.49065550809859104 ) ) ;
#15626 = CARTESIAN_POINT ( 'NONE',  ( 192.4448373802101173, 42.42640687122089815, -14.14213562370272470 ) ) ;
#15628 = CARTESIAN_POINT ( 'NONE',  ( 0.2972598230769938343, 10.13633138497486286, -10.13633138497461594 ) ) ;
#15629 = CARTESIAN_POINT ( 'NONE',  ( 14.38125909742180752, 15.17850393972634038, 0.000000000000000000 ) ) ;
#15630 = CARTESIAN_POINT ( 'NONE',  ( 190.0000000000000000, -52.49999999999992895, -52.49999999999999289 ) ) ;
#15631 = CARTESIAN_POINT ( 'NONE',  ( 19.06497207195981858, -40.00000000000007105, 14.19242893257826665 ) ) ;
#15632 = CARTESIAN_POINT ( 'NONE',  ( -192.9588430854690273, 18.05360324515418924, 38.51493924976949756 ) ) ;
#15633 = CARTESIAN_POINT ( 'NONE',  ( 184.8905102610680444, -14.79361573936399665, 14.79361573936367158 ) ) ;
#15634 = CARTESIAN_POINT ( 'NONE',  ( 200.0000000000000000, -20.00000000000006750, 40.00000000000002132 ) ) ;
#15635 = ORIENTED_EDGE ( 'NONE', *, *, #20542, .T. ) ;
#15636 = CARTESIAN_POINT ( 'NONE',  ( 19.06497207195979726, 38.31983398719629719, -18.24870850772750686 ) ) ;
#15637 = CARTESIAN_POINT ( 'NONE',  ( 40.56892791155959088, 37.51946456477319458, 15.54107107570585455 ) ) ;
#15638 = DIRECTION ( 'NONE',  ( 0.000000000000000000, 0.000000000000000000, -1.000000000000000000 ) ) ;
#15639 = CARTESIAN_POINT ( 'NONE',  ( -105.2054292635175869, -1.366713675291838737, 21.49321519473981468 ) ) ;
#15640 = ORIENTED_EDGE ( 'NONE', *, *, #12641, .T. ) ;
#15641 = CARTESIAN_POINT ( 'NONE',  ( -189.6939181379304955, -43.50327460064440999, 18.01964634722552461 ) ) ;
#15642 = B_SPLINE_CURVE_WITH_KNOTS ( 'NONE', 3,
 ( #22318, #9530, #16046, #13917, #25781, #22052, #15639, #1830 ),
 .UNSPECIFIED., .F., .F.,
 ( 4, 2, 2, 4 ),
 ( 0.0002291728420604105022, 0.002290361214547608718, 0.004351549587034806744, 0.008473926332009199328 ),
 .UNSPECIFIED. ) ;
#15643 = CARTESIAN_POINT ( 'NONE',  ( 200.0000000000001137, -7.564955314186367907, -17.43543124971759539 ) ) ;
#15644 = CARTESIAN_POINT ( 'NONE',  ( 23.39921416754915739, -23.33452606844846500, 42.84940400815675332 ) ) ;
#15645 = B_SPLINE_CURVE_WITH_KNOTS ( 'NONE', 3,
 ( #22250, #6271, #24241, #4165, #21979, #2158 ),
 .UNSPECIFIED., .F., .F.,
 ( 4, 2, 4 ),
 ( 7.757919228897728493E-18, 0.004202846899763157743, 0.008405693799526306811 ),
 .UNSPECIFIED. ) ;
#15646 = EDGE_CURVE ( 'NONE', #15869, #8765, #11456, .T. ) ;
#15647 = VECTOR ( 'NONE', #1257, 1000.000000000000000 ) ;
#15648 = CARTESIAN_POINT ( 'NONE',  ( 27.79909650598017379, 13.47302921524990538, -45.20561170652695893 ) ) ;
#15649 = CARTESIAN_POINT ( 'NONE',  ( 199.0053213077726753, 13.66600449016087993, -14.61040478752057226 ) ) ;
#15650 = UNCERTAINTY_MEASURE_WITH_UNIT (LENGTH_MEASURE( 1.000000000000000082E-05 ), #4028, 'distance_accuracy_value', 'NONE');
#15651 = CARTESIAN_POINT ( 'NONE',  ( -87.13361725327071383, 21.49321519333427233, 0.6985161928263129427 ) ) ;
#15652 = CARTESIAN_POINT ( 'NONE',  ( -198.0356074513804572, -9.007331120208026888E-14, 15.37879056873070560 ) ) ;
#15653 = DIRECTION ( 'NONE',  ( 0.000000000000000000, 0.000000000000000000, 1.000000000000000000 ) ) ;
#15654 = CARTESIAN_POINT ( 'NONE',  ( -211.2619052429883482, 9.184850993605148733E-15, 75.00000000000000000 ) ) ;
#15655 = CARTESIAN_POINT ( 'NONE',  ( -259.2033419157646676, 9.517827891722582478, 40.00000000000002132 ) ) ;
#15656 = CARTESIAN_POINT ( 'NONE',  ( -596.9857817216397962, 39.99915423894839250, 0.5766869916085746173 ) ) ;
#15657 = CARTESIAN_POINT ( 'NONE',  ( 98.29820294268191105, -7.653668647302824368, -18.47759065022797031 ) ) ;
#15658 = CARTESIAN_POINT ( 'NONE',  ( -100.7734535825088500, -17.32597176626812185, -40.00000000000002132 ) ) ;
#15659 = CARTESIAN_POINT ( 'NONE',  ( 146.6084372240433709, -34.62501878078303008, 40.00000000000002132 ) ) ;
#15660 = CARTESIAN_POINT ( 'NONE',  ( 192.4448373802100889, 2.472897170449861688E-13, -19.99999999996060751 ) ) ;
#15661 = CARTESIAN_POINT ( 'NONE',  ( -100.7734535825088358, -2.560096224687585342E-13, 22.67402823373191723 ) ) ;
#15662 = CARTESIAN_POINT ( 'NONE',  ( 14.38125909742181285, -10.73282306404712472, -10.73282306404731301 ) ) ;
#15663 = ORIENTED_EDGE ( 'NONE', *, *, #11565, .T. ) ;
#15664 = DIRECTION ( 'NONE',  ( 0.000000000000000000, 0.000000000000000000, 1.000000000000000000 ) ) ;
#15665 = CARTESIAN_POINT ( 'NONE',  ( -135.8532207217289738, 9.153146818113546246, -0.000000000000000000 ) ) ;
#15666 = CARTESIAN_POINT ( 'NONE',  ( -4.039451493210489019, 13.82811171175440812, 46.99046209229809534 ) ) ;
#15667 = CARTESIAN_POINT ( 'NONE',  ( -93.01854144616076780, -8.553566904025881712, 20.65013722625350567 ) ) ;
#15668 = DIRECTION ( 'NONE',  ( -1.836970198721030181E-16, 1.000000000000000000, -3.491481338843133355E-15 ) ) ;
#15669 = ORIENTED_EDGE ( 'NONE', *, *, #12307, .T. ) ;
#15670 = VERTEX_POINT ( 'NONE', #13127 ) ;
#15671 = CARTESIAN_POINT ( 'NONE',  ( -91.56559293963836410, 16.03295912088714203, -16.03295912088699282 ) ) ;
#15672 = LINE ( 'NONE', #23304, #8557 ) ;
#15673 = AXIS2_PLACEMENT_3D ( 'NONE', #13674, #17792, #10222 ) ;
#15674 = VERTEX_POINT ( 'NONE', #15747 ) ;
#15675 = CARTESIAN_POINT ( 'NONE',  ( -30.26275506840324425, 1.694272468446254232, -40.00000000000002132 ) ) ;
#15676 = CARTESIAN_POINT ( 'NONE',  ( -100.0957100000493512, -20.56213589465292912, 8.517115558914053253 ) ) ;
#15677 = ORIENTED_EDGE ( 'NONE', *, *, #5971, .F. ) ;
#15678 = CARTESIAN_POINT ( 'NONE',  ( 200.0000000000000568, -10.82911035642265141, 15.62521814345774196 ) ) ;
#15679 = CARTESIAN_POINT ( 'NONE',  ( 190.0000000000000000, -66.50000000000001421, -66.50000000000005684 ) ) ;
#15680 = CARTESIAN_POINT ( 'NONE',  ( 192.4448373802101173, 42.42640687116508502, -14.14213562375874567 ) ) ;
#15681 = DIRECTION ( 'NONE',  ( 0.000000000000000000, -1.000000000000000000, 0.000000000000000000 ) ) ;
#15682 = CARTESIAN_POINT ( 'NONE',  ( -86.96347745069644475, 5.999880687339585546E-14, -21.75974354311649961 ) ) ;
#15683 = CARTESIAN_POINT ( 'NONE',  ( 22.27434459963462388, -13.86259002493217096, 47.22399357567389444 ) ) ;
#15684 = LINE ( 'NONE', #3467, #10248 ) ;
#15685 = DIRECTION ( 'NONE',  ( 0.000000000000000000, 1.000000000000000000, 0.000000000000000000 ) ) ;
#15686 = CARTESIAN_POINT ( 'NONE',  ( 91.82158438592158234, -1.633484621919921769E-13, 17.20528682183300262 ) ) ;
#15687 = CARTESIAN_POINT ( 'NONE',  ( -238.4067589809705794, -3.369206980223063916E-14, -0.9644942799825824142 ) ) ;
#15688 = CARTESIAN_POINT ( 'NONE',  ( -199.9999999999999716, -47.95319408140863260, -15.63350978565342153 ) ) ;
#15689 = CARTESIAN_POINT ( 'NONE',  ( -213.1075012329537230, -9.698598906450557777, 9.698598906450415669 ) ) ;
#15690 = CARTESIAN_POINT ( 'NONE',  ( 163.1118516004056573, 1.251511021549353291E-13, -27.26290988616872824 ) ) ;
#15691 = CARTESIAN_POINT ( 'NONE',  ( 136.1360204305621266, -3.511608612530379592, -53.05693388239318153 ) ) ;
#15692 = CARTESIAN_POINT ( 'NONE',  ( -97.72675010090215153, 8.185591577777120875, 20.89622088363376307 ) ) ;
#15693 = VECTOR ( 'NONE', #23044, 1000.000000000000000 ) ;
#15694 = CARTESIAN_POINT ( 'NONE',  ( -77.59212294118380271, 13.55867551896204937, -17.46520578609249696 ) ) ;
#15695 = CARTESIAN_POINT ( 'NONE',  ( 19.06497207195979726, 40.00000000000017053, -14.19242893257798599 ) ) ;
#15696 = CARTESIAN_POINT ( 'NONE',  ( -238.4067589809705794, -40.00000000000021316, 40.96449427990166470 ) ) ;
#15697 = CARTESIAN_POINT ( 'NONE',  ( 163.1118516004056573, -19.27778845539233998, 37.29075403953149959 ) ) ;
#15698 = CARTESIAN_POINT ( 'NONE',  ( -198.0356074513804572, -10.87444709759714634, -10.87444709759729911 ) ) ;
#15699 = CARTESIAN_POINT ( 'NONE',  ( -629.4336412755042147, 28.28427124746188071, -35.00000000000000000 ) ) ;
#15700 = CARTESIAN_POINT ( 'NONE',  ( -100.7734535825088500, -12.25131212657462498, -44.31723036834905827 ) ) ;
#15701 = ORIENTED_EDGE ( 'NONE', *, *, #1740, .T. ) ;
#15702 = CARTESIAN_POINT ( 'NONE',  ( 184.8905102610680444, 13.49065550809826952, -13.49065550809790359 ) ) ;
#15703 = CARTESIAN_POINT ( 'NONE',  ( -575.0231298121445889, 90.00000000000000000, 29.99999999999825206 ) ) ;
#15704 = CARTESIAN_POINT ( 'NONE',  ( -626.9846540392142060, 28.28427124746186649, 34.99999999999999289 ) ) ;
#15705 = CARTESIAN_POINT ( 'NONE',  ( -30.26275506840324070, 1.198031551616724366, -57.76657404653984429 ) ) ;
#15706 = CARTESIAN_POINT ( 'NONE',  ( -82.28159816621803202, 6.254964767126788949, 19.22531893665605196 ) ) ;
#15707 = ORIENTED_EDGE ( 'NONE', *, *, #23136, .F. ) ;
#15708 = CARTESIAN_POINT ( 'NONE',  ( 200.0000000000000000, 15.11283142964146364, -11.58284877839162519 ) ) ;
#15709 = CARTESIAN_POINT ( 'NONE',  ( 199.0254332542744464, -18.76228886362404324, 6.941650229743832057 ) ) ;
#15710 = CARTESIAN_POINT ( 'NONE',  ( -24.88648382749770605, 12.31763033300769195, 39.69105101992045093 ) ) ;
#15711 = ORIENTED_EDGE ( 'NONE', *, *, #18093, .T. ) ;
#15712 = ORIENTED_EDGE ( 'NONE', *, *, #10207, .T. ) ;
#15713 = CARTESIAN_POINT ( 'NONE',  ( -30.26275506840324425, 41.69427246844628598, -40.00000000000002132 ) ) ;
#15714 = CARTESIAN_POINT ( 'NONE',  ( -208.1127848780265026, -10.60833733269551971, 10.60833733269537049 ) ) ;
#15715 = CARTESIAN_POINT ( 'NONE',  ( -192.9588430854690273, 39.99999999999980105, 54.46834944098235809 ) ) ;
#15716 = CARTESIAN_POINT ( 'NONE',  ( -86.86493150571119770, -19.60045294882755584, -8.366608963954130118 ) ) ;
#15717=STYLED_ITEM('',(#26374),#26128);
#15718 = EDGE_CURVE ( 'NONE', #23054, #20774, #7104, .T. ) ;
#15719 = CARTESIAN_POINT ( 'NONE',  ( -30.26275506840323715, 29.48230279907829754, -29.48230279907758344 ) ) ;
#15720 = SHAPE_REPRESENTATION ( 'Stator', ( #21058 ), #17620 ) ;
#15721 = CARTESIAN_POINT ( 'NONE',  ( -238.4067589809705794, 39.99999999999999289, -0.9644942799821634161 ) ) ;
#15722 = CARTESIAN_POINT ( 'NONE',  ( -210.0000000000000284, -52.49999999999972999, -82.49999999999998579 ) ) ;
#15723 = CARTESIAN_POINT ( 'NONE',  ( 170.2234770963711128, 40.00000000000014211, -24.55285855007172913 ) ) ;
#15724 = CARTESIAN_POINT ( 'NONE',  ( -149.5198336001615189, 31.65188091022390893, 13.11063834760882152 ) ) ;
#15725 = CARTESIAN_POINT ( 'NONE',  ( -0.5869797817569126774, -18.21245090263647981, -43.96874597320456957 ) ) ;
#15726 = CARTESIAN_POINT ( 'NONE',  ( -198.0356074513804572, 17.40982414986501325, -39.15871834505897198 ) ) ;
#15727 = CARTESIAN_POINT ( 'NONE',  ( -315.0000000000000568, -4.857225732735059864E-14, 21.53474504356810115 ) ) ;
#15728 = CARTESIAN_POINT ( 'NONE',  ( -208.1127848780264742, -39.99999999999990763, -15.00245453012711394 ) ) ;
#15729 = CARTESIAN_POINT ( 'NONE',  ( -105.4741150117382773, -19.77569912955116749, -7.943527260750395946 ) ) ;
#15730 = CARTESIAN_POINT ( 'NONE',  ( -86.96347745069645896, 21.75974354311648895, 40.00000000000002132 ) ) ;
#15731 = CARTESIAN_POINT ( 'NONE',  ( 4.995406935893294431, -15.24977328854832415, -40.00000000000002132 ) ) ;
#15732 = CARTESIAN_POINT ( 'NONE',  ( 184.8905102610680444, 43.07788698682572459, 13.49065550809829439 ) ) ;
#15733 = CARTESIAN_POINT ( 'NONE',  ( 136.1360204305621266, 35.03383547441298163, -40.00000000000002132 ) ) ;
#15734 = CARTESIAN_POINT ( 'NONE',  ( -105.4741150117389168, 7.943527260764259523, 19.77569912954497866 ) ) ;
#15735 = CARTESIAN_POINT ( 'NONE',  ( 146.6084372240433993, -3.357462877844280890E-13, 34.62501878078305850 ) ) ;
#15736 = CARTESIAN_POINT ( 'NONE',  ( 91.82158438592158234, 44.40256751092336884, -12.16597498400043342 ) ) ;
#15737 = CARTESIAN_POINT ( 'NONE',  ( 14.38125909742180752, 55.17850393972636880, 2.449293598294708485E-15 ) ) ;
#15738 = ORIENTED_EDGE ( 'NONE', *, *, #12245, .T. ) ;
#15739 = CARTESIAN_POINT ( 'NONE',  ( 98.29820294267354086, -18.47759065023112157, 7.653668647303947914 ) ) ;
#15740 = CARTESIAN_POINT ( 'NONE',  ( 57.59792236341147031, 26.56190807104693619, -30.00663442387692115 ) ) ;
#15741 = CARTESIAN_POINT ( 'NONE',  ( -280.0000000000000000, -1.237140859393462838E-13, 20.00000000000001421 ) ) ;
#15742 = CARTESIAN_POINT ( 'NONE',  ( -198.0356074513804572, 39.15871834505887250, 17.40982414986519089 ) ) ;
#15743 = CARTESIAN_POINT ( 'NONE',  ( 130.8568914410475372, -3.326198072800416995E-13, 34.05028731879788495 ) ) ;
#15744 = AXIS2_PLACEMENT_3D ( 'NONE', #17566, #5600, #5221 ) ;
#15745 = CARTESIAN_POINT ( 'NONE',  ( -198.0356074513804572, 15.37879056873067007, 0.000000000000000000 ) ) ;
#15746 = CIRCLE ( 'NONE', #8112, 20.53474504356812247 ) ;
#15747 = CARTESIAN_POINT ( 'NONE',  ( -87.13361725327075646, -15.19799821270861706, 15.19799821270823159 ) ) ;
#15748 = CARTESIAN_POINT ( 'NONE',  ( 199.9999999999996874, -6.995992324030534171, 17.67857064404661926 ) ) ;
#15749 = CARTESIAN_POINT ( 'NONE',  ( -87.08883489506207809, 3.402281996148261101, -21.20173182216571917 ) ) ;
#15750 = CARTESIAN_POINT ( 'NONE',  ( 136.1360204305621266, -24.77266263493151044, 24.77266263493093135 ) ) ;
#15751 = CARTESIAN_POINT ( 'NONE',  ( 57.59792236341148453, 1.722363176415528940, -54.84617931850878136 ) ) ;
#15752 = CARTESIAN_POINT ( 'NONE',  ( -77.55640685876511498, -22.13135000837103661, -4.964495286674871776E-15 ) ) ;
#15753 = CARTESIAN_POINT ( 'NONE',  ( -87.13348102036110276, 16.17099723932746258, -14.22374190074556033 ) ) ;
#15754 = CARTESIAN_POINT ( 'NONE',  ( -259.2033419157646676, -21.55415060305824326, -21.55415060305857367 ) ) ;
#15756 = CARTESIAN_POINT ( 'NONE',  ( -162.0762913951021176, -27.08623940707584055, -29.48230308784799547 ) ) ;
#15755 = CARTESIAN_POINT ( 'NONE',  ( -30.26275506840322649, -29.48230279907769358, -29.48230279907820162 ) ) ;
#15757 = CARTESIAN_POINT ( 'NONE',  ( 192.4448373802101173, -14.14213562375826605, -42.42640687116518450 ) ) ;
#15758 = CARTESIAN_POINT ( 'NONE',  ( -114.7826396787322665, 2.171560191748074081E-13, -22.13135001986799111 ) ) ;
#15759 = CARTESIAN_POINT ( 'NONE',  ( -370.0000000000001137, -4.857225732735059864E-14, -19.53474504356807273 ) ) ;
#15761 = CARTESIAN_POINT ( 'NONE',  ( 130.8568914410475088, -40.00000000000001421, 5.949712681206549725 ) ) ;
#15760 = CARTESIAN_POINT ( 'NONE',  ( -135.8532207217289738, 50.09629031063956006, 6.472252184284782217 ) ) ;
#15762 = CARTESIAN_POINT ( 'NONE',  ( -259.2033419157646676, 6.730120644403214669, 49.83842185052034068 ) ) ;
#15763 = CARTESIAN_POINT ( 'NONE',  ( -86.96347745069644475, -15.38646221621807442, 15.38646221621768184 ) ) ;
#15764 = AXIS2_PLACEMENT_3D ( 'NONE', #7439, #15551, #23678 ) ;
#15765 = CARTESIAN_POINT ( 'NONE',  ( -208.1127848780264742, 15.00245453012665742, 40.00000000000002132 ) ) ;
#15766 = VERTEX_POINT ( 'NONE', #17748 ) ;
#15767 = CARTESIAN_POINT ( 'NONE',  ( -208.1127848780264742, 38.89260858015732936, -17.67593391476642140 ) ) ;
#15768 = CARTESIAN_POINT ( 'NONE',  ( 91.16600911855444167, 21.07464282850845905, 8.729402881737186704 ) ) ;
#15769 = CARTESIAN_POINT ( 'NONE',  ( 22.86726691379304199, 17.87269271907674195, 43.14849715852160728 ) ) ;
#15770 = CARTESIAN_POINT ( 'NONE',  ( -30.26275506840324425, 1.694272468446254232, 40.00000000000002132 ) ) ;
#15771 = EDGE_LOOP ( 'NONE', ( #9596, #22398 ) ) ;
#15772 = CARTESIAN_POINT ( 'NONE',  ( -192.9370391625990919, -44.11033075278038496, 24.26711063095388710 ) ) ;
#15773 = CARTESIAN_POINT ( 'NONE',  ( 199.9999999999999432, -13.87586802671829211, 12.99819774096606118 ) ) ;
#15774 = CARTESIAN_POINT ( 'NONE',  ( -1.624577210500880220, -18.12534649861199654, 43.75845733969866558 ) ) ;
#15775 = CARTESIAN_POINT ( 'NONE',  ( 22.33254948916862404, 17.93222939140627403, -43.29223140031697170 ) ) ;
#15776 = CARTESIAN_POINT ( 'NONE',  ( 199.0067595892537327, 5.170136663293450674, -19.31817980730454209 ) ) ;
#15777 = VECTOR ( 'NONE', #23790, 1000.000000000000114 ) ;
#15778 = CARTESIAN_POINT ( 'NONE',  ( 126.3230993689412855, -28.30579214049056347, 11.72464299830478218 ) ) ;
#15779 = SPHERICAL_SURFACE ( 'NONE', #23324, 15.00000000000000000 ) ;
#15780 = DIRECTION ( 'NONE',  ( 1.000000000000000000, 1.836970198721030181E-16, -0.000000000000000000 ) ) ;
#15781 = EDGE_CURVE ( 'NONE', #23831, #23552, #13757, .T. ) ;
#15782 = CARTESIAN_POINT ( 'NONE',  ( -162.0762913951020892, 1.198031840456041497, -57.76657433537918251 ) ) ;
#15783 = CARTESIAN_POINT ( 'NONE',  ( -105.3755690713226585, 21.75974354311648185, 40.00000000000002132 ) ) ;
#15785 = CARTESIAN_POINT ( 'NONE',  ( -597.0000841186025582, 39.98842450048364583, 1.092820868205398366 ) ) ;
#15784 = CARTESIAN_POINT ( 'NONE',  ( -151.7004448982690974, 13.46262099571027981, -32.50164219281900557 ) ) ;
#15786 = EDGE_CURVE ( 'NONE', #23734, #25845, #13888, .T. ) ;
#15787 = CARTESIAN_POINT ( 'NONE',  ( -213.1075012329537230, 9.698598906450543566, -9.698598906450348167 ) ) ;
#15788 = CARTESIAN_POINT ( 'NONE',  ( 146.6084372240433709, 34.62501878078307982, -40.00000000000002132 ) ) ;
#15789 = CARTESIAN_POINT ( 'NONE',  ( -208.1127848780264742, 55.00245453014418473, 40.00000000000002132 ) ) ;
#15790 = CARTESIAN_POINT ( 'NONE',  ( 184.8905102610680444, 2.362515690532070066E-13, -19.07866798485558490 ) ) ;
#15791 = CARTESIAN_POINT ( 'NONE',  ( 170.2234770963711128, -2.259079968736224833E-13, 24.55285855007187124 ) ) ;
#15792 = CARTESIAN_POINT ( 'NONE',  ( -192.9588430854690273, 18.05360324515473280, -38.51493924976924177 ) ) ;
#15793 = EDGE_CURVE ( 'NONE', #2915, #10128, #19841, .T. ) ;
#15794 = EDGE_CURVE ( 'NONE', #17327, #60, #18015, .T. ) ;
#15795 = EDGE_LOOP ( 'NONE', ( #22217, #2247 ) ) ;
#15796 = DIRECTION ( 'NONE',  ( 0.000000000000000000, -1.000000000000000000, 0.000000000000000000 ) ) ;
#15797 = CARTESIAN_POINT ( 'NONE',  ( -86.96347745069645896, 21.75974354311648895, -0.000000000000000000 ) ) ;
#15798 = CARTESIAN_POINT ( 'NONE',  ( 170.2234770963711128, -17.36149277827010096, 17.36149277826970660 ) ) ;
#15799 = CARTESIAN_POINT ( 'NONE',  ( -103.9663809734266806, -8.574562934117741619, 19.92521373309844535 ) ) ;
#15800 = VERTEX_POINT ( 'NONE', #1540 ) ;
#15801 = VERTEX_POINT ( 'NONE', #24007 ) ;
#15802 = CARTESIAN_POINT ( 'NONE',  ( 130.8568914410475088, -4.207082182989324792, -52.36146031193423056 ) ) ;
#15803 = CARTESIAN_POINT ( 'NONE',  ( 27.79909650603157090, -45.20561170655300032, -13.47302921519561991 ) ) ;
#15804 = ORIENTED_EDGE ( 'NONE', *, *, #4263, .T. ) ;
#15805 = CARTESIAN_POINT ( 'NONE',  ( -192.9588430854690273, 14.46834944099966336, -40.00000000000002132 ) ) ;
#15806 = CARTESIAN_POINT ( 'NONE',  ( -86.86493150571010347, -19.60045294882735334, 8.366608963953911626 ) ) ;
#15807 = EDGE_LOOP ( 'NONE', ( #1210, #25880, #25433, #4260, #7962, #9442 ) ) ;
#15808 = CARTESIAN_POINT ( 'NONE',  ( 200.0000000000000000, 17.99290950227088004, 6.120759354987654000 ) ) ;
#15809 = CARTESIAN_POINT ( 'NONE',  ( 180.0000000000000000, -35.78896085774750446, 82.49999999999998579 ) ) ;
#15810 = CARTESIAN_POINT ( 'NONE',  ( -135.8532207217289738, 21.81201906317767936, 21.81201906317778239 ) ) ;
#15811 = FACE_OUTER_BOUND ( 'NONE', #12395, .T. ) ;
#15812 = CARTESIAN_POINT ( 'NONE',  ( 192.4448373802100889, 1.051811698935164031E-13, -20.00000000003942091 ) ) ;
#15813 = CARTESIAN_POINT ( 'NONE',  ( -86.96347745069644475, -21.75974354311652093, 40.00000000000002132 ) ) ;
#15814 = CARTESIAN_POINT ( 'NONE',  ( 14.38125909742181463, 10.73282306403652875, -67.30136555895941797 ) ) ;
#15815 = FACE_OUTER_BOUND ( 'NONE', #9093, .T. ) ;
#15816 = PLANE ( 'NONE',  #24586 ) ;
#15817 = CARTESIAN_POINT ( 'NONE',  ( 91.82158438592159655, -39.99999999999976552, -22.79471317813512599 ) ) ;
#15818 = CARTESIAN_POINT ( 'NONE',  ( -110.1003821002711760, -15.15067674037973688, 13.36729751626187301 ) ) ;
#15819 = CARTESIAN_POINT ( 'NONE',  ( 130.8568914410475372, -4.207082182992846420, 4.207082182992822439 ) ) ;
#15820 = CARTESIAN_POINT ( 'NONE',  ( 163.1118516004056573, 27.26290988616875310, 0.000000000000000000 ) ) ;
#15821 = CARTESIAN_POINT ( 'NONE',  ( 170.2234770963711128, -10.92277846919171935, -45.64576402573189995 ) ) ;
#15822 = FACE_OUTER_BOUND ( 'NONE', #4172, .T. ) ;
#15823 = CARTESIAN_POINT ( 'NONE',  ( -3.071327051952942089, -47.32824404903815463, 13.87830843099601275 ) ) ;
#15824 = CARTESIAN_POINT ( 'NONE',  ( -135.8532207217289738, -1.208299557080134822E-13, 9.153146818113572891 ) ) ;
#15825 = CARTESIAN_POINT ( 'NONE',  ( -280.0000000000000568, -40.00000000000000000, -20.00000000000015277 ) ) ;
#15826 = CARTESIAN_POINT ( 'NONE',  ( -238.4067589809705794, 28.96627169325324758, -27.60227080167054581 ) ) ;
#15827 = CARTESIAN_POINT ( 'NONE',  ( -114.7844311315812149, 14.74981244961873728, 16.56244415773397805 ) ) ;
#15828 = CARTESIAN_POINT ( 'NONE',  ( -197.6433718612336747, -18.53520099267758425, -44.74793361791282820 ) ) ;
#15829 = CARTESIAN_POINT ( 'NONE',  ( 151.7948205124836250, 23.49921654116361225, -23.49921654116333514 ) ) ;
#15830 = VERTEX_POINT ( 'NONE', #3527 ) ;
#15831 = CARTESIAN_POINT ( 'NONE',  ( 57.59792236341147031, -1.722363176415055985, 1.722363176415024677 ) ) ;
#15832 = CARTESIAN_POINT ( 'NONE',  ( 170.2234770963711128, 45.64576402573181468, 10.92277846919223627 ) ) ;
#15833 = CARTESIAN_POINT ( 'NONE',  ( 4.995406935893294431, -15.24977328854832415, -40.00000000000002132 ) ) ;
#15834 = DIRECTION ( 'NONE',  ( 0.000000000000000000, 1.000000000000000000, 0.000000000000000000 ) ) ;
#15835 = CARTESIAN_POINT ( 'NONE',  ( 130.8568914410475088, -52.36146031193413108, -4.207082182990267150 ) ) ;
#15836 =( NAMED_UNIT ( * ) PLANE_ANGLE_UNIT ( ) SI_UNIT ( $, .RADIAN. ) );
#15837 = CARTESIAN_POINT ( 'NONE',  ( -77.56353172722820943, 1.385506815401374769, 22.09247646618768712 ) ) ;
#15838 = VERTEX_POINT ( 'NONE', #11628 ) ;
#15839 = CARTESIAN_POINT ( 'NONE',  ( 0.2972598230770030492, -39.99999999999987210, -14.33493731733975451 ) ) ;
#15840 = DIRECTION ( 'NONE',  ( -1.000000000000000000, 0.000000000000000000, 0.000000000000000000 ) ) ;
#15841 = CARTESIAN_POINT ( 'NONE',  ( -5.304449574951913604, 17.72890873421401992, 42.80137191221402304 ) ) ;
#15842 = ORIENTED_EDGE ( 'NONE', *, *, #13368, .F. ) ;
#15843 = VERTEX_POINT ( 'NONE', #11498 ) ;
#15844 = CARTESIAN_POINT ( 'NONE',  ( -192.9588430854690273, 54.46834944098218756, -40.00000000000002132 ) ) ;
#15845 = CARTESIAN_POINT ( 'NONE',  ( -198.9233928134952976, -49.24835219437316169, -14.16707757978289806 ) ) ;
#15846 = CARTESIAN_POINT ( 'NONE',  ( 0.2972598230769883387, 39.99999999999997158, 14.33493731733947563 ) ) ;
#15847 = CARTESIAN_POINT ( 'NONE',  ( -83.21262154144231715, -33.12752917117752105, 13.72187187063024183 ) ) ;
#15848 = CARTESIAN_POINT ( 'NONE',  ( -200.0000000000000284, 82.50000000000008527, 52.49999999999980105 ) ) ;
#15849 = CARTESIAN_POINT ( 'NONE',  ( -135.8532207217289738, -1.208299557080134822E-13, 9.153146818113572891 ) ) ;
#15850 = DIRECTION ( 'NONE',  ( 0.000000000000000000, 1.000000000000000000, 0.000000000000000000 ) ) ;
#15851 = CARTESIAN_POINT ( 'NONE',  ( 199.0207542291320522, 6.104323864361830942, 19.05092312409432154 ) ) ;
#15852 = CARTESIAN_POINT ( 'NONE',  ( 180.0000000000000000, -66.50000000000001421, 66.50000000000005684 ) ) ;
#15853 = CARTESIAN_POINT ( 'NONE',  ( -3.615356597029639296, -17.91804473398299535, -43.25798660799100048 ) ) ;
#15854 = B_SPLINE_CURVE_WITH_KNOTS ( 'NONE', 3,
 ( #15007, #5170, #11390, #23011, #13274, #4911, #21396, #23268, #21520, #4786, #3294, #19264 ),
 .UNSPECIFIED., .F., .F.,
 ( 4, 2, 2, 2, 2, 4 ),
 ( 5.597004042492164534E-17, 0.004680202113614274732, 0.009360404227228492219, 0.01170050528403562135, 0.01404060634084275221, 0.01872080845445705383 ),
 .UNSPECIFIED. ) ;
#15855 = CARTESIAN_POINT ( 'NONE',  ( 130.8568914410475088, -32.49135343045495006, 24.07718906446878648 ) ) ;
#15856 = CARTESIAN_POINT ( 'NONE',  ( 160.7895100361087088, -20.14405787076046295, 20.14405787076000465 ) ) ;
#15857 = CARTESIAN_POINT ( 'NONE',  ( -56.48582580120559982, -21.81201906317755501, -34.75652343174621706 ) ) ;
#15858 = CARTESIAN_POINT ( 'NONE',  ( 192.4448373802101173, -40.00000000000019185, 20.00000000003900524 ) ) ;
#15859 = CARTESIAN_POINT ( 'NONE',  ( 160.9163046357249129, -205.7889608577475542, 55.61140153332249980 ) ) ;
#15860 = CARTESIAN_POINT ( 'NONE',  ( -210.0000000000000284, -52.49999999999992895, -52.49999999999999289 ) ) ;
#15861 = CARTESIAN_POINT ( 'NONE',  ( -56.48582580120558561, -30.84685318188645908, 40.00000000000002132 ) ) ;
#15862 = CARTESIAN_POINT ( 'NONE',  ( 192.4448373802101173, 14.14213562375862665, 42.42640687116509213 ) ) ;
#15863 = CARTESIAN_POINT ( 'NONE',  ( 91.82158438592159655, -22.79471317813468545, -2.449293598294708485E-15 ) ) ;
#15864 = CARTESIAN_POINT ( 'NONE',  ( 18.90082831370066785, -43.99399836018038457, -24.18116416851802342 ) ) ;
#15865 = EDGE_CURVE ( 'NONE', #6051, #12893, #12564, .T. ) ;
#15866 = CARTESIAN_POINT ( 'NONE',  ( -114.4364955367327354, 8.064892380842190178, 20.29001642038852182 ) ) ;
#15867 = CARTESIAN_POINT ( 'NONE',  ( -259.2033419157646676, 21.55415060305830366, 21.55415060305842800 ) ) ;
#15868 = CARTESIAN_POINT ( 'NONE',  ( 130.8568914410475088, -34.05028731879786363, -40.00000000000002132 ) ) ;
#15869 = VERTEX_POINT ( 'NONE', #1806 ) ;
#15870 = CARTESIAN_POINT ( 'NONE',  ( 98.29820294267354086, -18.47759065023111447, 7.653668647303970118 ) ) ;
#15871 = CARTESIAN_POINT ( 'NONE',  ( -199.9999999999998863, -44.86878812508856385, -24.82633483071075986 ) ) ;
#15872 =( BOUNDED_CURVE ( )  B_SPLINE_CURVE ( 3, ( #14541, #22138, #2440, #6819 ),
 .UNSPECIFIED., .F., .T. ) 
 B_SPLINE_CURVE_WITH_KNOTS ( ( 4, 4 ),
 ( 0.007854122480158971450, 0.01576650722537254259 ),
 .UNSPECIFIED. ) 
 CURVE ( )  GEOMETRIC_REPRESENTATION_ITEM ( )  RATIONAL_B_SPLINE_CURVE ( ( 0.9999999999999523714, 0.8893928793063825555, 0.7971366613349984975, 0.7232313460858235121 ) ) 
 REPRESENTATION_ITEM ( '' )  );
#15873 = CARTESIAN_POINT ( 'NONE',  ( 136.1360204305621551, 31.79587985999267374, -24.77266263493117293 ) ) ;
#15874 = CARTESIAN_POINT ( 'NONE',  ( 184.8905102610680444, -40.00000000000005684, 19.07866798485543569 ) ) ;
#15875 = DIRECTION ( 'NONE',  ( 0.000000000000000000, -1.000000000000000000, 0.000000000000000000 ) ) ;
#15876 = CARTESIAN_POINT ( 'NONE',  ( -83.21262154144254453, -13.72187187061479108, 33.12752917118424989 ) ) ;
#15877 = EDGE_CURVE ( 'NONE', #3931, #23238, #25092, .T. ) ;
#15878 = CARTESIAN_POINT ( 'NONE',  ( -192.9588430854689989, 14.46834944099965981, 0.000000000000000000 ) ) ;
#15879 = PRODUCT ( 'Baseplate', 'Baseplate', '', ( #5699 ) ) ;
#15880 = CARTESIAN_POINT ( 'NONE',  ( -370.0000000000001137, -4.857225732735059864E-14, 0.000000000000000000 ) ) ;
#15881 = CARTESIAN_POINT ( 'NONE',  ( 199.9999999999998579, 17.43084440603007224, 7.570815656493459223 ) ) ;
#15882 = EDGE_CURVE ( 'NONE', #4298, #25953, #19775, .T. ) ;
#15883 = CARTESIAN_POINT ( 'NONE',  ( 199.9999999999999147, -16.15527612753063380, 10.03904652186156099 ) ) ;
#15884 = CARTESIAN_POINT ( 'NONE',  ( -213.1075012329537230, 66.26714140138673770, -9.698598906462034819 ) ) ;
#15885 = CARTESIAN_POINT ( 'NONE',  ( 151.7948205124836534, 23.49921654116056047, -33.06932595376338213 ) ) ;
#15886 = CARTESIAN_POINT ( 'NONE',  ( 190.0000000000000000, 7.164183775012018789E-14, 0.000000000000000000 ) ) ;
#15887 = CARTESIAN_POINT ( 'NONE',  ( -82.23724611275160612, 13.84097227486004655, -14.71983334135863508 ) ) ;
#15888 = CARTESIAN_POINT ( 'NONE',  ( 4.995406935893287326, 17.50105314357225694, -39.06748935135176026 ) ) ;
#15890 = CARTESIAN_POINT ( 'NONE',  ( -86.96347745069644475, -15.38646221621807442, 15.38646221621768184 ) ) ;
#15889 = CARTESIAN_POINT ( 'NONE',  ( 151.7948205124836250, -4.785054706301600902, -4.785054706301715477 ) ) ;
#15891 = CARTESIAN_POINT ( 'NONE',  ( 19.06497207195980792, -18.24870850772710540, -38.31983398719647482 ) ) ;
#15892 = CARTESIAN_POINT ( 'NONE',  ( -162.0762913951020892, -1.198031840385783919, 1.198031840385741731 ) ) ;
#15893 = CARTESIAN_POINT ( 'NONE',  ( 199.0255668866977032, -7.539808606132146096, 18.52949269774865471 ) ) ;
#15894 = EDGE_CURVE ( 'NONE', #9227, #19209, #18334, .T. ) ;
#15896 = CARTESIAN_POINT ( 'NONE',  ( -259.2033419157646676, -40.00000000000017764, 30.48217210827725054 ) ) ;
#15895 = CARTESIAN_POINT ( 'NONE',  ( -100.7734535825088500, 12.25131212657428748, 44.31723036834913643 ) ) ;
#15897 = CARTESIAN_POINT ( 'NONE',  ( 4.995406935893287326, 17.50105314357170627, 39.06748935135200895 ) ) ;
#15898 = CARTESIAN_POINT ( 'NONE',  ( 91.82158438592158234, 12.16597498397756993, 12.16597498397776356 ) ) ;
#15899 = CARTESIAN_POINT ( 'NONE',  ( 146.6084372240433709, 5.374981219216996564, 40.00000000000002132 ) ) ;
#15900 = ORIENTED_EDGE ( 'NONE', *, *, #6614, .T. ) ;
#15901 = CARTESIAN_POINT ( 'NONE',  ( 130.8568914410475088, 4.207082182989741348, -52.36146031193420924 ) ) ;
#15902 = CARTESIAN_POINT ( 'NONE',  ( 31.39166500904787327, 40.05004873988723801, 16.58927336176482470 ) ) ;
#15903 = CARTESIAN_POINT ( 'NONE',  ( 27.00968939610489983, 17.38581019149919626, 41.97305875713701084 ) ) ;
#15904 = CARTESIAN_POINT ( 'NONE',  ( -208.1127848780265026, 15.00245453012665564, 0.000000000000000000 ) ) ;
#15905 = ORIENTED_EDGE ( 'NONE', *, *, #16629, .F. ) ;
#15906 = CARTESIAN_POINT ( 'NONE',  ( -198.9234529669416816, -44.84148137680988810, 24.80620787426756735 ) ) ;
#15907 = CARTESIAN_POINT ( 'NONE',  ( 200.0000000000001137, -18.99355687379454949, 0.7833857536329088544 ) ) ;
#15908 = CARTESIAN_POINT ( 'NONE',  ( 20.16956056500655237, -13.95858718337597892, 47.86583268170348759 ) ) ;
#15909 = B_SPLINE_CURVE_WITH_KNOTS ( 'NONE', 3,
 ( #2689, #11053, #10795, #949, #25169, #23168, #6920, #1072 ),
 .UNSPECIFIED., .F., .F.,
 ( 4, 2, 2, 4 ),
 ( 0.008396858476694638723, 0.01250098582284328574, 0.01455304949591760752, 0.01660511316899192930 ),
 .UNSPECIFIED. ) ;
#15910 = CARTESIAN_POINT ( 'NONE',  ( 27.26078259662905268, 17.35591035711511410, -41.90087417141796777 ) ) ;
#15911 = CARTESIAN_POINT ( 'NONE',  ( 199.0161314855084527, -14.37392100214799839, -13.91043101682956973 ) ) ;
#15912 = DIRECTION ( 'NONE',  ( 0.000000000000000000, 0.000000000000000000, -1.000000000000000000 ) ) ;
#15913 = CARTESIAN_POINT ( 'NONE',  ( -129.2920262388371668, -10.46331600586649202, 25.26067940862601091 ) ) ;
#15914 = CARTESIAN_POINT ( 'NONE',  ( 4.995406935893290878, 39.06748935135239265, -39.06748935135144762 ) ) ;
#15915 = CARTESIAN_POINT ( 'NONE',  ( 136.1360204305621266, 35.03383547441298163, 40.00000000000002132 ) ) ;
#15916 = AXIS2_PLACEMENT_3D ( 'NONE', #24816, #12168, #2597 ) ;
#15917 = VECTOR ( 'NONE', #18998, 1000.000000000000000 ) ;
#15919 = CARTESIAN_POINT ( 'NONE',  ( 19.06497207195979726, 38.31983398719604139, 18.24870850772803976 ) ) ;
#15918 = CARTESIAN_POINT ( 'NONE',  ( -716.9846540392142060, -52.49999999999992895, -52.49999999999999289 ) ) ;
#15920 = CARTESIAN_POINT ( 'NONE',  ( 14.38125909742181285, -15.17850393972633505, 0.000000000000000000 ) ) ;
#15921 = CARTESIAN_POINT ( 'NONE',  ( -86.96347745069643054, -18.24025645688353947, -40.00000000000002132 ) ) ;
#15922 = CARTESIAN_POINT ( 'NONE',  ( 136.1360204305621551, -35.03383547441293899, 40.00000000000002132 ) ) ;
#15923 = CARTESIAN_POINT ( 'NONE',  ( 163.1118516004056573, 40.00000000000017764, -12.73709011382432976 ) ) ;
#15924 = CARTESIAN_POINT ( 'NONE',  ( -280.0000000000000000, -2.609240458947769655E-13, 20.00000000000001421 ) ) ;
#15925 = CARTESIAN_POINT ( 'NONE',  ( -213.1075012329537230, -9.698598906450422774, -9.698598906450550672 ) ) ;
#15926 = ORIENTED_EDGE ( 'NONE', *, *, #687, .F. ) ;
#15927 = CARTESIAN_POINT ( 'NONE',  ( -87.01701082927733921, 20.73853774319881538, -5.374668562258758442 ) ) ;
#15928 = CARTESIAN_POINT ( 'NONE',  ( -259.2033419157646676, 9.517827891722584255, -0.000000000000000000 ) ) ;
#15929 = DIRECTION ( 'NONE',  ( 0.000000000000000000, 0.000000000000000000, -1.000000000000000000 ) ) ;
#15930 = APPLICATION_PROTOCOL_DEFINITION ( 'draft international standard', 'automotive_design', 1998, #20471 ) ;
#15931 = ORIENTED_EDGE ( 'NONE', *, *, #24689, .T. ) ;
#15932 = ORIENTED_EDGE ( 'NONE', *, *, #2672, .F. ) ;
#15933 = CARTESIAN_POINT ( 'NONE',  ( 184.8905102610680444, 14.79361573936396113, -14.79361573936377461 ) ) ;
#15934 = CARTESIAN_POINT ( 'NONE',  ( 23.39921416754913253, -42.84940400815667516, -23.33452606844848631 ) ) ;
#15935 = VERTEX_POINT ( 'NONE', #5925 ) ;
#15936 = CARTESIAN_POINT ( 'NONE',  ( -91.56559293963834989, -22.67402823373193499, -40.00000000000002132 ) ) ;
#15937 = CARTESIAN_POINT ( 'NONE',  ( -103.9663809733227282, -20.15238534249515823, 8.026122153668060477 ) ) ;
#15938 = ADVANCED_FACE ( 'NONE', ( #5651, #20157 ), #15618, .F. ) ;
#15939 = EDGE_LOOP ( 'NONE', ( #15905, #9961, #5778, #864 ) ) ;
#15940 = CARTESIAN_POINT ( 'NONE',  ( 200.0000000000000000, 15.44098642598172866, 11.08330662512073950 ) ) ;
#15941 = AXIS2_PLACEMENT_3D ( 'NONE', #4071, #20293, #4731 ) ;
#15942 = CIRCLE ( 'NONE', #4502, 5.000000000000004441 ) ;
#15943 = CARTESIAN_POINT ( 'NONE',  ( 169.9999999999999432, 19.80854622259133890, 15.47746304364925685 ) ) ;
#15944 = CARTESIAN_POINT ( 'NONE',  ( 91.82158438592158234, -12.16597498397761967, -12.16597498397768007 ) ) ;
#15945 = ADVANCED_FACE ( 'NONE', ( #1671 ), #17880, .F. ) ;
#15946 = CARTESIAN_POINT ( 'NONE',  ( -183.1091233172528234, -45.18843800008796308, -13.45963571008054238 ) ) ;
#15947 = CARTESIAN_POINT ( 'NONE',  ( -105.3755690713226585, -40.00000000000010658, 18.24025645688337249 ) ) ;
#15948 = CARTESIAN_POINT ( 'NONE',  ( -208.1127848780264742, 15.00245453012665742, 40.00000000000002132 ) ) ;
#15949 = CARTESIAN_POINT ( 'NONE',  ( 199.9999999999999432, 14.14213562373110911, -14.14213562373072364 ) ) ;
#15950 = CYLINDRICAL_SURFACE ( 'NONE', #14924, 6.000000000000019540 ) ;
#15951 = ADVANCED_FACE ( 'NONE', ( #18151 ), #3398, .T. ) ;
#15952 = EDGE_CURVE ( 'NONE', #19812, #4726, #5824, .T. ) ;
#15953 = CIRCLE ( 'NONE', #22790, 74.99999999999991473 ) ;
#15954 = VECTOR ( 'NONE', #16275, 1000.000000000000000 ) ;
#15955 = CARTESIAN_POINT ( 'NONE',  ( -280.0000000000000568, -40.00000000000000000, -20.00000000000015277 ) ) ;
#15956 = ORIENTED_EDGE ( 'NONE', *, *, #18880, .F. ) ;
#15957 = CARTESIAN_POINT ( 'NONE',  ( -192.9588430854690273, -39.99999999999991473, -14.46834944100011633 ) ) ;
#15958 = CIRCLE ( 'NONE', #6626, 5.000000000000004441 ) ;
#15959 = CARTESIAN_POINT ( 'NONE',  ( -200.0000000000000000, -46.41341197396108953, -18.14835560307970397 ) ) ;
#15960 = CARTESIAN_POINT ( 'NONE',  ( 4.995406935893305977, -39.06748935135212264, 39.06748935135171763 ) ) ;
#15961 = CARTESIAN_POINT ( 'NONE',  ( 146.6084372240433709, 34.62501878078307982, -40.00000000000002132 ) ) ;
#15962 = CARTESIAN_POINT ( 'NONE',  ( 4.995406935893297984, -39.06748935135182421, -17.50105314357212549 ) ) ;
#15963 = CARTESIAN_POINT ( 'NONE',  ( -210.0000000000000284, 57.47694228411666728, -64.52066607436458412 ) ) ;
#15964 = PLANE ( 'NONE',  #19183 ) ;
#15965 = CARTESIAN_POINT ( 'NONE',  ( -259.2033419157646676, 39.99999999999987921, 9.517827891723049660 ) ) ;
#15966 = CARTESIAN_POINT ( 'NONE',  ( 163.1118516004056573, -39.99999999999990052, -27.26290988616886679 ) ) ;
#15967 = CARTESIAN_POINT ( 'NONE',  ( 170.2234770963711128, 39.20704971665398375, -17.36149277826984871 ) ) ;
#15968 = CARTESIAN_POINT ( 'NONE',  ( -56.48582580120559271, 6.472252184284121412, 6.472252184284244869 ) ) ;
#15969 = CARTESIAN_POINT ( 'NONE',  ( -192.1964066537985332, -14.00508515768846252, -48.17614796926347509 ) ) ;
#15970 = CARTESIAN_POINT ( 'NONE',  ( 19.06497207195981147, -10.03556273973439517, 10.03556273973429214 ) ) ;
#15971 = VERTEX_POINT ( 'NONE', #23875 ) ;
#15972 = CARTESIAN_POINT ( 'NONE',  ( -208.1127848780265026, 10.60833733269551615, -10.60833733269529766 ) ) ;
#15973 = CARTESIAN_POINT ( 'NONE',  ( 4.995406935893287326, 17.50105314357170627, 39.06748935135200895 ) ) ;
#15974 = CARTESIAN_POINT ( 'NONE',  ( 180.0000000000000000, -61.50000000000001421, -66.50000000000005684 ) ) ;
#15975 = CARTESIAN_POINT ( 'NONE',  ( 48.46027384457359943, 18.19770403991907415, 35.02097776273673446 ) ) ;
#15976 = CARTESIAN_POINT ( 'NONE',  ( -91.56559293963834989, -16.03295912088659492, -40.53558337403696044 ) ) ;
#15977 = DIRECTION ( 'NONE',  ( 1.000000000000000000, 0.000000000000000000, 0.000000000000000000 ) ) ;
#15978 = CARTESIAN_POINT ( 'NONE',  ( -82.25136756410482519, 3.474794711389625146, 19.89060514491995590 ) ) ;
#15979 = ORIENTED_EDGE ( 'NONE', *, *, #25230, .T. ) ;
#15980 = CARTESIAN_POINT ( 'NONE',  ( 199.9999999999999147, 17.78310516339310254, 6.706406138798904237 ) ) ;
#15981 = FACE_OUTER_BOUND ( 'NONE', #9869, .T. ) ;
#15982 = CARTESIAN_POINT ( 'NONE',  ( -5.152948516938707257, 23.23217004669232111, 42.67688069069163248 ) ) ;
#15983 = AXIS2_PLACEMENT_3D ( 'NONE', #10814, #12940, #2568 ) ;
#15984 = VERTEX_POINT ( 'NONE', #3661 ) ;
#15985 = EDGE_LOOP ( 'NONE', ( #13724, #8971, #10354, #25685, #10669 ) ) ;
#15986 = CARTESIAN_POINT ( 'NONE',  ( -280.0000000000000000, -14.14213562373098831, -14.14213562373098654 ) ) ;
#15987 = CARTESIAN_POINT ( 'NONE',  ( 199.0067595892537327, 5.170136663293450674, -19.31817980730454209 ) ) ;
#15988 = CARTESIAN_POINT ( 'NONE',  ( -110.0574180503309805, 6.256710540492572470, 19.22461201371535822 ) ) ;
#15989 = CARTESIAN_POINT ( 'NONE',  ( -114.6379801953813455, -18.98756686744332001, -11.20591363448406597 ) ) ;
#15990 = AXIS2_PLACEMENT_3D ( 'NONE', #6255, #6379, #269 ) ;
#15991 = EDGE_CURVE ( 'NONE', #21267, #19077, #25656, .T. ) ;
#15992 = DIRECTION ( 'NONE',  ( 0.000000000000000000, -0.7071067811865561215, 0.7071067811865389130 ) ) ;
#15993 = CARTESIAN_POINT ( 'NONE',  ( 192.4448373802100889, -1.741373372144848397E-13, 20.00000000003942091 ) ) ;
#15994 = CARTESIAN_POINT ( 'NONE',  ( 200.0000000000001137, -18.36608873747554327, 4.914565663504686377 ) ) ;
#15995 =( BOUNDED_SURFACE ( )  B_SPLINE_SURFACE ( 3, 2, ( 
 ( #19040, #21171, #6394 ),
 ( #23169, #11054, #16906 ),
 ( #14635, #8661, #6658 ),
 ( #12510, #13053, #14903 ),
 ( #16769, #20638, #12784 ),
 ( #2414, #20911, #18906 ),
 ( #23043, #4818, #8525 ),
 ( #4416, #21037, #8389 ),
 ( #2820, #10929, #819 ),
 ( #8926, #17035, #25170 ),
 ( #6921, #15038, #2944 ),
 ( #16511, #24637, #10523 ),
 ( #18637, #13178, #23296 ),
 ( #16039, #5072, #950 ),
 ( #7301, #15171, #15537 ),
 ( #9307, #11420, #1326 ),
 ( #26184, #3192, #7922 ),
 ( #15415, #17163, #21299 ),
 ( #24165, #23541, #5312 ),
 ( #9182, #11544, #17413 ),
 ( #1204, #15291, #25553 ),
 ( #11301, #19540, #13423 ),
 ( #9431, #5940, #9058 ),
 ( #3448, #3074, #7174 ),
 ( #17538, #23421, #5445 ),
 ( #7422, #14048, #23665 ),
 ( #21546, #19668, #1455 ),
 ( #13546, #3320, #18032 ),
 ( #7056, #21674, #25297 ),
 ( #22182, #11175, #25676 ),
 ( #12053, #19418, #9926 ),
 ( #3955, #5196, #19290 ),
 ( #1073, #17295, #25427 ),
 ( #13299, #21420, #20443 ),
 ( #16575, #26315, #6202 ),
 ( #213, #12583, #22705 ),
 ( #24706, #2088, #18438 ),
 ( #18168, #10062, #24310 ),
 ( #8058, #16705, #20712 ),
 ( #22842, #14313, #2221 ),
 ( #1956, #12447, #24434 ),
 ( #14576, #10195, #6076 ),
 ( #2478, #4481, #10329 ),
 ( #6461, #16174, #22447 ),
 ( #8323, #10590, #18705 ),
 ( #18298, #16447, #4090 ),
 ( #488, #6588, #14178 ),
 ( #8595, #4617, #20575 ),
 ( #85, #4227, #24571 ),
 ( #22313, #24837, #2347 ),
 ( #12316, #12189, #20311 ),
 ( #14710, #8194, #6327 ),
 ( #20173, #16310, #14449 ),
 ( #22576, #4355, #10460 ),
 ( #18572, #352, #8456 ),
 ( #24976, #619, #12713 ),
 ( #16843, #22970, #2616 ),
 ( #18841, #20841, #14837 ),
 ( #8725, #10730, #6725 ),
 ( #8844, #333, #2736 ),
 ( #8574, #18685, #6442 ),
 ( #24684, #2460, #2599 ) ),
 .UNSPECIFIED., .F., .F., .T. ) 
 B_SPLINE_SURFACE_WITH_KNOTS ( ( 4, 2, 2, 2, 2, 2, 2, 2, 2, 2, 2, 2, 2, 2, 2, 2, 2, 2, 2, 2, 2, 2, 2, 2, 2, 2, 2, 2, 2, 2, 4 ),
 ( 3, 3 ),
 ( 0.005118828937694740178, 0.02956064127319283155, 0.05400245360869092293, 0.07844426594418901777, 0.08149949248612628483, 0.08302710575709490448, 0.08379091239257921431, 0.08417281571032136922, 0.08436376736919246055, 0.08445924319862799234, 0.08450698111334575824, 0.08455471902806353801, 0.09066517211193805825, 0.09677562519581259237, 0.09983085173774985943, 0.1028860782796871126, 0.1089965313635616329, 0.1151069844474361670, 0.1181622109893734340, 0.1196898242603420537, 0.1204536308958263635, 0.1208355342135685184, 0.1208594031709274014, 0.1208832721282862843, 0.1209310100430040641, 0.1210264858724396098, 0.1212174375313106872, 0.1273278906151852075, 0.1517697029506832884, 0.1762115152861813971, 0.2006533276216794781 ),
 ( 0.000000000000000000, 1.000000000000000000 ),
 .UNSPECIFIED. ) 
 GEOMETRIC_REPRESENTATION_ITEM ( )  RATIONAL_B_SPLINE_SURFACE ( (
 ( 1.000000000000000000, 0.9997813423572990965, 1.000000000000000000),
 ( 1.000000000000000000, 0.9990919206322235180, 1.000000000000000000),
 ( 1.000000000000000000, 0.9967874177836947291, 1.000000000000000000),
 ( 1.000000000000000000, 0.9887544623284948431, 1.000000000000000000),
 ( 1.000000000000000000, 0.9830290792199358751, 1.000000000000000000),
 ( 1.000000000000000000, 0.9678345454221568556, 1.000000000000000000),
 ( 1.000000000000000000, 0.9583650305405057024, 1.000000000000000000),
 ( 1.000000000000000000, 0.9453335293271457607, 1.000000000000000000),
 ( 1.000000000000000000, 0.9438523872744090104, 1.000000000000000000),
 ( 1.000000000000000000, 0.9415799504612152315, 1.000000000000000000),
 ( 1.000000000000000000, 0.9408140170424226234, 1.000000000000000000),
 ( 1.000000000000000000, 0.9396523143998946059, 1.000000000000000000),
 ( 1.000000000000000000, 0.9392629463989466965, 1.000000000000000000),
 ( 1.000000000000000000, 0.9386756783046048547, 1.000000000000000000),
 ( 1.000000000000000000, 0.9384793862554827726, 1.000000000000000000),
 ( 1.000000000000000000, 0.9381841422086968363, 1.000000000000000000),
 ( 1.000000000000000000, 0.9380855931974630968, 1.000000000000000000),
 ( 1.000000000000000000, 0.9379375679425695500, 1.000000000000000000),
 ( 1.000000000000000000, 0.9378881925679208864, 1.000000000000000000),
 ( 1.000000000000000000, 0.9378140790407644145, 1.000000000000000000),
 ( 1.000000000000000000, 0.9377896949153101680, 1.000000000000000000),
 ( 1.000000000000000000, 0.9377409313169018379, 1.000000000000000000),
 ( 1.000000000000000000, 0.9377165729686782747, 1.000000000000000000),
 ( 1.000000000000000000, 0.9345773786259867766, 1.000000000000000000),
 ( 1.000000000000000000, 0.9318492984274235891, 1.000000000000000000),
 ( 1.000000000000000000, 0.9273872927429864799, 1.000000000000000000),
 ( 1.000000000000000000, 0.9256532593473387749, 1.000000000000000000),
 ( 1.000000000000000000, 0.9239357372749489317, 1.000000000000000000),
 ( 1.000000000000000000, 0.9235102113426452153, 1.000000000000000000),
 ( 1.000000000000000000, 0.9229728558030405594, 1.000000000000000000),
 ( 1.000000000000000000, 0.9228633126625513938, 1.000000000000000000),
 ( 1.000000000000000000, 0.9230139704738934414, 1.000000000000000000),
 ( 1.000000000000000000, 0.9237531682200406102, 1.000000000000000000),
 ( 1.000000000000000000, 0.9264156051934446801, 1.000000000000000000),
 ( 1.000000000000000000, 0.9283388455998538014, 1.000000000000000000),
 ( 1.000000000000000000, 0.9320050037531960596, 1.000000000000000000),
 ( 1.000000000000000000, 0.9333574575349539160, 1.000000000000000000),
 ( 1.000000000000000000, 0.9355411998008593688, 1.000000000000000000),
 ( 1.000000000000000000, 0.9362956009276561797, 1.000000000000000000),
 ( 1.000000000000000000, 0.9374637148016045085, 1.000000000000000000),
 ( 1.000000000000000000, 0.9378591705544803148, 1.000000000000000000),
 ( 1.000000000000000000, 0.9384610703419883349, 1.000000000000000000),
 ( 1.000000000000000000, 0.9386631562400679085, 1.000000000000000000),
 ( 1.000000000000000000, 0.9388793792114360492, 1.000000000000000000),
 ( 1.000000000000000000, 0.9388921037490475241, 1.000000000000000000),
 ( 1.000000000000000000, 0.9389175638858683337, 1.000000000000000000),
 ( 1.000000000000000000, 0.9389305010154731512, 1.000000000000000000),
 ( 1.000000000000000000, 0.9389691441648032599, 1.000000000000000000),
 ( 1.000000000000000000, 0.9389948969011605584, 1.000000000000000000),
 ( 1.000000000000000000, 0.9390721270300055323, 1.000000000000000000),
 ( 1.000000000000000000, 0.9391235763422360883, 1.000000000000000000),
 ( 1.000000000000000000, 0.9392778120326598090, 1.000000000000000000),
 ( 1.000000000000000000, 0.9393804861645954629, 1.000000000000000000),
 ( 1.000000000000000000, 0.9427638002342189072, 1.000000000000000000),
 ( 1.000000000000000000, 0.9458915987232036082, 1.000000000000000000),
 ( 1.000000000000000000, 0.9607963039211067091, 1.000000000000000000),
 ( 1.000000000000000000, 0.9703812854709542579, 1.000000000000000000),
 ( 1.000000000000000000, 0.9854660764533734740, 1.000000000000000000),
 ( 1.000000000000000000, 0.9909632567906729861, 1.000000000000000000),
 ( 1.000000000000000000, 0.9982308762622305043, 1.000000000000000000),
 ( 1.000000000000000000, 0.9999976772054812724, 1.000000000000000000),
 ( 1.000000000000000000, 1.000000000000000000, 1.000000000000000000) ) ) 
 REPRESENTATION_ITEM ( '' )  SURFACE ( )  );
#15996 = CARTESIAN_POINT ( 'NONE',  ( -87.13361725327072804, -21.49321519333431141, -7.703719777548943412E-31 ) ) ;
#15997 = DIRECTION ( 'NONE',  ( 0.000000000000000000, 0.000000000000000000, 1.000000000000000000 ) ) ;
#15998 = CARTESIAN_POINT ( 'NONE',  ( 199.0245441510845410, -3.586860678693493565, 19.68275873856094549 ) ) ;
#15999 = CARTESIAN_POINT ( 'NONE',  ( -181.5938152729462729, 40.59897145788209372, 16.81664459624710162 ) ) ;
#16000 = CARTESIAN_POINT ( 'NONE',  ( 11.38508063393983250, -24.83994849154103690, -44.88728980639532296 ) ) ;
#16001 = CARTESIAN_POINT ( 'NONE',  ( -162.0762913951020892, -29.48230308784744125, -29.48230308784792442 ) ) ;
#16002 = CIRCLE ( 'NONE', #14317, 10.00000000000000888 ) ;
#16003 = CARTESIAN_POINT ( 'NONE',  ( -105.4741150117383057, 7.943527260750631314, -19.77569912955104670 ) ) ;
#16004 = CARTESIAN_POINT ( 'NONE',  ( 170.2234770963711128, -10.92277846919171935, -45.64576402573189995 ) ) ;
#16005 = CARTESIAN_POINT ( 'NONE',  ( 170.2234770963711128, -2.259079968736224833E-13, 24.55285855007187124 ) ) ;
#16006 = CARTESIAN_POINT ( 'NONE',  ( 192.4448373802100889, 20.00000000003945644, 0.000000000000000000 ) ) ;
#16007 = CARTESIAN_POINT ( 'NONE',  ( -56.48582580120557850, -30.84685318188645198, -2.449293598294708485E-15 ) ) ;
#16008 = CARTESIAN_POINT ( 'NONE',  ( -716.9846540392142060, -82.49999999999991473, -52.49999999999977973 ) ) ;
#16009 = CARTESIAN_POINT ( 'NONE',  ( 136.1360204305621266, -4.966164525587039691, -2.449293598294708485E-15 ) ) ;
#16010 = CARTESIAN_POINT ( 'NONE',  ( -110.0700150100807519, 17.57514348718454045, 10.00661953090928691 ) ) ;
#16011 = CARTESIAN_POINT ( 'NONE',  ( 4.995406935893283773, 40.00000000000017764, -15.24977328854790848 ) ) ;
#16012 = CARTESIAN_POINT ( 'NONE',  ( -213.1075012329537230, 37.98287015391236565, -18.58567234101138510 ) ) ;
#16013 = CARTESIAN_POINT ( 'NONE',  ( 192.4448373802101173, 19.99999999996065014, -40.00000000000002132 ) ) ;
#16014 = VERTEX_POINT ( 'NONE', #6183 ) ;
#16015 = CARTESIAN_POINT ( 'NONE',  ( 23.46661716383121288, -46.77475180958801815, 13.79413593526245840 ) ) ;
#16016 = CARTESIAN_POINT ( 'NONE',  ( -199.9999999999999432, -39.01096890182021326, -39.01096890182085986 ) ) ;
#16017 = AXIS2_PLACEMENT_3D ( 'NONE', #14529, #16660, #18654 ) ;
#16018 = CARTESIAN_POINT ( 'NONE',  ( 130.8568914410475088, 4.207082182989741348, -52.36146031193420924 ) ) ;
#16019 = CARTESIAN_POINT ( 'NONE',  ( 57.59792236341149163, -40.00000000000014211, 37.56421063658172699 ) ) ;
#16020 = CARTESIAN_POINT ( 'NONE',  ( 57.59792236341147031, 26.56190807104652052, 30.00663442387728708 ) ) ;
#16021 = CARTESIAN_POINT ( 'NONE',  ( -91.56559293963834989, -22.67402823373193499, 0.000000000000000000 ) ) ;
#16022 = CARTESIAN_POINT ( 'NONE',  ( -86.96347745069644475, -21.75974354311652093, -40.00000000000002132 ) ) ;
#16023 = DIRECTION ( 'NONE',  ( 0.000000000000000000, 0.000000000000000000, 1.000000000000000000 ) ) ;
#16024 = CARTESIAN_POINT ( 'NONE',  ( 200.0000000000000000, 17.99825158093497635, -6.097534595090909448 ) ) ;
#16025 = CARTESIAN_POINT ( 'NONE',  ( 199.9999999999999432, -17.05147999913141277, 8.410089918960904853 ) ) ;
#16026 = CARTESIAN_POINT ( 'NONE',  ( 14.38125909742180397, 67.30136555898270956, -10.73282306405792319 ) ) ;
#16027 = CARTESIAN_POINT ( 'NONE',  ( -91.56559293963834989, -40.53558337403692491, 16.03295912088671571 ) ) ;
#16028 = CARTESIAN_POINT ( 'NONE',  ( -192.1131556193064682, -14.00853984552904485, 48.19965519933757747 ) ) ;
#16029 = CARTESIAN_POINT ( 'NONE',  ( -626.9846540392142060, 90.00000000000000000, 74.99999999999991473 ) ) ;
#16030 = CARTESIAN_POINT ( 'NONE',  ( -208.1127848780264742, -67.17687982760682530, -10.60833733268364298 ) ) ;
#16031 = CARTESIAN_POINT ( 'NONE',  ( -716.9846540392142060, -66.50000000000001421, -66.50000000000005684 ) ) ;
#16032 = CARTESIAN_POINT ( 'NONE',  ( 4.995406935893289102, 10.78321810389013002, -10.78321810388986712 ) ) ;
#16033 = CARTESIAN_POINT ( 'NONE',  ( -56.48582580120559271, 6.472252184284211118, -6.472252184284153387 ) ) ;
#16034 = CARTESIAN_POINT ( 'NONE',  ( 199.0186595897608868, 10.02499462136977115, 17.31996783451393540 ) ) ;
#16036 = CARTESIAN_POINT ( 'NONE',  ( -213.1075012329537230, -40.00000000000011369, 13.71589010951897691 ) ) ;
#16035 = CARTESIAN_POINT ( 'NONE',  ( -30.26275506840324070, 1.198031551616724366, -57.76657404653984429 ) ) ;
#16037 = CARTESIAN_POINT ( 'NONE',  ( 163.1118516004056573, 47.56205970284957374, 9.006482792074494981 ) ) ;
#16038 = CARTESIAN_POINT ( 'NONE',  ( 91.82158438592158234, -12.16597498397778843, 12.16597498397750954 ) ) ;
#16039 = CARTESIAN_POINT ( 'NONE',  ( -4.558244102846631840, 42.85231560262757711, -23.34817229226003832 ) ) ;
#16040 = CARTESIAN_POINT ( 'NONE',  ( -213.1075012329537230, 13.71589010951907817, -40.00000000000002132 ) ) ;
#16041 = ORIENTED_EDGE ( 'NONE', *, *, #24118, .T. ) ;
#16042 = FACE_OUTER_BOUND ( 'NONE', #14779, .T. ) ;
#16043 =( BOUNDED_SURFACE ( )  B_SPLINE_SURFACE ( 3, 3, ( 
 ( #26191, #7930, #6081, #3685, #15904, #21910, #13780, #7788, #11927, #24033, #9801, #11793, #4095, #5946, #9668, #17906, #5812, #23765, #5674, #3550, #14054, #24316, #16180, #12061, #22188, #1696, #3962, #20179, #17638, #20052 ),
 ( #5545, #1961, #20317, #14185, #10068, #18173, #7656, #12195, #26321, #17772, #11651, #19912, #19774, #25915, #15770, #6732, #2225, #2353, #14844, #8462, #2093, #4622, #6466, #10466, #22977, #24842, #14715, #16849, #12721, #14581 ),
 ( #90, #24440, #494, #6207, #22710, #8601, #6332, #14454, #4755, #22582, #4487, #4361, #18442, #20846, #625, #12860, #12588, #24712, #16580, #18578, #20719, #217, #6595, #22847, #24982, #2484, #10597, #18710, #16315, #16710 ),
 ( #2623, #10333, #10202, #10736, #18847, #18304, #8732, #8199, #14319, #22453, #4232, #12321, #20448, #8328, #358, #16452, #24576, #12452, #20579, #5620, #7125, #3623, #7601, #1636, #15106, #7732, #20978, #1504, #25372, #10864 ),
 ( #6991, #15235, #23240, #10999, #13726, #19851, #15844, #23367, #17232, #9120, #21243, #1018, #19108, #25857, #15713, #9745, #5490, #3496, #13590, #8865, #21721, #21851, #11595, #2891, #17845, #25995, #9610, #19716, #892, #18981 ),
 ( #17715, #23840, #23974, #11733, #5750, #2759, #760, #16977, #25113, #6863, #9002, #14979, #23113, #4885, #5016, #13122, #12992, #17106, #21112, #11125, #25238, #3017, #19237, #8269, #22399, #12268, #10402, #8003, #20260, #26267 ),
 ( #16523, #22527, #2168, #24651, #30, #2292, #8141, #2039, #24522, #26124, #4174, #4307, #1904, #11865, #4037, #5886, #17978, #16257, #12136, #18116, #24385, #14260, #6024, #6150, #10142, #20125, #12396, #7866, #10008, #24250 ) ),
 .UNSPECIFIED., .T., .F., .F. ) 
 B_SPLINE_SURFACE_WITH_KNOTS ( ( 4, 3, 4 ),
 ( 4, 2, 2, 2, 2, 2, 2, 2, 2, 2, 2, 2, 2, 2, 4 ),
 ( 0.000000000000000000, 0.5000000000000000000, 1.000000000000000000 ),
 ( 0.000000000000000000, 0.1357259735107005372, 0.1651108541090157700, 0.1944957347073310028, 0.3598804999793158710, 0.3867117631979620773, 0.4135430264166082281, 0.5789277916885930964, 0.6062785021374117456, 0.6336292125862302838, 0.8508620842112317728, 0.8814014469398914198, 0.9119408096685510667, 0.9559704048342755334, 1.000000000000000000 ),
 .UNSPECIFIED. ) 
 GEOMETRIC_REPRESENTATION_ITEM ( )  RATIONAL_B_SPLINE_SURFACE ( (
 ( 1.000000000000000000, 1.000000000000000000, 1.000000000000000000, 1.000000000000000000, 1.000000000000000000, 1.000000000000000000, 1.000000000000000000, 1.000000000000000000, 1.000000000000000000, 1.000000000000000000, 1.000000000000000000, 1.000000000000000000, 1.000000000000000000, 1.000000000000000000, 1.000000000000000000, 1.000000000000000000, 1.000000000000000000, 1.000000000000000000, 1.000000000000000000, 1.000000000000000000, 1.000000000000000000, 1.000000000000000000, 1.000000000000000000, 1.000000000000000000, 1.000000000000000000, 1.000000000000000000, 1.000000000000000000, 1.000000000000000000, 1.000000000000000000, 1.000000000000000000),
 ( 0.3333333333333333703, 0.3333333333333333703, 0.3333333333333333703, 0.3333333333333333703, 0.3333333333333333703, 0.3333333333333333703, 0.3333333333333333703, 0.3333333333333333703, 0.3333333333333333703, 0.3333333333333333703, 0.3333333333333333703, 0.3333333333333333703, 0.3333333333333333703, 0.3333333333333333703, 0.3333333333333333703, 0.3333333333333333703, 0.3333333333333333703, 0.3333333333333333703, 0.3333333333333333703, 0.3333333333333333703, 0.3333333333333333703, 0.3333333333333333703, 0.3333333333333333703, 0.3333333333333333703, 0.3333333333333333703, 0.3333333333333333703, 0.3333333333333333703, 0.3333333333333333703, 0.3333333333333333703, 0.3333333333333333703),
 ( 0.3333333333333333703, 0.3333333333333333703, 0.3333333333333333703, 0.3333333333333333703, 0.3333333333333333703, 0.3333333333333333703, 0.3333333333333333703, 0.3333333333333333703, 0.3333333333333333703, 0.3333333333333333703, 0.3333333333333333703, 0.3333333333333333703, 0.3333333333333333703, 0.3333333333333333703, 0.3333333333333333703, 0.3333333333333333703, 0.3333333333333333703, 0.3333333333333333703, 0.3333333333333333703, 0.3333333333333333703, 0.3333333333333333703, 0.3333333333333333703, 0.3333333333333333703, 0.3333333333333333703, 0.3333333333333333703, 0.3333333333333333703, 0.3333333333333333703, 0.3333333333333333703, 0.3333333333333333703, 0.3333333333333333703),
 ( 1.000000000000000000, 1.000000000000000000, 1.000000000000000000, 1.000000000000000000, 1.000000000000000000, 1.000000000000000000, 1.000000000000000000, 1.000000000000000000, 1.000000000000000000, 1.000000000000000000, 1.000000000000000000, 1.000000000000000000, 1.000000000000000000, 1.000000000000000000, 1.000000000000000000, 1.000000000000000000, 1.000000000000000000, 1.000000000000000000, 1.000000000000000000, 1.000000000000000000, 1.000000000000000000, 1.000000000000000000, 1.000000000000000000, 1.000000000000000000, 1.000000000000000000, 1.000000000000000000, 1.000000000000000000, 1.000000000000000000, 1.000000000000000000, 1.000000000000000000),
 ( 0.3333333333333333703, 0.3333333333333333703, 0.3333333333333333703, 0.3333333333333333703, 0.3333333333333333703, 0.3333333333333333703, 0.3333333333333333703, 0.3333333333333333703, 0.3333333333333333703, 0.3333333333333333703, 0.3333333333333333703, 0.3333333333333333703, 0.3333333333333333703, 0.3333333333333333703, 0.3333333333333333703, 0.3333333333333333703, 0.3333333333333333703, 0.3333333333333333703, 0.3333333333333333703, 0.3333333333333333703, 0.3333333333333333703, 0.3333333333333333703, 0.3333333333333333703, 0.3333333333333333703, 0.3333333333333333703, 0.3333333333333333703, 0.3333333333333333703, 0.3333333333333333703, 0.3333333333333333703, 0.3333333333333333703),
 ( 0.3333333333333333703, 0.3333333333333333703, 0.3333333333333333703, 0.3333333333333333703, 0.3333333333333333703, 0.3333333333333333703, 0.3333333333333333703, 0.3333333333333333703, 0.3333333333333333703, 0.3333333333333333703, 0.3333333333333333703, 0.3333333333333333703, 0.3333333333333333703, 0.3333333333333333703, 0.3333333333333333703, 0.3333333333333333703, 0.3333333333333333703, 0.3333333333333333703, 0.3333333333333333703, 0.3333333333333333703, 0.3333333333333333703, 0.3333333333333333703, 0.3333333333333333703, 0.3333333333333333703, 0.3333333333333333703, 0.3333333333333333703, 0.3333333333333333703, 0.3333333333333333703, 0.3333333333333333703, 0.3333333333333333703),
 ( 1.000000000000000000, 1.000000000000000000, 1.000000000000000000, 1.000000000000000000, 1.000000000000000000, 1.000000000000000000, 1.000000000000000000, 1.000000000000000000, 1.000000000000000000, 1.000000000000000000, 1.000000000000000000, 1.000000000000000000, 1.000000000000000000, 1.000000000000000000, 1.000000000000000000, 1.000000000000000000, 1.000000000000000000, 1.000000000000000000, 1.000000000000000000, 1.000000000000000000, 1.000000000000000000, 1.000000000000000000, 1.000000000000000000, 1.000000000000000000, 1.000000000000000000, 1.000000000000000000, 1.000000000000000000, 1.000000000000000000, 1.000000000000000000, 1.000000000000000000) ) ) 
 REPRESENTATION_ITEM ( '' )  SURFACE ( )  );
#16044 = CARTESIAN_POINT ( 'NONE',  ( 190.0000000000000000, 52.49999999999987210, -82.49999999999998579 ) ) ;
#16045 = CARTESIAN_POINT ( 'NONE',  ( 200.0000000000000000, 72.72568232011447265, -59.67546976104962653 ) ) ;
#16046 = CARTESIAN_POINT ( 'NONE',  ( -105.3895334812053193, -6.678845697753541089, 20.30817960291332369 ) ) ;
#16047 = ORIENTED_EDGE ( 'NONE', *, *, #19519, .F. ) ;
#16048 = CARTESIAN_POINT ( 'NONE',  ( -188.9524464571102556, -43.19209889639846978, 23.58788642769247090 ) ) ;
#16049 = CARTESIAN_POINT ( 'NONE',  ( 200.0000000000002558, -14.49689853580991539, 12.29876589910006857 ) ) ;
#16050 = CARTESIAN_POINT ( 'NONE',  ( 6.984886629847075312, -14.16808340396305255, 49.25486234615101466 ) ) ;
#16051 = EDGE_CURVE ( 'NONE', #61, #7472, #10091, .T. ) ;
#16052 = EDGE_CURVE ( 'NONE', #22053, #13885, #16832, .T. ) ;
#16053 = CARTESIAN_POINT ( 'NONE',  ( 22.72611120194095236, 17.88893075486401329, -43.18769924474474919 ) ) ;
#16054 = CARTESIAN_POINT ( 'NONE',  ( 199.0101504891794946, -4.065683697617192394, -19.58013257009994135 ) ) ;
#16055 = DIRECTION ( 'NONE',  ( 0.000000000000000000, 1.000000000000000000, 0.000000000000000000 ) ) ;
#16056 = CARTESIAN_POINT ( 'NONE',  ( -187.7699188115425102, -23.34606611631818751, 42.84915433766021664 ) ) ;
#16057 = CARTESIAN_POINT ( 'NONE',  ( 14.38125909742180397, 67.30136555898270956, -10.73282306405792319 ) ) ;
#16058 = CARTESIAN_POINT ( 'NONE',  ( 200.0000000000000000, 20.00000000000013856, 40.00000000000002132 ) ) ;
#16060 = CARTESIAN_POINT ( 'NONE',  ( 4.995406935893289102, 10.78321810389013002, -10.78321810388986712 ) ) ;
#16059 = CARTESIAN_POINT ( 'NONE',  ( -188.3120606736140417, 13.82878088495430191, -46.99497558484331705 ) ) ;
#16061 = CARTESIAN_POINT ( 'NONE',  ( -348.0000000000001137, -4.857225732735059864E-14, 0.000000000000000000 ) ) ;
#16062 = CARTESIAN_POINT ( 'NONE',  ( 130.8568914410475372, 34.05028731879791337, 0.000000000000000000 ) ) ;
#16063 = CARTESIAN_POINT ( 'NONE',  ( -280.0000000000000568, -20.00000000000006750, 40.00000000000002132 ) ) ;
#16064 = CARTESIAN_POINT ( 'NONE',  ( 199.9999999999999432, 2.486775779033024914E-13, -19.99999999999992539 ) ) ;
#16065 = CARTESIAN_POINT ( 'NONE',  ( -238.4067589809705794, 57.25054294077225592, 0.6820004458485544596 ) ) ;
#16066 = DIRECTION ( 'NONE',  ( -1.000000000000000000, -1.836970198721030181E-16, 0.000000000000000000 ) ) ;
#16067 = CARTESIAN_POINT ( 'NONE',  ( 146.6084372240433709, 52.76785682606523409, -3.800685668858194255 ) ) ;
#16068 = ORIENTED_EDGE ( 'NONE', *, *, #18683, .F. ) ;
#16069 = CARTESIAN_POINT ( 'NONE',  ( 4.995406935893294431, -17.50105314357198694, 39.06748935135188816 ) ) ;
#16070 = CARTESIAN_POINT ( 'NONE',  ( -238.4067589809705794, -0.9644942799826262680, 0.000000000000000000 ) ) ;
#16071 = CARTESIAN_POINT ( 'NONE',  ( -105.4741150117391300, -8.366608964594041353, 19.60045294982699460 ) ) ;
#16072 = CONTEXT_DEPENDENT_SHAPE_REPRESENTATION ( #23460, #18687 ) ;
#16073 = VERTEX_POINT ( 'NONE', #4339 ) ;
#16074 = ORIENTED_EDGE ( 'NONE', *, *, #21445, .T. ) ;
#16075 = CARTESIAN_POINT ( 'NONE',  ( 170.2234770963711128, -10.92277846919171935, -45.64576402573189995 ) ) ;
#16076 = CARTESIAN_POINT ( 'NONE',  ( 23.10188454848739070, -46.91040837923751639, -13.81611343686933502 ) ) ;
#16077 = ORIENTED_EDGE ( 'NONE', *, *, #20019, .T. ) ;
#16078 = CARTESIAN_POINT ( 'NONE',  ( 184.8905102610680444, 19.07866798485562398, -40.00000000000002132 ) ) ;
#16079 = CARTESIAN_POINT ( 'NONE',  ( -88.38011430172180383, -20.03522014374173210, 8.298859908482608461 ) ) ;
#16080 = AXIS2_PLACEMENT_3D ( 'NONE', #6545, #13196, #25059 ) ;
#16081 = ORIENTED_EDGE ( 'NONE', *, *, #2836, .F. ) ;
#16082 = CARTESIAN_POINT ( 'NONE',  ( 199.9999999999998295, 10.02997355460652429, 16.14748021227288532 ) ) ;
#16083 = CARTESIAN_POINT ( 'NONE',  ( -109.1264249741454933, -33.12752917269487796, -13.72187187123350327 ) ) ;
#16084 = CARTESIAN_POINT ( 'NONE',  ( 146.6084372240433993, -24.48358557860319706, -24.48358557860330720 ) ) ;
#16085 = CARTESIAN_POINT ( 'NONE',  ( -188.3120606736019340, -43.00889065702904190, -23.45204117844409453 ) ) ;
#16086 = CARTESIAN_POINT ( 'NONE',  ( 200.0000000000000000, -40.00000000000005684, 19.99999999999978328 ) ) ;
#16087 = CARTESIAN_POINT ( 'NONE',  ( -213.1075012329537230, 53.71589010953660193, 40.00000000000002132 ) ) ;
#16088 = CARTESIAN_POINT ( 'NONE',  ( 136.1360204305621551, -24.77266263493081766, -31.79587985999290112 ) ) ;
#16089 = CARTESIAN_POINT ( 'NONE',  ( 199.0227319893622848, 1.617020328492027259, 19.94056979940310015 ) ) ;
#16090 = CARTESIAN_POINT ( 'NONE',  ( -162.0762913951020892, -3.568845385355699554E-14, 1.694272876828323948 ) ) ;
#16091 = CARTESIAN_POINT ( 'NONE',  ( 200.0000000000000000, -39.99999999999991473, -20.00000000000024514 ) ) ;
#16092 = CARTESIAN_POINT ( 'NONE',  ( -192.9588430854689989, 1.161019517985663313E-13, -14.46834944099969533 ) ) ;
#16093 = CARTESIAN_POINT ( 'NONE',  ( -200.0000000000000000, -47.13392792189006286, -16.85576820966595335 ) ) ;
#16094 = CARTESIAN_POINT ( 'NONE',  ( 136.1360204305621551, -31.79587985999244282, -24.77266263493140386 ) ) ;
#16095 = CARTESIAN_POINT ( 'NONE',  ( -192.9588430854689989, -14.46834944099973086, 0.000000000000000000 ) ) ;
#16096 = CARTESIAN_POINT ( 'NONE',  ( 57.59792236341147031, -26.56190807104670171, -30.00663442387710234 ) ) ;
#16097 = CARTESIAN_POINT ( 'NONE',  ( -210.0000000000000284, 61.50000000000009237, -66.50000000000005684 ) ) ;
#16098 = CARTESIAN_POINT ( 'NONE',  ( 21.99343714674520811, -47.30053030063386643, 13.87412077874992278 ) ) ;
#16099 = CARTESIAN_POINT ( 'NONE',  ( 116.7964245048539169, 19.78678521258989065, 19.78678521259021039 ) ) ;
#16100 = CARTESIAN_POINT ( 'NONE',  ( -192.9588430854690273, -40.00000000000011369, 14.46834944099955855 ) ) ;
#16101 = CARTESIAN_POINT ( 'NONE',  ( 19.06497207195979726, 38.31983398719629719, -18.24870850772750686 ) ) ;
#16102 = CARTESIAN_POINT ( 'NONE',  ( 184.8905102610680444, 14.79361573936375507, 14.79361573936398067 ) ) ;
#16103 = CARTESIAN_POINT ( 'NONE',  ( -188.9524938556044162, -23.58789616778188147, -43.19211203807876132 ) ) ;
#16104 = CARTESIAN_POINT ( 'NONE',  ( -213.1075012329537230, -37.98287015391232302, -18.58567234101164800 ) ) ;
#16105 = ORIENTED_EDGE ( 'NONE', *, *, #7189, .T. ) ;
#16106 = CIRCLE ( 'NONE', #1303, 5.000000000000004441 ) ;
#16107 = CARTESIAN_POINT ( 'NONE',  ( -162.0762913951021176, -27.08623940707584055, -29.48230308784799547 ) ) ;
#16108 = EDGE_CURVE ( 'NONE', #19940, #11892, #1117, .T. ) ;
#16109 = CARTESIAN_POINT ( 'NONE',  ( 98.29820294267871361, -20.00000000000369837, 2.581272653893885938 ) ) ;
#16110 = CARTESIAN_POINT ( 'NONE',  ( 146.6084372240433993, 34.62501878078308692, 0.000000000000000000 ) ) ;
#16111 = DIRECTION ( 'NONE',  ( -1.000000000000000000, 0.000000000000000000, -0.000000000000000000 ) ) ;
#16112 = CARTESIAN_POINT ( 'NONE',  ( 184.8905102610680444, -14.79361573936330565, -41.77492675556016621 ) ) ;
#16113 = CARTESIAN_POINT ( 'NONE',  ( -90.07798792367798058, 22.27377874500493604, -0.000000000000000000 ) ) ;
#16114 = ORIENTED_EDGE ( 'NONE', *, *, #17515, .F. ) ;
#16115 = CARTESIAN_POINT ( 'NONE',  ( 199.9999999999999147, 18.88155072364786591, -2.150913467935055223 ) ) ;
#16116 = CYLINDRICAL_SURFACE ( 'NONE', #18753, 5.000000000000018652 ) ;
#16117 = CARTESIAN_POINT ( 'NONE',  ( -4.915070467883093208, 13.76630780994167580, 46.68718905934800034 ) ) ;
#16118 = EDGE_LOOP ( 'NONE', ( #4687, #6148, #8224, #14287 ) ) ;
#16119 = ORIENTED_EDGE ( 'NONE', *, *, #23402, .T. ) ;
#16120 = CARTESIAN_POINT ( 'NONE',  ( -208.1127848780265026, 10.60833733269537049, 10.60833733269544510 ) ) ;
#16121 = CARTESIAN_POINT ( 'NONE',  ( 199.0100048860339541, -3.743224330709818748, -19.64425440907078269 ) ) ;
#16122 = CARTESIAN_POINT ( 'NONE',  ( -105.2502192156942868, 3.402547493085597896, 21.20168261175021129 ) ) ;
#16123 = CARTESIAN_POINT ( 'NONE',  ( -198.0356074513804572, 10.87444709759714989, 10.87444709759722450 ) ) ;
#16124 = DIRECTION ( 'NONE',  ( -1.000000000000000000, -0.000000000000000000, -0.000000000000000000 ) ) ;
#16125 = CIRCLE ( 'NONE', #16989, 74.99999999999991473 ) ;
#16126 = CARTESIAN_POINT ( 'NONE',  ( -280.0000000000000000, -2.609240458947769655E-13, 20.00000000000001421 ) ) ;
#16127 = CARTESIAN_POINT ( 'NONE',  ( 200.0000000000003411, -18.28334586770733594, 5.214203034309022655 ) ) ;
#16128 = DIRECTION ( 'NONE',  ( 0.000000000000000000, 1.000000000000000000, 0.000000000000000000 ) ) ;
#16129 = DIRECTION ( 'NONE',  ( 0.000000000000000000, 1.000000000000000000, 0.000000000000000000 ) ) ;
#16130 = CARTESIAN_POINT ( 'NONE',  ( 199.0232347278000873, 0.3099713519423794028, 20.00382596759649800 ) ) ;
#16131 = CARTESIAN_POINT ( 'NONE',  ( -186.9957605999037753, 41.92394832788998826, 17.36546798563979976 ) ) ;
#16132 = CARTESIAN_POINT ( 'NONE',  ( -3.993758944536758726, -13.83056263162038135, -47.00698038897023423 ) ) ;
#16133 = CARTESIAN_POINT ( 'NONE',  ( -86.96347745069643054, -41.18208027870611687, 15.38646221621750954 ) ) ;
#16134 = EDGE_CURVE ( 'NONE', #24474, #5318, #16689, .T. ) ;
#16135 = CARTESIAN_POINT ( 'NONE',  ( -114.7826396787322238, 2.131776515495821831E-13, -22.13135001986798400 ) ) ;
#16136 = CARTESIAN_POINT ( 'NONE',  ( 4.995406935893305977, -39.06748935135212264, 39.06748935135171763 ) ) ;
#16137 = CARTESIAN_POINT ( 'NONE',  ( 130.8568914410475372, -3.326198072800416995E-13, 34.05028731879788495 ) ) ;
#16138 = CARTESIAN_POINT ( 'NONE',  ( -259.2033419157646676, 35.01439189186559275, -21.55415060305807984 ) ) ;
#16139 = APPLICATION_CONTEXT ( 'automotive_design' ) ;
#16140 = CARTESIAN_POINT ( 'NONE',  ( 130.8568914410475372, -5.949712681206667853, -2.449293598294708485E-15 ) ) ;
#16141 = EDGE_CURVE ( 'NONE', #2818, #9561, #6059, .T. ) ;
#16142 = CARTESIAN_POINT ( 'NONE',  ( 151.7948205124836534, -6.767089262349000656, -40.00000000000002132 ) ) ;
#16143 = CARTESIAN_POINT ( 'NONE',  ( -105.2709636321762616, 17.75029751208181139, 12.04384390868683496 ) ) ;
#16144 = CARTESIAN_POINT ( 'NONE',  ( -238.4067589809705794, 3.877349844572403567E-13, -40.96449427998260973 ) ) ;
#16145 = EDGE_CURVE ( 'NONE', #21989, #9701, #604, .T. ) ;
#16146 = CARTESIAN_POINT ( 'NONE',  ( -162.0762913951020892, 1.198031840385716418, 1.198031840385750169 ) ) ;
#16147 = EDGE_CURVE ( 'NONE', #6279, #15935, #314, .T. ) ;
#16148 = CARTESIAN_POINT ( 'NONE',  ( -30.26275506840324425, 1.694272468446254232, -40.00000000000002132 ) ) ;
#16149 = ORIENTED_EDGE ( 'NONE', *, *, #18004, .F. ) ;
#16150 = AXIS2_PLACEMENT_3D ( 'NONE', #21041, #19043, #20779 ) ;
#16151 = ORIENTED_EDGE ( 'NONE', *, *, #12049, .F. ) ;
#16152 = CARTESIAN_POINT ( 'NONE',  ( 57.59792236341147031, -2.435789363418150000, 40.00000000000002132 ) ) ;
#16153 = FILL_AREA_STYLE_COLOUR ( '', #14252 ) ;
#16154 = CARTESIAN_POINT ( 'NONE',  ( -100.7734535825088358, -8.145438380286941744E-14, 17.32597176626811120 ) ) ;
#16155 = CARTESIAN_POINT ( 'NONE',  ( -259.2033419157646676, 21.55415060305790931, 35.01439189186571355 ) ) ;
#16156 = CARTESIAN_POINT ( 'NONE',  ( 91.82158438592158234, -17.20528682183298486, 0.000000000000000000 ) ) ;
#16157 = CARTESIAN_POINT ( 'NONE',  ( -188.2995950289364373, 13.82811170417284075, -46.99046209955416487 ) ) ;
#16158 = CARTESIAN_POINT ( 'NONE',  ( 170.0000000000000000, 24.25569233607185282, -6.285860131565223163 ) ) ;
#16159 = CARTESIAN_POINT ( 'NONE',  ( 200.0000000000002842, 18.39723030902092660, -4.753359243483134655 ) ) ;
#16160 = CARTESIAN_POINT ( 'NONE',  ( 199.9999999999999432, -14.49604467618470593, -12.29544462711038832 ) ) ;
#16161 = CARTESIAN_POINT ( 'NONE',  ( 146.6084372240433993, 3.800685668858732935, -3.800685668858610367 ) ) ;
#16162 = CARTESIAN_POINT ( 'NONE',  ( 91.82158438592159655, -44.40256751092341858, 12.16597498400012434 ) ) ;
#16163 = CIRCLE ( 'NONE', #21273, 5.000000000000004441 ) ;
#16164 = DIRECTION ( 'NONE',  ( 0.000000000000000000, 0.000000000000000000, 1.000000000000000000 ) ) ;
#16165 = CARTESIAN_POINT ( 'NONE',  ( -82.24432634623720162, 12.38461122507612089, -15.96101146153671912 ) ) ;
#16166 = CARTESIAN_POINT ( 'NONE',  ( 163.1118516004056573, -9.006482792069506971, -9.006482792069697041 ) ) ;
#16167 = CARTESIAN_POINT ( 'NONE',  ( -65.65550967526027648, 9.107276986624018633, 24.89650881518432968 ) ) ;
#16168 = CARTESIAN_POINT ( 'NONE',  ( 200.0000000000000000, -42.42640687119272513, -14.14213562373140753 ) ) ;
#16169 = CARTESIAN_POINT ( 'NONE',  ( 192.4448373802100889, 14.14213562375893574, -14.14213562375874922 ) ) ;
#16170 = CARTESIAN_POINT ( 'NONE',  ( 199.0250287384835985, -5.300309701115731187, 19.29992413559400788 ) ) ;
#16172 = CARTESIAN_POINT ( 'NONE',  ( 151.7948205124836534, 40.00000000000002842, 6.767089262349174739 ) ) ;
#16171 = CARTESIAN_POINT ( 'NONE',  ( 91.82158438592158234, 16.11829626346161604, -16.11829626346121103 ) ) ;
#16173 = CARTESIAN_POINT ( 'NONE',  ( -208.1127848780264742, 67.17687982763172272, -10.60833733270698254 ) ) ;
#16174 = CARTESIAN_POINT ( 'NONE',  ( 22.75856136761854387, 43.17893233522199381, -17.88529938203877379 ) ) ;
#16175 = CARTESIAN_POINT ( 'NONE',  ( 91.82158438592158234, 22.79471317813472453, -40.00000000000002132 ) ) ;
#16176 = EDGE_LOOP ( 'NONE', ( #2321, #7307 ) ) ;
#16177 = CARTESIAN_POINT ( 'NONE',  ( 199.9999999999999432, -14.14213562373096345, -14.14213562373104871 ) ) ;
#16178 = CARTESIAN_POINT ( 'NONE',  ( -47.65341557551126073, -29.74088027401770518, 14.80716566690741409 ) ) ;
#16179 = CIRCLE ( 'NONE', #14493, 4.999999999999962697 ) ;
#16180 = CARTESIAN_POINT ( 'NONE',  ( 136.1360204305621266, -35.03383547441293899, 0.000000000000000000 ) ) ;
#16181 = EDGE_LOOP ( 'NONE', ( #21805, #10139, #20123, #7789 ) ) ;
#16182 = CARTESIAN_POINT ( 'NONE',  ( -188.9266304146012203, -43.31220791188976449, 17.94050393342803673 ) ) ;
#16183 = AXIS2_PLACEMENT_3D ( 'NONE', #2405, #8652, #10515 ) ;
#16184 = VECTOR ( 'NONE', #17001, 1000.000000000000000 ) ;
#16185 = TOROIDAL_SURFACE ( 'NONE', #18310, 46.18033988749894547, 15.00000000000000000 ) ;
#16186 = CARTESIAN_POINT ( 'NONE',  ( 200.0000000000000284, -17.94985894478863386, -6.254032569489808679 ) ) ;
#16187 = CARTESIAN_POINT ( 'NONE',  ( 20.16956056503475736, -23.97604322319281422, 43.71646652951534406 ) ) ;
#16188 = CARTESIAN_POINT ( 'NONE',  ( 22.37977766478910979, 13.85469381971835290, -47.17011059971203224 ) ) ;
#16189 = CARTESIAN_POINT ( 'NONE',  ( 199.0103724725597658, -4.548822225537863417, -19.47368150598642345 ) ) ;
#16190 = CARTESIAN_POINT ( 'NONE',  ( -91.56559293963834989, -2.543181659092656077E-13, 22.67402823373191723 ) ) ;
#16191 = CARTESIAN_POINT ( 'NONE',  ( 133.2080217031554525, -29.90338805389125199, 12.38638889282714928 ) ) ;
#16192 = CARTESIAN_POINT ( 'NONE',  ( -114.4364955367308454, -8.644468109209068274, 20.04994829327590011 ) ) ;
#16193 = CARTESIAN_POINT ( 'NONE',  ( 170.2234770963711128, 10.92277846919216522, -10.92277846919186501 ) ) ;
#16194 = CARTESIAN_POINT ( 'NONE',  ( 151.7948205124836250, 33.23291073765556547, 0.000000000000000000 ) ) ;
#16195 = CIRCLE ( 'NONE', #1779, 15.00000000000000178 ) ;
#16197 = CARTESIAN_POINT ( 'NONE',  ( -30.26275506840324070, 1.198031551616030033, -1.198031551616006496 ) ) ;
#16196 = CARTESIAN_POINT ( 'NONE',  ( -190.7346372394923151, 13.94676542150583742, -47.78727444208931274 ) ) ;
#16198 = CARTESIAN_POINT ( 'NONE',  ( 14.38125909742182884, -55.17850393972636169, -2.449293598294708485E-15 ) ) ;
#16199 = CIRCLE ( 'NONE', #4758, 14.99999999999999645 ) ;
#16200 = CARTESIAN_POINT ( 'NONE',  ( 192.4448373802101173, 19.99999999996063949, 40.00000000000002132 ) ) ;
#16201 = CARTESIAN_POINT ( 'NONE',  ( 200.0000000000000000, 40.00000000000026290, -19.99999999999950617 ) ) ;
#16202 = CARTESIAN_POINT ( 'NONE',  ( 192.4448373802101173, -14.14213562375886291, 42.42640687116498555 ) ) ;
#16203 =( BOUNDED_SURFACE ( )  B_SPLINE_SURFACE ( 3, 3, ( 
 ( #14703, #25102, #613, #8719, #18970, #22963, #20966, #2747, #750, #21101, #18697, #8854, #14568, #25227, #23228, #6851, #18565, #2881, #10989, #6980, #20567, #344, #8448, #22698, #4473, #12573, #10581, #17221, #1261, #17351 ),
 ( #7616, #23602, #25487, #15357, #5507, #25359, #5381, #9110, #1522, #13486, #3380, #7236, #7114, #5133, #19351, #1393, #15731, #19735, #17731, #23481, #5006, #11111, #15225, #1007, #11358, #23356, #3005, #21737, #13238, #13608 ),
 ( #19607, #21607, #13357, #15473, #11479, #9494, #3513, #5253, #11613, #25872, #19474, #21232, #21361, #7490, #17599, #25738, #13111, #19227, #3130, #15601, #21479, #3254, #11233, #1140, #9244, #9365, #17475, #7363, #25617, #23726 ),
 ( #9628, #1920, #18135, #16274, #48, #13878, #2057, #5769, #22142, #12285, #21867, #13741, #1653, #16007, #11884, #9762, #23856, #8161, #179, #9894, #24133, #16140, #5634, #24270, #1790, #17862, #6169, #18266, #22011, #26013 ),
 ( #5905, #7749, #2188, #8286, #26284, #3643, #10025, #8023, #24403, #22416, #4054, #20004, #6043, #15861, #14013, #17998, #23990, #20142, #26142, #3780, #18403, #11750, #10296, #4192, #7886, #20413, #3924, #12022, #14148, #22280 ),
 ( #12155, #20278, #10163, #14279, #19869, #852, #4848, #2856, #8560, #16412, #22544, #2312, #12415, #22808, #18538, #14414, #6824, #10421, #16938, #320, #24540, #20945, #4585, #6296, #25073, #10698, #23077, #8421, #12954, #12544 ),
 ( #4324, #20541, #18943, #8696, #2723, #16542, #24672, #6428, #723, #24806, #6558, #10964, #22676, #14546, #16675, #14672, #4449, #12682, #20812, #20676, #589, #2445, #10557, #18669, #24944, #456, #18809, #2583, #19071, #16807 ) ),
 .UNSPECIFIED., .T., .F., .F. ) 
 B_SPLINE_SURFACE_WITH_KNOTS ( ( 4, 3, 4 ),
 ( 4, 2, 2, 2, 2, 2, 2, 2, 2, 2, 2, 2, 2, 2, 4 ),
 ( 0.000000000000000000, 0.5000000000000000000, 1.000000000000000000 ),
 ( 0.000000000000000000, 0.1357259735107005372, 0.1651108541090157700, 0.1944957347073310028, 0.3598804999793158710, 0.3867117631979620773, 0.4135430264166082281, 0.5789277916885930964, 0.6062785021374117456, 0.6336292125862302838, 0.8508620842112317728, 0.8814014469398914198, 0.9119408096685510667, 0.9559704048342755334, 1.000000000000000000 ),
 .UNSPECIFIED. ) 
 GEOMETRIC_REPRESENTATION_ITEM ( )  RATIONAL_B_SPLINE_SURFACE ( (
 ( 1.000000000000000000, 1.000000000000000000, 1.000000000000000000, 1.000000000000000000, 1.000000000000000000, 1.000000000000000000, 1.000000000000000000, 1.000000000000000000, 1.000000000000000000, 1.000000000000000000, 1.000000000000000000, 1.000000000000000000, 1.000000000000000000, 1.000000000000000000, 1.000000000000000000, 1.000000000000000000, 1.000000000000000000, 1.000000000000000000, 1.000000000000000000, 1.000000000000000000, 1.000000000000000000, 1.000000000000000000, 1.000000000000000000, 1.000000000000000000, 1.000000000000000000, 1.000000000000000000, 1.000000000000000000, 1.000000000000000000, 1.000000000000000000, 1.000000000000000000),
 ( 0.3333333333333333703, 0.3333333333333333703, 0.3333333333333333703, 0.3333333333333333703, 0.3333333333333333703, 0.3333333333333333703, 0.3333333333333333703, 0.3333333333333333703, 0.3333333333333333703, 0.3333333333333333703, 0.3333333333333333703, 0.3333333333333333703, 0.3333333333333333703, 0.3333333333333333703, 0.3333333333333333703, 0.3333333333333333703, 0.3333333333333333703, 0.3333333333333333703, 0.3333333333333333703, 0.3333333333333333703, 0.3333333333333333703, 0.3333333333333333703, 0.3333333333333333703, 0.3333333333333333703, 0.3333333333333333703, 0.3333333333333333703, 0.3333333333333333703, 0.3333333333333333703, 0.3333333333333333703, 0.3333333333333333703),
 ( 0.3333333333333333703, 0.3333333333333333703, 0.3333333333333333703, 0.3333333333333333703, 0.3333333333333333703, 0.3333333333333333703, 0.3333333333333333703, 0.3333333333333333703, 0.3333333333333333703, 0.3333333333333333703, 0.3333333333333333703, 0.3333333333333333703, 0.3333333333333333703, 0.3333333333333333703, 0.3333333333333333703, 0.3333333333333333703, 0.3333333333333333703, 0.3333333333333333703, 0.3333333333333333703, 0.3333333333333333703, 0.3333333333333333703, 0.3333333333333333703, 0.3333333333333333703, 0.3333333333333333703, 0.3333333333333333703, 0.3333333333333333703, 0.3333333333333333703, 0.3333333333333333703, 0.3333333333333333703, 0.3333333333333333703),
 ( 1.000000000000000000, 1.000000000000000000, 1.000000000000000000, 1.000000000000000000, 1.000000000000000000, 1.000000000000000000, 1.000000000000000000, 1.000000000000000000, 1.000000000000000000, 1.000000000000000000, 1.000000000000000000, 1.000000000000000000, 1.000000000000000000, 1.000000000000000000, 1.000000000000000000, 1.000000000000000000, 1.000000000000000000, 1.000000000000000000, 1.000000000000000000, 1.000000000000000000, 1.000000000000000000, 1.000000000000000000, 1.000000000000000000, 1.000000000000000000, 1.000000000000000000, 1.000000000000000000, 1.000000000000000000, 1.000000000000000000, 1.000000000000000000, 1.000000000000000000),
 ( 0.3333333333333333703, 0.3333333333333333703, 0.3333333333333333703, 0.3333333333333333703, 0.3333333333333333703, 0.3333333333333333703, 0.3333333333333333703, 0.3333333333333333703, 0.3333333333333333703, 0.3333333333333333703, 0.3333333333333333703, 0.3333333333333333703, 0.3333333333333333703, 0.3333333333333333703, 0.3333333333333333703, 0.3333333333333333703, 0.3333333333333333703, 0.3333333333333333703, 0.3333333333333333703, 0.3333333333333333703, 0.3333333333333333703, 0.3333333333333333703, 0.3333333333333333703, 0.3333333333333333703, 0.3333333333333333703, 0.3333333333333333703, 0.3333333333333333703, 0.3333333333333333703, 0.3333333333333333703, 0.3333333333333333703),
 ( 0.3333333333333333703, 0.3333333333333333703, 0.3333333333333333703, 0.3333333333333333703, 0.3333333333333333703, 0.3333333333333333703, 0.3333333333333333703, 0.3333333333333333703, 0.3333333333333333703, 0.3333333333333333703, 0.3333333333333333703, 0.3333333333333333703, 0.3333333333333333703, 0.3333333333333333703, 0.3333333333333333703, 0.3333333333333333703, 0.3333333333333333703, 0.3333333333333333703, 0.3333333333333333703, 0.3333333333333333703, 0.3333333333333333703, 0.3333333333333333703, 0.3333333333333333703, 0.3333333333333333703, 0.3333333333333333703, 0.3333333333333333703, 0.3333333333333333703, 0.3333333333333333703, 0.3333333333333333703, 0.3333333333333333703),
 ( 1.000000000000000000, 1.000000000000000000, 1.000000000000000000, 1.000000000000000000, 1.000000000000000000, 1.000000000000000000, 1.000000000000000000, 1.000000000000000000, 1.000000000000000000, 1.000000000000000000, 1.000000000000000000, 1.000000000000000000, 1.000000000000000000, 1.000000000000000000, 1.000000000000000000, 1.000000000000000000, 1.000000000000000000, 1.000000000000000000, 1.000000000000000000, 1.000000000000000000, 1.000000000000000000, 1.000000000000000000, 1.000000000000000000, 1.000000000000000000, 1.000000000000000000, 1.000000000000000000, 1.000000000000000000, 1.000000000000000000, 1.000000000000000000, 1.000000000000000000) ) ) 
 REPRESENTATION_ITEM ( '' )  SURFACE ( )  );
#16204 = CARTESIAN_POINT ( 'NONE',  ( 160.9163046357249129, -135.7889608577475542, 61.61140153332250691 ) ) ;
#16205 = CARTESIAN_POINT ( 'NONE',  ( 136.1360204305621266, 24.77266263493104148, 24.77266263493145004 ) ) ;
#16206 = EDGE_LOOP ( 'NONE', ( #18196, #329, #6931, #25776 ) ) ;
#16207 = B_SPLINE_CURVE_WITH_KNOTS ( 'NONE', 3,
 ( #2986, #2729, #10834, #18950, #24952, #731, #595, #6699, #8566, #16680, #8836, #25079, #16944, #4456, #6830, #4591, #6433, #23208, #13095, #24811, #12550, #19208, #12960, #21079, #20682, #10971, #14812, #19080, #860, #8969, #17078, #25212, #6960, #990, #15077, #22814, #4989, #21213, #2452, #2590, #18815, #6563, #14680, #11092, #16547, #12688, #24677, #14551, #22681, #10562, #18675, #461, #20818, #10705, #7468, #25853, #23834, #17710, #23707, #19847, #21587, #15211, #15334, #7097, #25596, #3358, #23582, #9348, #13339, #1500, #23338, #23463, #5114, #7343, #13219, #5234, #21340, #15583, #5616, #7597, #11589, #17202, #3111, #9095, #25340, #1243, #5359, #11340, #11216, #11460, #19330, #13722, #17456, #17580, #7218, #3618, #15709, #9224, #21847, #3235, #25716, #21460, #11729, #13466, #21714, #5486, #9473, #19711 ),
 .UNSPECIFIED., .F., .F.,
 ( 4, 2, 2, 2, 1, 1, 1, 2, 2, 2, 2, 2, 1, 1, 1, 1, 2, 2, 2, 2, 2, 1, 1, 1, 1, 1, 1, 2, 2, 2, 2, 2, 2, 2, 1, 2, 2, 2, 2, 2, 2, 1, 1, 1, 1, 1, 2, 2, 2, 2, 2, 1, 1, 1, 1, 2, 2, 2, 2, 2, 1, 1, 1, 2, 2, 2, 4 ),
 ( 0.5000000000000000000, 0.5312500000000124345, 0.5468750000000187628, 0.5546875000000218714, 0.5585937500000235367, 0.5605468750000243139, 0.5615234375000246470, 0.5620117187500248690, 0.5625000000000250910, 0.5937500000000373035, 0.6093750000000434097, 0.6171875000000464073, 0.6210937500000479616, 0.6230468750000487388, 0.6240234375000490719, 0.6245117187500492939, 0.6247558593750494049, 0.6250000000000495159, 0.6562500000000617284, 0.6718750000000678346, 0.6796875000000708322, 0.6835937500000723865, 0.6855468750000731637, 0.6865234375000734968, 0.6870117187500737188, 0.6872558593750738298, 0.6873779296875738298, 0.6874389648438239409, 0.6875000000000739409, 0.7031250000000741629, 0.7187500000000744960, 0.7343750000000748290, 0.7421875000000749401, 0.7460937500000750511, 0.7480468750000750511, 0.7490234375000750511, 0.7500000000000750511, 0.7656250000000757172, 0.7812500000000763833, 0.7968750000000770495, 0.8046875000000772715, 0.8085937500000774936, 0.8105468750000776046, 0.8115234375000776046, 0.8120117187500776046, 0.8122558593750776046, 0.8123779296875774936, 0.8125000000000774936, 0.8437500000000639488, 0.8593750000000570655, 0.8671875000000537348, 0.8710937500000519584, 0.8730468750000510703, 0.8740234375000506262, 0.8745117187500504041, 0.8747558593750504041, 0.8750000000000501821, 0.9062500000000366374, 0.9218750000000297540, 0.9296875000000264233, 0.9335937500000248690, 0.9355468750000239808, 0.9365234375000235367, 0.9370117187500233147, 0.9375000000000230926, 0.9687500000000115463, 1.000000000000000000 ),
 .UNSPECIFIED. ) ;
#16208 = CARTESIAN_POINT ( 'NONE',  ( -96.94475454966692496, -9.001119816639596038, 20.58449551010044587 ) ) ;
#16209 = APPLICATION_PROTOCOL_DEFINITION ( 'draft international standard', 'automotive_design', 1998, #21093 ) ;
#16210 = EDGE_LOOP ( 'NONE', ( #14746, #10673, #890, #15677 ) ) ;
#16211 = EDGE_LOOP ( 'NONE', ( #22780, #2090, #8833, #20519 ) ) ;
#16212 = CARTESIAN_POINT ( 'NONE',  ( 146.6084372240433709, -32.08495691632041513, -24.48358557860343154 ) ) ;
#16213 = CARTESIAN_POINT ( 'NONE',  ( 22.92196489051161024, -46.97629733300992427, -13.82589419143533327 ) ) ;
#16214 = ORIENTED_EDGE ( 'NONE', *, *, #24600, .F. ) ;
#16215 = CARTESIAN_POINT ( 'NONE',  ( -208.1127848780265026, 15.00245453012665564, 0.000000000000000000 ) ) ;
#16216 = CARTESIAN_POINT ( 'NONE',  ( -96.94475454971259865, -20.92018922313259921, 8.190683501837476399 ) ) ;
#16217 = VERTEX_POINT ( 'NONE', #14560 ) ;
#16218 = CARTESIAN_POINT ( 'NONE',  ( 199.9999999999999432, 3.548988777896260771, 18.67457114543681485 ) ) ;
#16219 = CIRCLE ( 'NONE', #23024, 46.18033988749894547 ) ;
#16220 = CYLINDRICAL_SURFACE ( 'NONE', #24726, 5.000000000000004441 ) ;
#16221 = B_SPLINE_CURVE_WITH_KNOTS ( 'NONE', 3,
 ( #5797, #18291, #22304, #77, #10054, #14306, #20165, #10322 ),
 .UNSPECIFIED., .F., .F.,
 ( 4, 2, 2, 4 ),
 ( 0.0002282271112602323728, 0.004312542793977438421, 0.006354700635336038572, 0.008396858476694638723 ),
 .UNSPECIFIED. ) ;
#16222 = CARTESIAN_POINT ( 'NONE',  ( -192.9588430854690273, 38.51493924976939098, -18.05360324515436687 ) ) ;
#16223 = CARTESIAN_POINT ( 'NONE',  ( -144.1957134274819907, -30.13185274855893780, -12.48102206796960267 ) ) ;
#16224 = CARTESIAN_POINT ( 'NONE',  ( -280.0000000000000568, -40.00000000000014211, 19.99999999999987210 ) ) ;
#16225 = CARTESIAN_POINT ( 'NONE',  ( -238.4067589809705794, 0.9644942799825385604, 40.00000000000002132 ) ) ;
#16226 = CARTESIAN_POINT ( 'NONE',  ( 200.0000000000000000, -14.14213562373046784, -42.42640687119298804 ) ) ;
#16227 = CARTESIAN_POINT ( 'NONE',  ( 192.4448373802100889, 1.051811698935164031E-13, -20.00000000003942091 ) ) ;
#16228 = CARTESIAN_POINT ( 'NONE',  ( -162.0762913951020892, -1.777970010055771463E-13, 41.69427287682835015 ) ) ;
#16229 = CARTESIAN_POINT ( 'NONE',  ( 151.7948205124836534, -40.00000000000034817, 33.23291073765511072 ) ) ;
#16230 = CARTESIAN_POINT ( 'NONE',  ( 184.8905102610680444, 39.99999999999999289, 19.07866798485573057 ) ) ;
#16231 = DIRECTION ( 'NONE',  ( 0.000000000000000000, 1.000000000000000000, 0.000000000000000000 ) ) ;
#16232 = CARTESIAN_POINT ( 'NONE',  ( -192.9588430854689705, -38.51493924976963967, 38.51493924976919914 ) ) ;
#16233 = CARTESIAN_POINT ( 'NONE',  ( 130.8568914410475088, 34.05028731879790627, -40.00000000000002132 ) ) ;
#16234 = EDGE_CURVE ( 'NONE', #21773, #9962, #11697, .T. ) ;
#16235 = CARTESIAN_POINT ( 'NONE',  ( -280.0000000000000568, -14.14213562373078226, -42.42640687119295251 ) ) ;
#16236 = CARTESIAN_POINT ( 'NONE',  ( -678.9461782662789346, 75.00000000000000000, -34.99999999999845812 ) ) ;
#16237 = CARTESIAN_POINT ( 'NONE',  ( 18.89824444022308114, -48.20791849611961766, 14.00990882958429751 ) ) ;
#16238 = CARTESIAN_POINT ( 'NONE',  ( 4.995406935893290878, 1.606505379428369110E-13, -15.24977328854832592 ) ) ;
#16239 = CARTESIAN_POINT ( 'NONE',  ( -238.4067589809705794, 39.99999999999983658, 40.96449428006354765 ) ) ;
#16240 = CARTESIAN_POINT ( 'NONE',  ( -86.96347745069644475, 41.18208027870598187, -15.38646221621779731 ) ) ;
#16241 = CARTESIAN_POINT ( 'NONE',  ( 57.59792236341147031, -26.56190807104712448, 30.00663442387673285 ) ) ;
#16242 = CARTESIAN_POINT ( 'NONE',  ( -192.9370379451513884, -14.03127537977493411, -48.35015161800508565 ) ) ;
#16243 = CARTESIAN_POINT ( 'NONE',  ( 57.59792236341147031, 1.722363176415065089, -1.722363176415036445 ) ) ;
#16244 = EDGE_LOOP ( 'NONE', ( #15576, #8223 ) ) ;
#16245 = CARTESIAN_POINT ( 'NONE',  ( -208.1127848780264742, -17.67593391476605547, -38.89260858015755673 ) ) ;
#16246 = CARTESIAN_POINT ( 'NONE',  ( 98.29820294270304259, -18.47759065022024672, 7.653668647299475047 ) ) ;
#16247 = CARTESIAN_POINT ( 'NONE',  ( -86.96347745069645896, 21.75974354311648895, -0.000000000000000000 ) ) ;
#16248 =( NAMED_UNIT ( * ) PLANE_ANGLE_UNIT ( ) SI_UNIT ( $, .RADIAN. ) );
#16249 = CARTESIAN_POINT ( 'NONE',  ( 14.38125909742181463, 10.73282306403652875, -67.30136555895941797 ) ) ;
#16250 = CARTESIAN_POINT ( 'NONE',  ( -77.55640685876512919, -9.396736996787159758E-14, 22.13135000837102595 ) ) ;
#16251 = ORIENTED_EDGE ( 'NONE', *, *, #2256, .T. ) ;
#16252 = CARTESIAN_POINT ( 'NONE',  ( 199.9999999999999716, 18.27648386272512226, -5.205167537210750872 ) ) ;
#16253 = CARTESIAN_POINT ( 'NONE',  ( 23.30631261065773430, -23.35506702541406554, 42.87793822514953490 ) ) ;
#16254 = CARTESIAN_POINT ( 'NONE',  ( -3.524834090819536137, 17.92814044289615794, 43.28235980537024830 ) ) ;
#16255 = VERTEX_POINT ( 'NONE', #14163 ) ;
#16256 = VERTEX_POINT ( 'NONE', #10314 ) ;
#16257 = CARTESIAN_POINT ( 'NONE',  ( 14.38125909742180752, 15.17850393972634038, 0.000000000000000000 ) ) ;
#16258 = CARTESIAN_POINT ( 'NONE',  ( 199.0078145870362221, 1.786107411569149317, -19.91668635079984284 ) ) ;
#16259 = CARTESIAN_POINT ( 'NONE',  ( -210.0000000000000000, -82.49999999999991473, -52.49999999999977973 ) ) ;
#16260 = FACE_OUTER_BOUND ( 'NONE', #11299, .T. ) ;
#16261 = CARTESIAN_POINT ( 'NONE',  ( 19.06497207195979726, 40.00000000000017053, -14.19242893257798599 ) ) ;
#16262 = B_SPLINE_CURVE_WITH_KNOTS ( 'NONE', 3,
 ( #6999, #18590, #14724, #21125, #22856, #2901, #12734, #20729 ),
 .UNSPECIFIED., .F., .F.,
 ( 4, 2, 2, 4 ),
 ( 0.0002278873370240370642, 0.004309043385737469124, 0.006349621410094185778, 0.008390199434450903299 ),
 .UNSPECIFIED. ) ;
#16263 = CARTESIAN_POINT ( 'NONE',  ( 199.9999999999999432, -13.66164182518334691, 13.22314710892283074 ) ) ;
#16264 = CARTESIAN_POINT ( 'NONE',  ( -652.2876273073196671, 36.60715735981532504, 16.14560165132014191 ) ) ;
#16265 = DIRECTION ( 'NONE',  ( 1.000000000000000000, -1.836970198721030181E-16, -0.000000000000000000 ) ) ;
#16266 = CARTESIAN_POINT ( 'NONE',  ( 199.0186810464772691, 9.993108295904475469, 17.32680936265314386 ) ) ;
#16267 = CYLINDRICAL_SURFACE ( 'NONE', #22823, 5.000000000000004441 ) ;
#16268 = CARTESIAN_POINT ( 'NONE',  ( 12.96694272559235195, -14.15914421027394354, -49.19577900140984639 ) ) ;
#16269 = CARTESIAN_POINT ( 'NONE',  ( -259.2033419157646676, -49.83842185052040463, 6.730120644403092101 ) ) ;
#16270 = CARTESIAN_POINT ( 'NONE',  ( -110.1017833366170748, 9.975556358476777704E-14, -20.19517362627949453 ) ) ;
#16271 = CARTESIAN_POINT ( 'NONE',  ( -86.96347745069643054, -41.18208027870589660, -15.38646221621809040 ) ) ;
#16272 = CARTESIAN_POINT ( 'NONE',  ( -77.92915424793434909, 20.15198149301296482, 8.347224043097730473 ) ) ;
#16273 = CARTESIAN_POINT ( 'NONE',  ( -56.48582580120559271, 6.472252184284121412, 6.472252184284244869 ) ) ;
#16274 = CARTESIAN_POINT ( 'NONE',  ( -213.1075012329536946, -53.71589010951918652, -2.449293598294708485E-15 ) ) ;
#16275 = DIRECTION ( 'NONE',  ( 0.000000000000000000, 1.000000000000000000, 0.000000000000000000 ) ) ;
#16276 = CARTESIAN_POINT ( 'NONE',  ( 192.4448373802100889, -19.99999999996057198, -2.449293598294708485E-15 ) ) ;
#16277 = CARTESIAN_POINT ( 'NONE',  ( -626.9846540392142060, 90.00000000000000000, 0.000000000000000000 ) ) ;
#16278 = ADVANCED_BREP_SHAPE_REPRESENTATION ( '', ( #26128, #21058 ), #4064 ) ;
#16279 = CARTESIAN_POINT ( 'NONE',  ( -198.0356074513804572, 5.461327841961909642E-13, -55.37879056873073580 ) ) ;
#16280 = CARTESIAN_POINT ( 'NONE',  ( 163.1118516004056573, -19.27778845538761132, -19.27778845538770724 ) ) ;
#16281 = CARTESIAN_POINT ( 'NONE',  ( 151.7948205124836250, -33.23291073765550863, 0.000000000000000000 ) ) ;
#16282 = ORIENTED_EDGE ( 'NONE', *, *, #21658, .T. ) ;
#16283 = ORIENTED_EDGE ( 'NONE', *, *, #14191, .T. ) ;
#16284 = EDGE_LOOP ( 'NONE', ( #8388, #4127 ) ) ;
#16285 = CARTESIAN_POINT ( 'NONE',  ( -30.26275506840324070, 1.694272468446254232, 0.000000000000000000 ) ) ;
#16286 = DIRECTION ( 'NONE',  ( 1.000000000000000000, 1.836970198721030181E-16, 0.000000000000000000 ) ) ;
#16287 = EDGE_CURVE ( 'NONE', #19850, #5454, #24821, .T. ) ;
#16288 = CARTESIAN_POINT ( 'NONE',  ( -135.8532207217289738, 40.00000000000002842, -9.153146818113432559 ) ) ;
#16289 = CARTESIAN_POINT ( 'NONE',  ( 4.995406935893286438, 67.35176059880245703, -10.78321810387767066 ) ) ;
#16290 = CARTESIAN_POINT ( 'NONE',  ( -162.0762913951020892, 1.694272876828294194, 0.000000000000000000 ) ) ;
#16291 = EDGE_CURVE ( 'NONE', #858, #20449, #24101, .T. ) ;
#16292 = CARTESIAN_POINT ( 'NONE',  ( -175.9235640272266039, 12.95568063362427047, -42.70623598722775682 ) ) ;
#16293 = CARTESIAN_POINT ( 'NONE',  ( -86.86493150571116928, 8.366608963953661160, 19.60045294882771572 ) ) ;
#16294 = CARTESIAN_POINT ( 'NONE',  ( 199.9999999999998863, 14.88114354045644561, 11.82478185164094775 ) ) ;
#16295 = ADVANCED_FACE ( 'NONE', ( #18688 ), #9233, .T. ) ;
#16296 = EDGE_CURVE ( 'NONE', #19940, #23643, #22560, .T. ) ;
#16297 = CARTESIAN_POINT ( 'NONE',  ( 200.0000000000000000, -18.00239984878453825, 6.108539637176261472 ) ) ;
#16298 = CARTESIAN_POINT ( 'NONE',  ( 163.1118516004056573, 37.29075403953132906, 19.27778845539275565 ) ) ;
#16299 = CARTESIAN_POINT ( 'NONE',  ( -208.1127848780264742, -67.17687982760682530, -10.60833733268364298 ) ) ;
#16300 = FACE_BOUND ( 'NONE', #16522, .T. ) ;
#16301 = CARTESIAN_POINT ( 'NONE',  ( -86.99952317291106851, 18.62540174577003427, -10.54562204237578271 ) ) ;
#16302 = CARTESIAN_POINT ( 'NONE',  ( -280.0000000000000568, -14.14213562373137556, 42.42640687119276066 ) ) ;
#16303 = CARTESIAN_POINT ( 'NONE',  ( -210.0000000000000284, 82.50000000000008527, -52.49999999999978684 ) ) ;
#16304 = CARTESIAN_POINT ( 'NONE',  ( -192.9588430854690273, -18.05360324515454096, 38.51493924976936967 ) ) ;
#16305 = CARTESIAN_POINT ( 'NONE',  ( -238.4067589809705794, -57.25054294065807881, 0.6820004457338858517 ) ) ;
#16306 = CARTESIAN_POINT ( 'NONE',  ( 199.0258546901197860, -8.886439070910094884, 17.97156912711873034 ) ) ;
#16308 = CARTESIAN_POINT ( 'NONE',  ( 199.9999999999999432, -3.553951640073651008E-14, 19.99999999999992539 ) ) ;
#16307 = CARTESIAN_POINT ( 'NONE',  ( 146.6084372240433993, 3.800685668858732935, -3.800685668858610367 ) ) ;
#16309 = CARTESIAN_POINT ( 'NONE',  ( 4.995406935893286438, 67.35176059880245703, -10.78321810387767066 ) ) ;
#16310 = CARTESIAN_POINT ( 'NONE',  ( 23.05038679986473937, 43.09692730306933584, -17.85133178553897793 ) ) ;
#16311 = CARTESIAN_POINT ( 'NONE',  ( -135.8532207217289738, 30.84685318188643066, 2.449293598294708485E-15 ) ) ;
#16312 = ORIENTED_EDGE ( 'NONE', *, *, #22658, .T. ) ;
#16313 = CARTESIAN_POINT ( 'NONE',  ( -105.3755690713226727, -21.75974354311652093, 0.000000000000000000 ) ) ;
#16314 = CARTESIAN_POINT ( 'NONE',  ( -7.769366557095455761, -41.90323276218102677, 22.72119856430033380 ) ) ;
#16315 = CARTESIAN_POINT ( 'NONE',  ( 192.4448373802101173, 19.99999999996063949, 40.00000000000002132 ) ) ;
#16316 = VERTEX_POINT ( 'NONE', #16293 ) ;
#16317 = FACE_OUTER_BOUND ( 'NONE', #6988, .T. ) ;
#16318 = EDGE_CURVE ( 'NONE', #19428, #14640, #22432, .T. ) ;
#16319 = CARTESIAN_POINT ( 'NONE',  ( 199.9999999999999147, -17.67734251759716457, -6.986728219496066927 ) ) ;
#16320 = CARTESIAN_POINT ( 'NONE',  ( 7.112934525951993159, -18.57375239869932670, 44.84100494512510693 ) ) ;
#16321 = CARTESIAN_POINT ( 'NONE',  ( 9.345847406432913118, 14.17927947630575325, -49.32890504403901843 ) ) ;
#16322 = CARTESIAN_POINT ( 'NONE',  ( 199.0135655005340425, -10.56572504866429973, -16.98073106299600710 ) ) ;
#16323 = CARTESIAN_POINT ( 'NONE',  ( 130.8568914410475372, -3.326198072800416995E-13, 34.05028731879788495 ) ) ;
#16324 = CARTESIAN_POINT ( 'NONE',  ( -210.0000000000000284, 71.50000000000002842, -66.50000000000005684 ) ) ;
#16325 = CARTESIAN_POINT ( 'NONE',  ( 199.9999999999999432, 1.065690307512836407E-13, -20.00000000000010303 ) ) ;
#16326 = CARTESIAN_POINT ( 'NONE',  ( -259.2033419157646676, -6.730120644402966867, -49.83842185052038332 ) ) ;
#16327 = CARTESIAN_POINT ( 'NONE',  ( 192.4448373802101173, 20.00000000003945644, 40.00000000000002132 ) ) ;
#16329 = CARTESIAN_POINT ( 'NONE',  ( 0.2972598230769886718, 38.42060263243643448, 18.14793986248763957 ) ) ;
#16328 = CARTESIAN_POINT ( 'NONE',  ( -188.3611024622149728, 23.46270902204793529, -43.02327292322510033 ) ) ;
#16330 = CARTESIAN_POINT ( 'NONE',  ( 0.2972598230769886718, 38.42060263243643448, 18.14793986248763957 ) ) ;
#16331 = CARTESIAN_POINT ( 'NONE',  ( -198.0356074513804572, -55.37879056874826489, 40.00000000000002132 ) ) ;
#16332 = CARTESIAN_POINT ( 'NONE',  ( -162.0762913951020892, 41.69427287692678163, -40.00000000000002132 ) ) ;
#16333 = CARTESIAN_POINT ( 'NONE',  ( 136.1360204305621551, -40.00000000000036238, 35.03383547441254109 ) ) ;
#16334 = CARTESIAN_POINT ( 'NONE',  ( -259.2033419157646676, 21.55415060305830366, 21.55415060305842800 ) ) ;
#16335 = CARTESIAN_POINT ( 'NONE',  ( 98.29820294268670011, 19.44947291833535630, -5.307337294604018929 ) ) ;
#16336 = CARTESIAN_POINT ( 'NONE',  ( 4.995406935893300648, -10.78321810387790514, -67.35176059880241439 ) ) ;
#16337 = VERTEX_POINT ( 'NONE', #14298 ) ;
#16338 = CARTESIAN_POINT ( 'NONE',  ( 184.8905102610680444, -14.79361573936379415, -14.79361573936387941 ) ) ;
#16339 = CARTESIAN_POINT ( 'NONE',  ( -96.94475454971953354, 9.001119816637983106, 20.58449551010110667 ) ) ;
#16340 = APPLICATION_PROTOCOL_DEFINITION ( 'draft international standard', 'automotive_design', 1998, #11214 ) ;
#16341 = EDGE_LOOP ( 'NONE', ( #15297, #25175, #17573, #24096 ) ) ;
#16342 = ORIENTED_EDGE ( 'NONE', *, *, #24271, .T. ) ;
#16343 = CARTESIAN_POINT ( 'NONE',  ( -135.8532207217289738, -50.09629031063965243, -6.472252184284438492 ) ) ;
#16344 = CARTESIAN_POINT ( 'NONE',  ( 22.37977766479031771, -47.17011059971120090, -13.85469381971834402 ) ) ;
#16345 = ORIENTED_EDGE ( 'NONE', *, *, #24526, .F. ) ;
#16346 = CARTESIAN_POINT ( 'NONE',  ( -97.72675010090144099, -20.89622088363380925, 8.185591577777151073 ) ) ;
#16347 = CARTESIAN_POINT ( 'NONE',  ( -190.0000000000000000, 52.49999999999987210, -82.49999999999998579 ) ) ;
#16348 = VERTEX_POINT ( 'NONE', #2205 ) ;
#16349 = CARTESIAN_POINT ( 'NONE',  ( 199.9999999999999716, 15.96353534131429797, 10.31599105002992545 ) ) ;
#16350 = CARTESIAN_POINT ( 'NONE',  ( -362.0709805440841365, -4.734761052820324085E-14, -10.00000000000004796 ) ) ;
#16351 = CARTESIAN_POINT ( 'NONE',  ( 0.2972598230769938343, 10.13633138497472252, 10.13633138497475628 ) ) ;
#16352 = CARTESIAN_POINT ( 'NONE',  ( -188.4702232936898554, -47.05182887786696710, -13.83721295434361487 ) ) ;
#16353 = CARTESIAN_POINT ( 'NONE',  ( 130.8568914410475088, -40.00000000000001421, 5.949712681206549725 ) ) ;
#16354 = CARTESIAN_POINT ( 'NONE',  ( 151.7948205124836250, -33.23291073765550863, 0.000000000000000000 ) ) ;
#16355 = CARTESIAN_POINT ( 'NONE',  ( 19.06497207195981147, 38.31983398719673772, -38.31983398719579981 ) ) ;
#16356 = CARTESIAN_POINT ( 'NONE',  ( 199.0218477376944577, 3.734929907270702287, 19.65178994764128717 ) ) ;
#16357 = CARTESIAN_POINT ( 'NONE',  ( -259.2033419157646676, -40.00000000000017764, 30.48217210827725054 ) ) ;
#16358 = CARTESIAN_POINT ( 'NONE',  ( -259.2033419157646676, -1.564921101325656229E-13, 30.48217210827739621 ) ) ;
#16359 = CARTESIAN_POINT ( 'NONE',  ( -280.0000000000000000, 1.839446121267387017E-14, -20.00000000000001421 ) ) ;
#16360 = CARTESIAN_POINT ( 'NONE',  ( -626.9846540392142060, 75.00000000000000000, 0.000000000000000000 ) ) ;
#16361 = CARTESIAN_POINT ( 'NONE',  ( -208.1127848780264742, -38.89260858015758515, 38.89260858015713751 ) ) ;
#16362 = CARTESIAN_POINT ( 'NONE',  ( -192.9588430854690273, -14.46834944099973264, -40.00000000000002132 ) ) ;
#16363 = CARTESIAN_POINT ( 'NONE',  ( 170.2234770963711128, 17.36149277826973503, 39.20704971665401217 ) ) ;
#16364 = DIRECTION ( 'NONE',  ( 0.000000000000000000, -0.000000000000000000, 1.000000000000000000 ) ) ;
#16365 = CARTESIAN_POINT ( 'NONE',  ( 8.517493190815677906, -49.32792454093240764, 14.17913040910394429 ) ) ;
#16366 = CARTESIAN_POINT ( 'NONE',  ( -100.7734535825088358, 1.654174317907124744E-13, -17.32597176626811120 ) ) ;
#16367 = CARTESIAN_POINT ( 'NONE',  ( -91.56559293963834989, -40.00000000000009948, 17.32597176626796553 ) ) ;
#16368 = CIRCLE ( 'NONE', #23188, 69.99999999999998579 ) ;
#16369 = CARTESIAN_POINT ( 'NONE',  ( -192.9588430854690273, 38.51493924976939098, -18.05360324515436687 ) ) ;
#16370 = DIRECTION ( 'NONE',  ( -1.000000000000000000, 1.836970198721030181E-16, 0.000000000000000000 ) ) ;
#16371 = CARTESIAN_POINT ( 'NONE',  ( -94.58366989427317151, -9.000605044545517686, -20.58370269626833604 ) ) ;
#16372 = CARTESIAN_POINT ( 'NONE',  ( 136.1360204305621551, -31.79587985999244282, -24.77266263493140386 ) ) ;
#16373 = ORIENTED_EDGE ( 'NONE', *, *, #25592, .F. ) ;
#16374 = CARTESIAN_POINT ( 'NONE',  ( 130.8568914410475088, -52.36146031193413108, -4.207082182990267150 ) ) ;
#16375 = DIRECTION ( 'NONE',  ( -1.000000000000000000, 0.000000000000000000, 0.000000000000000000 ) ) ;
#16376 = CARTESIAN_POINT ( 'NONE',  ( 14.38125909742182884, -55.17850393974264733, -40.00000000000002132 ) ) ;
#16377 = CARTESIAN_POINT ( 'NONE',  ( -30.26275506840324070, 1.198031551616030033, -1.198031551616006496 ) ) ;
#16378 = SHAPE_REPRESENTATION_RELATIONSHIP ( 'NONE' , 'NONE' ,  #12169, #11500 ) ;
#16379 = ORIENTED_EDGE ( 'NONE', *, *, #16134, .T. ) ;
#16380=STYLED_ITEM('',(#26395),#8975);
#16381 = ORIENTED_EDGE ( 'NONE', *, *, #13762, .F. ) ;
#16382 = VECTOR ( 'NONE', #19097, 1000.000000000000000 ) ;
#16383 = CARTESIAN_POINT ( 'NONE',  ( 199.9999999999999147, 7.829686725388152801, 17.32023057510092912 ) ) ;
#16384 = CARTESIAN_POINT ( 'NONE',  ( -28.75808802781980944, -18.59445401971578704, -35.61482992978298512 ) ) ;
#16385 = EDGE_CURVE ( 'NONE', #2425, #3239, #10573, .T. ) ;
#16386 = CARTESIAN_POINT ( 'NONE',  ( -3.856733984653986980, 17.89110409353202158, 43.19294614843431646 ) ) ;
#16387 = VERTEX_POINT ( 'NONE', #21352 ) ;
#16388 = ORIENTED_EDGE ( 'NONE', *, *, #25739, .F. ) ;
#16389 = APPLICATION_CONTEXT ( 'automotive_design' ) ;
#16390 = CARTESIAN_POINT ( 'NONE',  ( -238.4067589809705794, 0.6820004457912757223, 0.6820004457913219076 ) ) ;
#16391 = CARTESIAN_POINT ( 'NONE',  ( 199.0106728332879698, -5.188592077825961546, -19.31531804097554073 ) ) ;
#16392 = CYLINDRICAL_SURFACE ( 'NONE', #3913, 20.53474504356812247 ) ;
#16393 = EDGE_CURVE ( 'NONE', #3239, #1984, #12970, .T. ) ;
#16394 = CARTESIAN_POINT ( 'NONE',  ( -56.48582580120559271, -6.472252184284187138, -6.472252184284199572 ) ) ;
#16395 = VECTOR ( 'NONE', #9546, 1000.000000000000000 ) ;
#16396 = EDGE_CURVE ( 'NONE', #10496, #18341, #21978, .T. ) ;
#16397 = CARTESIAN_POINT ( 'NONE',  ( -100.0957100001246687, -8.517115559311239537, -20.56213589529557240 ) ) ;
#16398 = ADVANCED_FACE ( 'NONE', ( #23219 ), #17742, .T. ) ;
#16399 = CARTESIAN_POINT ( 'NONE',  ( -91.56559293963834989, 1.671088883502053755E-13, -17.32597176626811120 ) ) ;
#16400 = CARTESIAN_POINT ( 'NONE',  ( -238.4067589809705794, -3.369206980223063916E-14, -0.9644942799825824142 ) ) ;
#16401 = CARTESIAN_POINT ( 'NONE',  ( -114.4364955367328349, 20.29001642038852538, -8.064892380842216824 ) ) ;
#16402 = CIRCLE ( 'NONE', #8322, 40.00000000000003553 ) ;
#16403 = DIRECTION ( 'NONE',  ( 0.000000000000000000, 0.000000000000000000, -1.000000000000000000 ) ) ;
#16404 = CARTESIAN_POINT ( 'NONE',  ( 199.0151032989660678, 15.24552994868030531, 12.94849756636627447 ) ) ;
#16405 = CARTESIAN_POINT ( 'NONE',  ( -188.4265004370476504, 23.47686928852973764, 43.04236487214772922 ) ) ;
#16406 = CARTESIAN_POINT ( 'NONE',  ( 23.38399212876534961, -23.33762193384630379, -42.85408588822686227 ) ) ;
#16407 = CARTESIAN_POINT ( 'NONE',  ( 192.4448373802101173, 14.14213562375922884, -42.42640687116488607 ) ) ;
#16408 = CARTESIAN_POINT ( 'NONE',  ( -97.72675010090189573, 20.56394680065915637, -8.987772175319548751 ) ) ;
#16409 = CARTESIAN_POINT ( 'NONE',  ( -208.1127848780264742, -38.89260858015758515, 38.89260858015713751 ) ) ;
#16410 = CARTESIAN_POINT ( 'NONE',  ( -210.0000000000000284, 52.49999999999988631, -82.49999999999998579 ) ) ;
#16411 = CARTESIAN_POINT ( 'NONE',  ( -192.9588430854689989, -10.23066800230742501, -10.23066800230756712 ) ) ;
#16412 = CARTESIAN_POINT ( 'NONE',  ( -105.3755690713226585, 21.75974354311648185, 40.00000000000002132 ) ) ;
#16413 = MECHANICAL_DESIGN_GEOMETRIC_PRESENTATION_REPRESENTATION (  '', ( #18539 ), #20677 ) ;
#16414 = FACE_BOUND ( 'NONE', #24514, .T. ) ;
#16415 = CARTESIAN_POINT ( 'NONE',  ( -162.0762913951020607, -41.69427287692683848, 40.00000000000002132 ) ) ;
#16416 = CARTESIAN_POINT ( 'NONE',  ( -114.5469942457206116, 9.971021741842124086, 19.54051464164524887 ) ) ;
#16417 = CARTESIAN_POINT ( 'NONE',  ( -198.0356074513804572, 40.00000000000014921, -15.37879056873028816 ) ) ;
#16418 = CARTESIAN_POINT ( 'NONE',  ( -259.2033419157646676, 21.55415060305839958, -35.01439189186541512 ) ) ;
#16419 = CARTESIAN_POINT ( 'NONE',  ( 163.1118516004056573, -27.26290988616869626, -40.00000000000002132 ) ) ;
#16420 = ORIENTED_EDGE ( 'NONE', *, *, #24303, .F. ) ;
#16421 = EDGE_LOOP ( 'NONE', ( #12134, #5046 ) ) ;
#16422 = ORIENTED_EDGE ( 'NONE', *, *, #1337, .T. ) ;
#16423 = CARTESIAN_POINT ( 'NONE',  ( -280.0000000000000568, -20.00000000000006750, 40.00000000000002132 ) ) ;
#16424 = CLOSED_SHELL ( 'NONE', ( #9152, #19460, #21274, #13859, #15158, #17292, #8326, #7194, #9806, #8575, #5720, #10291, #23166, #17427, #1772, #193, #3968, #23755, #14346, #4223, #304, #26165, #20798, #17741, #23538, #9299, #12824, #300, #1053, #18250, #24702, #14331, #21016, #5912, #12528, #2006, #21811, #15095, #8588, #14484 ) ) ;
#16425 = CARTESIAN_POINT ( 'NONE',  ( 144.1620285550793312, 12.51613133675833822, 30.21661402164571797 ) ) ;
#16426 = CARTESIAN_POINT ( 'NONE',  ( -280.0000000000000000, 14.14213562373108246, -14.14213562373078581 ) ) ;
#16427 = CARTESIAN_POINT ( 'NONE',  ( -114.6297772182882397, -21.30737554388467814, -5.474609583126212264 ) ) ;
#16428 = AXIS2_PLACEMENT_3D ( 'NONE', #21600, #19221, #3373 ) ;
#16429 = CARTESIAN_POINT ( 'NONE',  ( -199.9999999999999716, -53.44529986889247652, -10.02640517461732372 ) ) ;
#16430 = CARTESIAN_POINT ( 'NONE',  ( -726.9846540392142060, 66.50000000000009948, 66.50000000000005684 ) ) ;
#16431 = CARTESIAN_POINT ( 'NONE',  ( 199.9999999999999432, 17.49244587396685091, 7.427265670988617785 ) ) ;
#16432 = CARTESIAN_POINT ( 'NONE',  ( 199.9999999999998863, -15.08414020386666721, -11.56687813556520261 ) ) ;
#16433 = CARTESIAN_POINT ( 'NONE',  ( 200.0000000000000000, 14.14213562373041455, 42.42640687119311593 ) ) ;
#16434 = CARTESIAN_POINT ( 'NONE',  ( -280.0000000000000568, -42.42640687119305198, 14.14213562373058686 ) ) ;
#16435 = CARTESIAN_POINT ( 'NONE',  ( -190.0000000000001705, -69.99999999999994316, 8.572527594031469837E-15 ) ) ;
#16436 = CARTESIAN_POINT ( 'NONE',  ( -135.8532207217289738, 40.00000000000031974, -30.84685318188603986 ) ) ;
#16437 = CARTESIAN_POINT ( 'NONE',  ( -86.96347745069645896, -12.89780903124443689, 43.67073346367968156 ) ) ;
#16438 = CARTESIAN_POINT ( 'NONE',  ( -210.0000000000000284, -52.49999999999972999, -82.49999999999998579 ) ) ;
#16439 = CARTESIAN_POINT ( 'NONE',  ( 130.8568914410475372, -24.07718906447222551, -24.07718906447233209 ) ) ;
#16440 = CARTESIAN_POINT ( 'NONE',  ( -105.3755690713226585, -41.18208027870589660, -15.38646221621809040 ) ) ;
#16441 = CARTESIAN_POINT ( 'NONE',  ( -190.0000000000001705, 1.836970198721007106E-15, 0.000000000000000000 ) ) ;
#16442 = EDGE_CURVE ( 'NONE', #8666, #7950, #5361, .T. ) ;
#16443 =( BOUNDED_SURFACE ( )  B_SPLINE_SURFACE ( 3, 2, ( 
 ( #6619, #4118, #18329 ),
 ( #25003, #12342, #18868 ),
 ( #12214, #649, #20470 ),
 ( #8622, #14602, #14737 ),
 ( #20336, #22868, #2245 ),
 ( #18462, #10352, #8353 ),
 ( #110, #12612, #8217 ),
 ( #20740, #240, #16474 ),
 ( #24598, #18601, #6353 ),
 ( #4645, #12747, #8756 ),
 ( #10488, #380, #14472 ),
 ( #4381, #2509, #2651 ) ),
 .UNSPECIFIED., .F., .F., .F. ) 
 B_SPLINE_SURFACE_WITH_KNOTS ( ( 4, 2, 2, 2, 2, 4 ),
 ( 3, 3 ),
 ( 0.006022589392327087551, 0.01254516766564490668, 0.01580645680230381711, 0.01906774593896272754, 0.02559032421228054494, 0.03211290248559836580 ),
 ( 0.000000000000000000, 1.000000000000000000 ),
 .UNSPECIFIED. ) 
 GEOMETRIC_REPRESENTATION_ITEM ( )  RATIONAL_B_SPLINE_SURFACE ( (
 ( 1.000000000000000000, 0.9998834880171258988, 1.000000000000000000),
 ( 1.000000000000000000, 0.9998139205011338237, 1.000000000000000000),
 ( 1.000000000000000000, 0.9997315632445886724, 1.000000000000000000),
 ( 1.000000000000000000, 0.9996405464946352959, 1.000000000000000000),
 ( 1.000000000000000000, 0.9996155081776924023, 1.000000000000000000),
 ( 1.000000000000000000, 0.9995814087511104562, 1.000000000000000000),
 ( 1.000000000000000000, 0.9995724100939920032, 1.000000000000000000),
 ( 1.000000000000000000, 0.9995726760936896049, 1.000000000000000000),
 ( 1.000000000000000000, 0.9996103361816741639, 1.000000000000000000),
 ( 1.000000000000000000, 0.9997312749796802844, 1.000000000000000000),
 ( 1.000000000000000000, 0.9998135910914284219, 1.000000000000000000),
 ( 1.000000000000000000, 0.9998834880173383954, 1.000000000000000000) ) ) 
 REPRESENTATION_ITEM ( '' )  SURFACE ( )  );
#16445 = CARTESIAN_POINT ( 'NONE',  ( 4.995406935893292655, 39.99999999999982947, 55.24977328856478209 ) ) ;
#16444 = CARTESIAN_POINT ( 'NONE',  ( -238.4067589809705794, 28.96627169325354956, -28.96627169325289231 ) ) ;
#16446 = CARTESIAN_POINT ( 'NONE',  ( 146.6084372240433709, 32.08495691632030145, 24.48358557860365181 ) ) ;
#16447 = CARTESIAN_POINT ( 'NONE',  ( 22.77497178454824223, 43.17449153292937325, -17.88345994150133578 ) ) ;
#16448 = CARTESIAN_POINT ( 'NONE',  ( 14.38125909742180752, 55.17850393972636880, 2.449293598294708485E-15 ) ) ;
#16449 = CARTESIAN_POINT ( 'NONE',  ( -100.7734535825088358, -16.03295912088706743, -16.03295912088710296 ) ) ;
#16450 = VECTOR ( 'NONE', #18192, 1000.000000000000000 ) ;
#16451 = CARTESIAN_POINT ( 'NONE',  ( -4.027137536849560107, -43.00884733904522506, 23.45200847982325598 ) ) ;
#16452 = CARTESIAN_POINT ( 'NONE',  ( 0.2972598230769930572, 54.33493731733936016, 2.449293598294708485E-15 ) ) ;
#16453 = ADVANCED_FACE ( 'NONE', ( #9294, #23280 ), #23651, .F. ) ;
#16454 = ORIENTED_EDGE ( 'NONE', *, *, #21219, .F. ) ;
#16455 = SPHERICAL_SURFACE ( 'NONE', #13070, 15.00000000000000000 ) ;
#16456 = AXIS2_PLACEMENT_3D ( 'NONE', #10335, #14321, #361 ) ;
#16457 = CARTESIAN_POINT ( 'NONE',  ( 130.8568914410475088, -52.36146031193419503, 4.207082182989537955 ) ) ;
#16458 = CARTESIAN_POINT ( 'NONE',  ( -47.45115950043103226, -10.57586762654845280, 31.57405104340034541 ) ) ;
#16459 = CARTESIAN_POINT ( 'NONE',  ( -3.205219349397945283, 17.96245967913786856, -43.36521377095283469 ) ) ;
#16460 = CARTESIAN_POINT ( 'NONE',  ( 199.0175917791061977, -16.16856137136818816, -11.77441583767826039 ) ) ;
#16461 = CARTESIAN_POINT ( 'NONE',  ( 48.46046615278683589, -37.63122026539700471, 11.89583623203270157 ) ) ;
#16462 = CARTESIAN_POINT ( 'NONE',  ( 132.4338126186516149, -29.78211700502427917, 12.33615677966322721 ) ) ;
#16463 = CARTESIAN_POINT ( 'NONE',  ( -188.2507053403079738, -13.82466505297404247, 46.97353740712713233 ) ) ;
#16464 = CARTESIAN_POINT ( 'NONE',  ( 57.59792236341147031, -30.00663442387662627, -26.56190807104723461 ) ) ;
#16465 = CARTESIAN_POINT ( 'NONE',  ( 163.1118516004056573, 27.26290988616875310, 0.000000000000000000 ) ) ;
#16467 = CARTESIAN_POINT ( 'NONE',  ( 192.4448373802100889, -14.14213562375896061, 14.14213562375865330 ) ) ;
#16466 = CARTESIAN_POINT ( 'NONE',  ( -188.2957210513887674, 13.82790368522472946, -46.98905903629629677 ) ) ;
#16468 = CARTESIAN_POINT ( 'NONE',  ( -208.1127848780264742, 38.89260858015707356, 17.67593391476696141 ) ) ;
#16469 = CARTESIAN_POINT ( 'NONE',  ( -238.4067589809705510, -40.96449427998265946, -2.449293598294708485E-15 ) ) ;
#16470 = CARTESIAN_POINT ( 'NONE',  ( -86.96347745069644475, 18.24025645688351105, 2.449293598294708485E-15 ) ) ;
#16471 = CARTESIAN_POINT ( 'NONE',  ( -100.7734535825088500, -40.00000000000027711, 22.67402823373149801 ) ) ;
#16472 = CARTESIAN_POINT ( 'NONE',  ( 184.8905102610680444, 13.49065550809807945, 13.49065550809809544 ) ) ;
#16473 = ADVANCED_FACE ( 'NONE', ( #25791 ), #20656, .T. ) ;
#16474 = CARTESIAN_POINT ( 'NONE',  ( -94.58360650935111380, 20.91945674502911956, -8.190527749670891922 ) ) ;
#16475 = CARTESIAN_POINT ( 'NONE',  ( 163.1118516004056573, 19.27778845539265618, -37.29075403953135037 ) ) ;
#16476 = CARTESIAN_POINT ( 'NONE',  ( -114.6679276626351509, -4.801621139947936712, 21.51116696530568362 ) ) ;
#16477 = VERTEX_POINT ( 'NONE', #7540 ) ;
#16478 = CARTESIAN_POINT ( 'NONE',  ( 200.0000000000000000, -42.42640687119293119, 14.14213562373082134 ) ) ;
#16479 = CARTESIAN_POINT ( 'NONE',  ( -103.9650464692577998, 8.298274099270956938, 20.03380587467329832 ) ) ;
#16480 = CARTESIAN_POINT ( 'NONE',  ( 4.995406935893305977, -39.06748935135212264, 39.06748935135171763 ) ) ;
#16481 = CARTESIAN_POINT ( 'NONE',  ( -4.061681315507636114, -46.98276670624674267, -13.82654462146565777 ) ) ;
#16482 = EDGE_CURVE ( 'NONE', #8935, #4460, #15953, .T. ) ;
#16483 = EDGE_CURVE ( 'NONE', #10709, #19077, #3696, .T. ) ;
#16484 = ORIENTED_EDGE ( 'NONE', *, *, #8406, .F. ) ;
#16485 = CARTESIAN_POINT ( 'NONE',  ( 14.33519811653601472, -49.08818492847915849, -14.14278418308693475 ) ) ;
#16486 = CARTESIAN_POINT ( 'NONE',  ( -199.9999999999999716, -44.86878812508714276, 24.82633483071253622 ) ) ;
#16487 = ORIENTED_EDGE ( 'NONE', *, *, #225, .T. ) ;
#16488 = CARTESIAN_POINT ( 'NONE',  ( 199.9999999999998863, 3.552885321105354599, -18.66644157592937248 ) ) ;
#16489 = CARTESIAN_POINT ( 'NONE',  ( -4.039451493210489907, 13.82811171175507603, -46.99046209229789639 ) ) ;
#16490 = CARTESIAN_POINT ( 'NONE',  ( -208.1127848780265026, 10.60833733269537049, 10.60833733269544510 ) ) ;
#16491 = CARTESIAN_POINT ( 'NONE',  ( -188.6890294954627905, -43.11788624869991793, -23.53287096354742403 ) ) ;
#16492 = CARTESIAN_POINT ( 'NONE',  ( -208.1127848780264742, -40.00000000000011369, 15.00245453012655439 ) ) ;
#16493 = CARTESIAN_POINT ( 'NONE',  ( -100.7734535825088358, 17.32597176626809343, 2.449293598294708485E-15 ) ) ;
#16494 = CARTESIAN_POINT ( 'NONE',  ( -30.26275506840324070, 1.198031551616030033, -1.198031551616006496 ) ) ;
#16495 = DIRECTION ( 'NONE',  ( 0.000000000000000000, 0.000000000000000000, 1.000000000000000000 ) ) ;
#16496 = CARTESIAN_POINT ( 'NONE',  ( 136.1360204305621266, 1.473277640373554421E-13, -35.03383547441296741 ) ) ;
#16497 = CARTESIAN_POINT ( 'NONE',  ( -213.1075012329537230, 39.99999999999992895, 13.71589010951925935 ) ) ;
#16498 = CARTESIAN_POINT ( 'NONE',  ( 170.2234770963711128, 1.169953928977015745E-13, -24.55285855007187124 ) ) ;
#16499 = CARTESIAN_POINT ( 'NONE',  ( 146.6084372240433993, 34.62501878078308692, 0.000000000000000000 ) ) ;
#16500 = CARTESIAN_POINT ( 'NONE',  ( -213.1075012329537230, -53.71589010950170717, 40.00000000000002132 ) ) ;
#16501 = CARTESIAN_POINT ( 'NONE',  ( -208.1127848780264742, -10.60833733268345469, 67.17687982760682530 ) ) ;
#16502 = CARTESIAN_POINT ( 'NONE',  ( -86.86493150571114086, -8.366608963953616751, 19.60045294882772993 ) ) ;
#16503 = FACE_OUTER_BOUND ( 'NONE', #15420, .T. ) ;
#16504 = CARTESIAN_POINT ( 'NONE',  ( 136.1360204305621551, 40.00000000000009948, -4.966164525586641787 ) ) ;
#16505 = CARTESIAN_POINT ( 'NONE',  ( 0.2972598230770030492, -1.921041075453695163E-13, 54.33493731733936016 ) ) ;
#16506 = CARTESIAN_POINT ( 'NONE',  ( 163.1118516004056573, 9.006482792074356425, -47.56205970284957374 ) ) ;
#16507 = DIRECTION ( 'NONE',  ( 1.000000000000000000, 1.303213150798907793E-16, 2.465190328815661892E-32 ) ) ;
#16508 = CARTESIAN_POINT ( 'NONE',  ( 190.0000000000000000, -66.50000000000001421, 66.50000000000005684 ) ) ;
#16509 = CARTESIAN_POINT ( 'NONE',  ( -56.48582580120558561, -50.09629031063963112, -6.472252184284449150 ) ) ;
#16510 = VERTEX_POINT ( 'NONE', #13162 ) ;
#16511 = CARTESIAN_POINT ( 'NONE',  ( -5.152948516935869527, 42.67688069069274093, -23.23217004669248809 ) ) ;
#16512 = CARTESIAN_POINT ( 'NONE',  ( -716.9846540392142060, 66.50000000000009948, 66.50000000000005684 ) ) ;
#16513 = CARTESIAN_POINT ( 'NONE',  ( -192.9588430854689705, -54.46834944099975928, -2.449293598294708485E-15 ) ) ;
#16514 = DIRECTION ( 'NONE',  ( 0.000000000000000000, -0.9307566067079398042, -0.3656393565653475175 ) ) ;
#16515 = CARTESIAN_POINT ( 'NONE',  ( 146.6084372240433993, -24.48358557860353457, 24.48358557860296258 ) ) ;
#16516 = ORIENTED_EDGE ( 'NONE', *, *, #13851, .T. ) ;
#16517 = EDGE_LOOP ( 'NONE', ( #19666, #18039, #593, #962 ) ) ;
#16518 = DIRECTION ( 'NONE',  ( 0.000000000000000000, 1.000000000000000000, 0.000000000000000000 ) ) ;
#16519 = CARTESIAN_POINT ( 'NONE',  ( -96.94475454971987460, 9.001119816634455262, -20.58449551010242828 ) ) ;
#16520 = CARTESIAN_POINT ( 'NONE',  ( 6.011245401487562923, 18.54985650214280923, 44.78331514754981413 ) ) ;
#16521 = EDGE_LOOP ( 'NONE', ( #4559, #25950, #6356, #3716 ) ) ;
#16522 = EDGE_LOOP ( 'NONE', ( #11950, #26193 ) ) ;
#16523 = CARTESIAN_POINT ( 'NONE',  ( -280.0000000000000000, -20.00000000000006750, 0.000000000000000000 ) ) ;
#16524 = CARTESIAN_POINT ( 'NONE',  ( 199.0111317961331281, -6.131174403448985011, -19.03732645848564431 ) ) ;
#16525 = FACE_OUTER_BOUND ( 'NONE', #25994, .T. ) ;
#16526 = CARTESIAN_POINT ( 'NONE',  ( -238.4067589809705794, 0.6820004457912757223, 0.6820004457913219076 ) ) ;
#16527 = CARTESIAN_POINT ( 'NONE',  ( -238.4067589809705794, 28.96627169325324758, -27.60227080167054581 ) ) ;
#16528 = CARTESIAN_POINT ( 'NONE',  ( -199.9999999999999432, -15.63350978565347660, 47.95319408140866813 ) ) ;
#16529 = AXIS2_PLACEMENT_3D ( 'NONE', #18967, #8716, #25484 ) ;
#16530 = CARTESIAN_POINT ( 'NONE',  ( -93.01741312765729219, -8.946232117619631552, -20.50009083229717533 ) ) ;
#16531 = CARTESIAN_POINT ( 'NONE',  ( -30.26275506840324425, 40.00000000000044764, -41.69427246844585255 ) ) ;
#16532 = CARTESIAN_POINT ( 'NONE',  ( 57.59792236341147031, -1.493297263419786540E-14, 2.435789363418160658 ) ) ;
#16533 = CARTESIAN_POINT ( 'NONE',  ( -640.9073278876498989, 29.89490142532471850, 26.57793756188680234 ) ) ;
#16534 = FACE_OUTER_BOUND ( 'NONE', #10969, .T. ) ;
#16535 = CARTESIAN_POINT ( 'NONE',  ( 199.0064300139308102, 18.94043123351016433, -6.416860702434988184 ) ) ;
#16536 = CARTESIAN_POINT ( 'NONE',  ( -188.8753211508389711, 17.93495349242735060, 43.29880796194883885 ) ) ;
#16537 = CARTESIAN_POINT ( 'NONE',  ( -56.48582580120559271, 6.472252184284121412, 6.472252184284244869 ) ) ;
#16538 = CARTESIAN_POINT ( 'NONE',  ( 170.2234770963711128, 17.36149277826973503, 39.20704971665401217 ) ) ;
#16539 = LINE ( 'NONE', #22805, #3204 ) ;
#16540 = CARTESIAN_POINT ( 'NONE',  ( 19.06497207195980792, 18.24870850772790831, -38.31983398719609824 ) ) ;
#16541 = CARTESIAN_POINT ( 'NONE',  ( -199.9999999999999716, 46.84854965773192248, -17.28402242884627782 ) ) ;
#16542 = CARTESIAN_POINT ( 'NONE',  ( -198.0356074513804572, -15.37879056873074290, 0.000000000000000000 ) ) ;
#16543 = CARTESIAN_POINT ( 'NONE',  ( 190.0000000000000000, -35.78896085774750446, -65.91016826501511616 ) ) ;
#16544 = CARTESIAN_POINT ( 'NONE',  ( -198.0356074513804572, -15.37879056873074290, 0.000000000000000000 ) ) ;
#16545 = CARTESIAN_POINT ( 'NONE',  ( -114.6980683190641628, 18.22973761981876706, 12.42092015837599739 ) ) ;
#16546 = CARTESIAN_POINT ( 'NONE',  ( -162.0762913951021176, 40.00000000000042633, -41.69427287672947102 ) ) ;
#16547 = CARTESIAN_POINT ( 'NONE',  ( 199.0121230032554251, -8.046372254322770701, -18.31269210357472943 ) ) ;
#16548 = CARTESIAN_POINT ( 'NONE',  ( 154.0339099654741517, -11.67508747798902391, 28.18615453125275394 ) ) ;
#16549 = VERTEX_POINT ( 'NONE', #13533 ) ;
#16551 = ORIENTED_EDGE ( 'NONE', *, *, #465, .T. ) ;
#16550 = ADVANCED_FACE ( 'NONE', ( #21282 ), #25240, .T. ) ;
#16552 = VERTEX_POINT ( 'NONE', #17783 ) ;
#16553 = CARTESIAN_POINT ( 'NONE',  ( -213.1075012329537230, 13.71589010951907994, 0.000000000000000000 ) ) ;
#16554 = B_SPLINE_CURVE_WITH_KNOTS ( 'NONE', 3,
 ( #8514, #16759, #2536, #24762, #24893, #23034, #6259, #21028, #4282, #2679, #2272, #12372, #6648, #12501, #10786, #4543, #4672, #10920, #20901, #20766, #18763, #16897, #14763, #19031, #18896, #6515, #14894, #675, #20500, #8784, #10381, #18491, #810, #10514 ),
 .UNSPECIFIED., .F., .F.,
 ( 4, 2, 2, 2, 2, 2, 2, 2, 2, 2, 2, 2, 2, 2, 2, 2, 4 ),
 ( -5.298243351207334109E-05, 0.01887868273877498990, 0.02834451532491851986, 0.03071097347145438500, 0.03307743161799024667, 0.03544388976452610834, 0.03781034791106197002, 0.04254326420413369336, 0.04727618049720541671, 0.04964263864374132001, 0.05200909679027721638, 0.05674201308334893973, 0.05910847122988479446, 0.06029170030315276346, 0.06147492937642073246, 0.06620784566949260153, 0.07567367825563635353 ),
 .UNSPECIFIED. ) ;
#16555 = CARTESIAN_POINT ( 'NONE',  ( -56.48582580120559271, 21.81201906317798489, -21.81201906317746619 ) ) ;
#16556 = B_SPLINE_CURVE_WITH_KNOTS ( 'NONE', 3,
 ( #16272, #4190, #2185, #18401, #6949, #23448, #720, #7207, #2720, #15067, #21067, #2974, #13208, #17445, #5346, #23197 ),
 .UNSPECIFIED., .F., .F.,
 ( 4, 2, 2, 2, 2, 2, 2, 4 ),
 ( 1.734723475976807094E-18, 0.004250215528541258399, 0.006375323292811887164, 0.008500431057082516798, 0.01275064658562377433, 0.01381320046775908784, 0.01487575434989440309, 0.01700086211416503013 ),
 .UNSPECIFIED. ) ;
#16557 = CARTESIAN_POINT ( 'NONE',  ( -105.3239292022295075, -20.72686647363872581, -5.381957438748616873 ) ) ;
#16558 = CARTESIAN_POINT ( 'NONE',  ( -188.2995950289364089, -13.82811170417104840, -46.99046209955525200 ) ) ;
#16559 = CARTESIAN_POINT ( 'NONE',  ( -87.13361725327072804, 0.6795304812954694462, -21.49321519333428654 ) ) ;
#16560 = CARTESIAN_POINT ( 'NONE',  ( 199.9999999999997442, 1.230017881244859446, -18.96210773722240361 ) ) ;
#16561 = CARTESIAN_POINT ( 'NONE',  ( 199.9999999999999147, 10.03116143388543868, -16.13932148327019078 ) ) ;
#16562 = CARTESIAN_POINT ( 'NONE',  ( -86.96347745069644475, -15.38646221621738164, -41.18208027870615240 ) ) ;
#16563 = CARTESIAN_POINT ( 'NONE',  ( -192.9588430854689989, -10.23066800230742501, -10.23066800230756712 ) ) ;
#16564 = DIRECTION ( 'NONE',  ( 0.000000000000000000, 1.000000000000000000, 0.000000000000000000 ) ) ;
#16565 = CARTESIAN_POINT ( 'NONE',  ( -238.4067589809705794, 39.99999999999999289, -0.9644942799821634161 ) ) ;
#16566 = CARTESIAN_POINT ( 'NONE',  ( -213.1075012329537230, -37.98287015391257881, 18.58567234101111509 ) ) ;
#16567 = DIRECTION ( 'NONE',  ( -0.01051738777841135231, 0.9166396752739897069, 0.3995761382614246848 ) ) ;
#16568 = DIRECTION ( 'NONE',  ( 0.000000000000000000, -1.000000000000000000, 0.000000000000000000 ) ) ;
#16569 = CARTESIAN_POINT ( 'NONE',  ( 14.38125909742181285, -10.73282306404727393, 10.73282306404716380 ) ) ;
#16570 = CARTESIAN_POINT ( 'NONE',  ( 199.0116138701751538, 18.70391647836493476, 7.080528309964213562 ) ) ;
#16571 = CIRCLE ( 'NONE', #25511, 14.99999999999999467 ) ;
#16573 = CARTESIAN_POINT ( 'NONE',  ( 163.1118516004056573, -40.00000000000003553, 12.73709011382460687 ) ) ;
#16572 = CARTESIAN_POINT ( 'NONE',  ( 136.1360204305621551, 31.79587985999232558, 24.77266263493161702 ) ) ;
#16574 = CARTESIAN_POINT ( 'NONE',  ( 184.8905102610680444, 13.49065550809757497, 43.07788698682593065 ) ) ;
#16575 = CARTESIAN_POINT ( 'NONE',  ( 17.65190073994223852, 44.23515346912816426, -24.35922420889879447 ) ) ;
#16576 = CARTESIAN_POINT ( 'NONE',  ( 170.2234770963711128, 15.44714144992819627, -40.00000000000002132 ) ) ;
#16577 = CARTESIAN_POINT ( 'NONE',  ( 130.8568914410475372, 34.05028731879791337, 0.000000000000000000 ) ) ;
#16578 = CARTESIAN_POINT ( 'NONE',  ( 146.6084372240433709, -34.62501878078303008, 40.00000000000002132 ) ) ;
#16579 = CARTESIAN_POINT ( 'NONE',  ( -4.112199523540559731, -42.98379141459074049, 23.43514144949434552 ) ) ;
#16580 = CARTESIAN_POINT ( 'NONE',  ( 19.06497207195980792, 54.19242893257844429, 40.00000000000002132 ) ) ;
#16581 = ORIENTED_EDGE ( 'NONE', *, *, #4305, .T. ) ;
#16582 = CARTESIAN_POINT ( 'NONE',  ( -3.555049149807541387, 23.55301256057208903, -43.14507846637719979 ) ) ;
#16583 = CARTESIAN_POINT ( 'NONE',  ( 146.6084372240433993, -24.48358557860319706, -24.48358557860330720 ) ) ;
#16584 = CARTESIAN_POINT ( 'NONE',  ( -4.031723327955644365, -13.82865651623139769, 46.99313739789381117 ) ) ;
#16585 = CIRCLE ( 'NONE', #14037, 69.99999999999998579 ) ;
#16586 = CARTESIAN_POINT ( 'NONE',  ( 3.869409319524869773, 14.12455301876681268, -48.96737585071113585 ) ) ;
#16587 = CARTESIAN_POINT ( 'NONE',  ( 199.0231033154536817, -19.99336494683761956, -0.6578043788800663760 ) ) ;
#16588 = DIRECTION ( 'NONE',  ( 0.000000000000000000, -1.000000000000000000, -0.000000000000000000 ) ) ;
#16589 = FILL_AREA_STYLE_COLOUR ( '', #5373 ) ;
#16590 = CARTESIAN_POINT ( 'NONE',  ( -188.3611024622156833, -23.46270902204734909, 43.02327292322546981 ) ) ;
#16591 =( BOUNDED_SURFACE ( )  B_SPLINE_SURFACE ( 3, 3, ( 
 ( #25261, #12883, #15132, #23263, #5039, #1040, #9141, #13269, #25393, #7144, #21391, #15260, #23389, #3164, #23509, #13388, #21515, #3288, #11385, #24162, #12051, #3676, #21899, #13772, #25906, #5666, #10060, #3953, #11784, #19904 ),
 ( #26179, #7919, #21769, #16036, #22044, #25773, #17629, #21638, #3542, #9792, #1952, #1688, #17895, #13514, #1422, #25646, #7523, #24023, #15631, #7392, #9923, #15503, #23633, #26043, #5537, #5802, #5938, #1555, #7780, #9523 ),
 ( #5412, #15896, #13909, #3817, #23756, #19639, #11920, #22179, #20042, #1821, #11513, #18029, #11642, #14045, #20170, #3412, #13643, #19764, #9660, #17764, #7647, #15761, #23890, #2218, #4478, #16573, #22703, #486, #24704, #20440 ),
 ( #12580, #4352, #2086, #18703, #82, #18570, #14447, #8320, #6458, #6587, #12314, #8593, #16703, #14311, #24835, #14574, #18296, #10193, #14176, #22445, #2345, #20840, #24569, #6325, #6074, #20309, #2615, #8192, #20710, #16308 ),
 ( #4225, #350, #8454, #12187, #10327, #18436, #4616, #24432, #22310, #14708, #211, #18166, #10457, #2476, #10588, #6199, #16445, #22841, #12712, #22574, #26313, #4086, #8056, #12444, #16172, #20573, #24307, #25364, #21483, #23233 ),
 ( #13115, #3010, #18974, #7119, #16842, #15361, #15229, #9249, #21105, #23360, #5137, #2885, #13242, #19231, #23484, #4748, #5259, #1011, #19102, #18840, #21236, #886, #8995, #9114, #8858, #13361, #1144, #10856, #25491, #4879 ),
 ( #16970, #10728, #25232, #8724, #618, #25106, #12983, #21367, #11117, #11237, #6855, #24975, #3135, #14972, #6724, #23107, #10993, #17099, #6984, #14836, #17225, #22969, #5010, #19355, #15099, #17356, #12854, #7240, #20972, #2753 ) ),
 .UNSPECIFIED., .T., .F., .T. ) 
 B_SPLINE_SURFACE_WITH_KNOTS ( ( 4, 3, 4 ),
 ( 4, 2, 2, 2, 2, 2, 2, 2, 2, 2, 2, 2, 2, 2, 4 ),
 ( 0.000000000000000000, 0.5000000000000000000, 1.000000000000000000 ),
 ( 0.000000000000000000, 0.1357259735107005372, 0.1651108541090157700, 0.1944957347073310028, 0.3598804999793158710, 0.3867117631979620773, 0.4135430264166082281, 0.5789277916885930964, 0.6062785021374117456, 0.6336292125862302838, 0.8508620842112317728, 0.8814014469398914198, 0.9119408096685510667, 0.9559704048342755334, 1.000000000000000000 ),
 .UNSPECIFIED. ) 
 GEOMETRIC_REPRESENTATION_ITEM ( )  RATIONAL_B_SPLINE_SURFACE ( (
 ( 1.000000000000000000, 1.000000000000000000, 1.000000000000000000, 1.000000000000000000, 1.000000000000000000, 1.000000000000000000, 1.000000000000000000, 1.000000000000000000, 1.000000000000000000, 1.000000000000000000, 1.000000000000000000, 1.000000000000000000, 1.000000000000000000, 1.000000000000000000, 1.000000000000000000, 1.000000000000000000, 1.000000000000000000, 1.000000000000000000, 1.000000000000000000, 1.000000000000000000, 1.000000000000000000, 1.000000000000000000, 1.000000000000000000, 1.000000000000000000, 1.000000000000000000, 1.000000000000000000, 1.000000000000000000, 1.000000000000000000, 1.000000000000000000, 1.000000000000000000),
 ( 0.3333333333333333703, 0.3333333333333333703, 0.3333333333333333703, 0.3333333333333333703, 0.3333333333333333703, 0.3333333333333333703, 0.3333333333333333703, 0.3333333333333333703, 0.3333333333333333703, 0.3333333333333333703, 0.3333333333333333703, 0.3333333333333333703, 0.3333333333333333703, 0.3333333333333333703, 0.3333333333333333703, 0.3333333333333333703, 0.3333333333333333703, 0.3333333333333333703, 0.3333333333333333703, 0.3333333333333333703, 0.3333333333333333703, 0.3333333333333333703, 0.3333333333333333703, 0.3333333333333333703, 0.3333333333333333703, 0.3333333333333333703, 0.3333333333333333703, 0.3333333333333333703, 0.3333333333333333703, 0.3333333333333333703),
 ( 0.3333333333333333703, 0.3333333333333333703, 0.3333333333333333703, 0.3333333333333333703, 0.3333333333333333703, 0.3333333333333333703, 0.3333333333333333703, 0.3333333333333333703, 0.3333333333333333703, 0.3333333333333333703, 0.3333333333333333703, 0.3333333333333333703, 0.3333333333333333703, 0.3333333333333333703, 0.3333333333333333703, 0.3333333333333333703, 0.3333333333333333703, 0.3333333333333333703, 0.3333333333333333703, 0.3333333333333333703, 0.3333333333333333703, 0.3333333333333333703, 0.3333333333333333703, 0.3333333333333333703, 0.3333333333333333703, 0.3333333333333333703, 0.3333333333333333703, 0.3333333333333333703, 0.3333333333333333703, 0.3333333333333333703),
 ( 1.000000000000000000, 1.000000000000000000, 1.000000000000000000, 1.000000000000000000, 1.000000000000000000, 1.000000000000000000, 1.000000000000000000, 1.000000000000000000, 1.000000000000000000, 1.000000000000000000, 1.000000000000000000, 1.000000000000000000, 1.000000000000000000, 1.000000000000000000, 1.000000000000000000, 1.000000000000000000, 1.000000000000000000, 1.000000000000000000, 1.000000000000000000, 1.000000000000000000, 1.000000000000000000, 1.000000000000000000, 1.000000000000000000, 1.000000000000000000, 1.000000000000000000, 1.000000000000000000, 1.000000000000000000, 1.000000000000000000, 1.000000000000000000, 1.000000000000000000),
 ( 0.3333333333333333703, 0.3333333333333333703, 0.3333333333333333703, 0.3333333333333333703, 0.3333333333333333703, 0.3333333333333333703, 0.3333333333333333703, 0.3333333333333333703, 0.3333333333333333703, 0.3333333333333333703, 0.3333333333333333703, 0.3333333333333333703, 0.3333333333333333703, 0.3333333333333333703, 0.3333333333333333703, 0.3333333333333333703, 0.3333333333333333703, 0.3333333333333333703, 0.3333333333333333703, 0.3333333333333333703, 0.3333333333333333703, 0.3333333333333333703, 0.3333333333333333703, 0.3333333333333333703, 0.3333333333333333703, 0.3333333333333333703, 0.3333333333333333703, 0.3333333333333333703, 0.3333333333333333703, 0.3333333333333333703),
 ( 0.3333333333333333703, 0.3333333333333333703, 0.3333333333333333703, 0.3333333333333333703, 0.3333333333333333703, 0.3333333333333333703, 0.3333333333333333703, 0.3333333333333333703, 0.3333333333333333703, 0.3333333333333333703, 0.3333333333333333703, 0.3333333333333333703, 0.3333333333333333703, 0.3333333333333333703, 0.3333333333333333703, 0.3333333333333333703, 0.3333333333333333703, 0.3333333333333333703, 0.3333333333333333703, 0.3333333333333333703, 0.3333333333333333703, 0.3333333333333333703, 0.3333333333333333703, 0.3333333333333333703, 0.3333333333333333703, 0.3333333333333333703, 0.3333333333333333703, 0.3333333333333333703, 0.3333333333333333703, 0.3333333333333333703),
 ( 1.000000000000000000, 1.000000000000000000, 1.000000000000000000, 1.000000000000000000, 1.000000000000000000, 1.000000000000000000, 1.000000000000000000, 1.000000000000000000, 1.000000000000000000, 1.000000000000000000, 1.000000000000000000, 1.000000000000000000, 1.000000000000000000, 1.000000000000000000, 1.000000000000000000, 1.000000000000000000, 1.000000000000000000, 1.000000000000000000, 1.000000000000000000, 1.000000000000000000, 1.000000000000000000, 1.000000000000000000, 1.000000000000000000, 1.000000000000000000, 1.000000000000000000, 1.000000000000000000, 1.000000000000000000, 1.000000000000000000, 1.000000000000000000, 1.000000000000000000) ) ) 
 REPRESENTATION_ITEM ( '' )  SURFACE ( )  );
#16592 = CARTESIAN_POINT ( 'NONE',  ( -100.7734535825088358, -16.03295912088728770, 16.03295912088687913 ) ) ;
#16593 = CARTESIAN_POINT ( 'NONE',  ( -162.0762913951020892, -1.694272876828353702, 0.000000000000000000 ) ) ;
#16595 = CARTESIAN_POINT ( 'NONE',  ( 163.1118516004056573, 9.006482792069759213, -9.006482792069505194 ) ) ;
#16594 = CARTESIAN_POINT ( 'NONE',  ( -188.2652746676673701, 13.82569223136002279, -46.97858116095154202 ) ) ;
#16596 = CARTESIAN_POINT ( 'NONE',  ( 4.995406935893289102, 10.78321810389013002, -10.78321810388986712 ) ) ;
#16597 = CARTESIAN_POINT ( 'NONE',  ( -192.9588430854689705, -54.46834944099975928, -2.449293598294708485E-15 ) ) ;
#16598 = CARTESIAN_POINT ( 'NONE',  ( -198.0356074513804572, 55.37879056873070027, 2.449293598294708485E-15 ) ) ;
#16599 = CARTESIAN_POINT ( 'NONE',  ( 170.2234770963711128, -40.00000000000024158, 24.55285855007145202 ) ) ;
#16600 = CARTESIAN_POINT ( 'NONE',  ( 91.82158438592158234, 16.11829626346139577, 16.11829626346143840 ) ) ;
#16601 = CARTESIAN_POINT ( 'NONE',  ( 98.29820294267349823, -4.524526698162719462, 19.49240851342997161 ) ) ;
#16602 = CARTESIAN_POINT ( 'NONE',  ( 170.2234770963711128, 45.64576402573196390, -10.92277846919159856 ) ) ;
#16603 = CARTESIAN_POINT ( 'NONE',  ( -238.4067589809705794, -0.6820004457913680929, 0.6820004457913170226 ) ) ;
#16604 = ORIENTED_EDGE ( 'NONE', *, *, #17195, .T. ) ;
#16605 = CARTESIAN_POINT ( 'NONE',  ( -280.0000000000000000, -14.14213562373098831, -14.14213562373098654 ) ) ;
#16606 = AXIS2_PLACEMENT_3D ( 'NONE', #26276, #38, #8014 ) ;
#16607 = CARTESIAN_POINT ( 'NONE',  ( -189.2428623074473535, -13.87687453620301348, -47.31877164625541354 ) ) ;
#16608 = CARTESIAN_POINT ( 'NONE',  ( -208.1127848780264742, -10.60833733268345469, 67.17687982760682530 ) ) ;
#16609 = CARTESIAN_POINT ( 'NONE',  ( -0.6848998192525614925, -43.87669161505422721, -24.09453515736277041 ) ) ;
#16610 = VERTEX_POINT ( 'NONE', #7668 ) ;
#16611 = CARTESIAN_POINT ( 'NONE',  ( 146.6084372240433993, -34.62501878078303008, 0.000000000000000000 ) ) ;
#16612 = DIRECTION ( 'NONE',  ( 0.000000000000000000, 1.000000000000000000, 0.000000000000000000 ) ) ;
#16613 = ORIENTED_EDGE ( 'NONE', *, *, #9469, .T. ) ;
#16614 = CARTESIAN_POINT ( 'NONE',  ( 200.0000000000002558, 17.05253901346626222, -8.385556056821480198 ) ) ;
#16615 = CARTESIAN_POINT ( 'NONE',  ( -315.0000000000000568, -4.857225732735059864E-14, 0.000000000000000000 ) ) ;
#16616 = CARTESIAN_POINT ( 'NONE',  ( -192.6563370916107374, -44.11756948123341715, -18.27409561805956173 ) ) ;
#16617 = EDGE_CURVE ( 'NONE', #20651, #24679, #12627, .T. ) ;
#16618 = CARTESIAN_POINT ( 'NONE',  ( -86.96347745069644475, -8.210974027862429531E-14, 18.24025645688352881 ) ) ;
#16619 = CARTESIAN_POINT ( 'NONE',  ( 146.6084372240433993, 5.374981219216999229, 2.449293598294708485E-15 ) ) ;
#16620 = CARTESIAN_POINT ( 'NONE',  ( -238.4067589809705794, -27.60227080167029001, -28.96627169325357798 ) ) ;
#16621 = FACE_OUTER_BOUND ( 'NONE', #22020, .T. ) ;
#16622 = AXIS2_PLACEMENT_3D ( 'NONE', #23508, #19506, #1290 ) ;
#16623 = ADVANCED_FACE ( 'NONE', ( #5684, #19787, #24927 ), #575, .F. ) ;
#16624 = AXIS2_PLACEMENT_3D ( 'NONE', #12533, #18659, #17062 ) ;
#16625 = CARTESIAN_POINT ( 'NONE',  ( 0.2972598230770030492, -1.921041075453695163E-13, 54.33493731733936016 ) ) ;
#16626 = CARTESIAN_POINT ( 'NONE',  ( -86.96347745069645896, 39.99999999999994316, 18.24025645688366737 ) ) ;
#16627 = LINE ( 'NONE', #669, #23612 ) ;
#16628 = CARTESIAN_POINT ( 'NONE',  ( -259.2033419157646676, 9.517827891722582478, -40.00000000000002132 ) ) ;
#16629 = EDGE_CURVE ( 'NONE', #12261, #21267, #6746, .T. ) ;
#16630 = CARTESIAN_POINT ( 'NONE',  ( 4.995406935893307754, -55.24977328853207581, -40.00000000000002132 ) ) ;
#16631 = EDGE_CURVE ( 'NONE', #21007, #8002, #17056, .T. ) ;
#16632 = CARTESIAN_POINT ( 'NONE',  ( -100.7734535825088500, 16.03295912088683295, 40.53558337403684675 ) ) ;
#16633 = CARTESIAN_POINT ( 'NONE',  ( -86.96347745069644475, -2.438961472018186339E-13, 21.75974354311649961 ) ) ;
#16634 = CARTESIAN_POINT ( 'NONE',  ( -114.4364955367320249, 20.04994829327449679, -8.644468109213075735 ) ) ;
#16635 = CARTESIAN_POINT ( 'NONE',  ( -192.9588430854689989, 5.375290060580374156E-13, -54.46834944099972375 ) ) ;
#16636 = CARTESIAN_POINT ( 'NONE',  ( -162.0762913951021176, -40.00000000000019895, 41.69427287672974813 ) ) ;
#16637 = CARTESIAN_POINT ( 'NONE',  ( 199.0261090282319856, -10.57113834583376644, 16.98461103275367634 ) ) ;
#16638 = DIRECTION ( 'NONE',  ( 0.000000000000000000, -1.000000000000000000, 0.000000000000000000 ) ) ;
#16639 = CARTESIAN_POINT ( 'NONE',  ( -114.4944481313176112, -9.302331659126325647, 19.81806240209552783 ) ) ;
#16640 = CARTESIAN_POINT ( 'NONE',  ( 184.8905102610680444, -13.49065550809780412, -43.07788698682583828 ) ) ;
#16641 = VERTEX_POINT ( 'NONE', #18523 ) ;
#16642 = CARTESIAN_POINT ( 'NONE',  ( -86.86493150571118349, -7.943527260495776510, -19.77569912839190280 ) ) ;
#16643 = CARTESIAN_POINT ( 'NONE',  ( 121.8740240556054459, 26.81399039734628076, -11.10671848392266092 ) ) ;
#16644 = CARTESIAN_POINT ( 'NONE',  ( -91.56559293963834989, -17.32597176626812896, -2.449293598294708485E-15 ) ) ;
#16645 = DIRECTION ( 'NONE',  ( -1.000000000000000000, 0.000000000000000000, 0.000000000000000000 ) ) ;
#16646 = CARTESIAN_POINT ( 'NONE',  ( -192.9588430854689989, 14.46834944099965981, 0.000000000000000000 ) ) ;
#16647 = ORIENTED_EDGE ( 'NONE', *, *, #17141, .T. ) ;
#16648 = ORIENTED_EDGE ( 'NONE', *, *, #3372, .T. ) ;
#16649 = VECTOR ( 'NONE', #964, 1000.000000000000000 ) ;
#16650 = CARTESIAN_POINT ( 'NONE',  ( -109.1264249741457348, 13.72187187126464991, 33.12752917268250741 ) ) ;
#16651 = CARTESIAN_POINT ( 'NONE',  ( -94.58360650938178082, 9.000712009840871275, -20.58386743644488703 ) ) ;
#16652 = CARTESIAN_POINT ( 'NONE',  ( 8.209392600932645223, 24.84362085273527043, 44.89226883836252568 ) ) ;
#16653 = EDGE_LOOP ( 'NONE', ( #8463, #15327, #5323, #20342 ) ) ;
#16654 = EDGE_LOOP ( 'NONE', ( #3420, #1377 ) ) ;
#16655 = CARTESIAN_POINT ( 'NONE',  ( 136.1360204305621266, -24.77266263493116583, -24.77266263493127951 ) ) ;
#16656 = CARTESIAN_POINT ( 'NONE',  ( 199.0244488197511998, -19.74721217248383809, 3.261676333419620821 ) ) ;
#16657 = CARTESIAN_POINT ( 'NONE',  ( -110.0471271033544269, -6.849398635777247613, 18.98461286765427758 ) ) ;
#16658 = FACE_OUTER_BOUND ( 'NONE', #328, .T. ) ;
#16659 = DIRECTION ( 'NONE',  ( 0.9698969544100265461, -0.09318942522532003281, -0.2249791742635964820 ) ) ;
#16660 = DIRECTION ( 'NONE',  ( 0.000000000000000000, 1.000000000000000000, 0.000000000000000000 ) ) ;
#16661 = DIRECTION ( 'NONE',  ( 0.000000000000000000, -1.000000000000000000, 0.000000000000000000 ) ) ;
#16662 = CARTESIAN_POINT ( 'NONE',  ( 151.7948205124836534, 39.99999999999970157, 33.23291073765595627 ) ) ;
#16663 = CARTESIAN_POINT ( 'NONE',  ( -56.48582580120560692, 39.99999999999991473, 9.153146818114004546 ) ) ;
#16664 = DIRECTION ( 'NONE',  ( 1.000000000000000000, 1.836970198721030181E-16, 0.000000000000000000 ) ) ;
#16665 = CIRCLE ( 'NONE', #24748, 6.000000000000019540 ) ;
#16666 = CARTESIAN_POINT ( 'NONE',  ( -86.86493150571116928, 8.366608963953661160, 19.60045294882771572 ) ) ;
#16667 = CARTESIAN_POINT ( 'NONE',  ( 199.0072342795740497, 19.67962538453564036, -3.556093180948044274 ) ) ;
#16668 = CARTESIAN_POINT ( 'NONE',  ( -188.6889827002360960, 23.53286111060924313, 43.11787295909677908 ) ) ;
#16669 = CARTESIAN_POINT ( 'NONE',  ( 14.38125909742181285, -10.73282306404712472, -10.73282306404731301 ) ) ;
#16670 = CARTESIAN_POINT ( 'NONE',  ( -96.93773665439030651, 9.001171854901906855, 20.58457565566410352 ) ) ;
#16671 = CARTESIAN_POINT ( 'NONE',  ( -135.8532207217289738, 6.472252184283881604, 50.09629031063969506 ) ) ;
#16672 = CARTESIAN_POINT ( 'NONE',  ( 98.29820294267865677, -17.41560179325844615, 10.21753654889059781 ) ) ;
#16673 = CARTESIAN_POINT ( 'NONE',  ( 136.1360204305621551, 24.77266263493153176, -31.79587985999237887 ) ) ;
#16674 = CARTESIAN_POINT ( 'NONE',  ( -200.0000000000000568, 47.66874763508950963, -16.05666331275189762 ) ) ;
#16675 = CARTESIAN_POINT ( 'NONE',  ( -30.26275506840324070, -1.694272468446265112, 0.000000000000000000 ) ) ;
#16676 = CARTESIAN_POINT ( 'NONE',  ( 170.2234770963711128, -17.36149277827010096, 17.36149277826970660 ) ) ;
#16677 = CARTESIAN_POINT ( 'NONE',  ( 14.38125909742181285, -15.17850393972633505, 0.000000000000000000 ) ) ;
#16678 = DIRECTION ( 'NONE',  ( 1.000000000000000000, 1.836970198721030427E-16, -0.000000000000000000 ) ) ;
#16679 = CARTESIAN_POINT ( 'NONE',  ( 0.2972598230770030492, 5.716321584140269555E-13, -54.33493731733936016 ) ) ;
#16680 = CARTESIAN_POINT ( 'NONE',  ( 199.0060826632022781, 7.907239936230238797, -18.36546223987650706 ) ) ;
#16681 = CARTESIAN_POINT ( 'NONE',  ( 130.8888609958233360, -12.21841679119747681, 29.49786752803523626 ) ) ;
#16682 = VERTEX_POINT ( 'NONE', #14792 ) ;
#16683 = ORIENTED_EDGE ( 'NONE', *, *, #2899, .F. ) ;
#16684 = CARTESIAN_POINT ( 'NONE',  ( -162.0762913951020892, 1.694272876828294194, 0.000000000000000000 ) ) ;
#16685 =( NAMED_UNIT ( * ) PLANE_ANGLE_UNIT ( ) SI_UNIT ( $, .RADIAN. ) );
#16686 = CARTESIAN_POINT ( 'NONE',  ( 130.8568914410475088, 32.49135343045448820, 24.07718906446946860 ) ) ;
#16687 = CARTESIAN_POINT ( 'NONE',  ( -105.2109270643573922, -21.45728911406257922, 1.359352815171848361 ) ) ;
#16688 = CARTESIAN_POINT ( 'NONE',  ( -138.9613193425325619, 10.11110876495220090, -29.42718875726376382 ) ) ;
#16689 = LINE ( 'NONE', #18283, #25342 ) ;
#16690 = CARTESIAN_POINT ( 'NONE',  ( 200.0000000000001990, 0.6082288760829889229, -18.99424756986708474 ) ) ;
#16691 = CARTESIAN_POINT ( 'NONE',  ( 199.9999999999999716, -4.015339075642541111, -18.57593938989771587 ) ) ;
#16692 = CARTESIAN_POINT ( 'NONE',  ( 184.8905102610680444, -14.79361573936330565, -41.77492675556016621 ) ) ;
#16693 = CARTESIAN_POINT ( 'NONE',  ( -135.8532207217289738, 6.472252184284096543, 6.472252184284234211 ) ) ;
#16694 = DIRECTION ( 'NONE',  ( 0.000000000000000000, 0.3995982397861173041, -0.9166903767138807613 ) ) ;
#16695 = CARTESIAN_POINT ( 'NONE',  ( 163.1118516004056573, -2.556006622855449647E-13, 27.26290988616872824 ) ) ;
#16696 = CARTESIAN_POINT ( 'NONE',  ( 19.06497207195981147, -10.03556273973425483, -10.03556273973443247 ) ) ;
#16697 = EDGE_CURVE ( 'NONE', #25993, #6082, #19056, .T. ) ;
#16698 = CARTESIAN_POINT ( 'NONE',  ( 22.40986519363267959, 13.85314893102515477, 47.15972762675168894 ) ) ;
#16699 = CARTESIAN_POINT ( 'NONE',  ( -210.0000000000000284, 66.50000000000009948, 66.50000000000005684 ) ) ;
#16700 = CARTESIAN_POINT ( 'NONE',  ( -86.96347745069644475, -12.89780903124413491, 12.89780903124398037 ) ) ;
#16701 = CARTESIAN_POINT ( 'NONE',  ( 199.0079644305843090, 19.95293258044705098, -1.355764268682818408 ) ) ;
#16703 = CARTESIAN_POINT ( 'NONE',  ( -86.96347745069644475, -8.210974027862429531E-14, 18.24025645688352881 ) ) ;
#16702 = CARTESIAN_POINT ( 'NONE',  ( -192.9588430854690273, -18.05360324515400094, -38.51493924976961836 ) ) ;
#16704 = CARTESIAN_POINT ( 'NONE',  ( 170.2234770963711128, 10.92277846919147066, 45.64576402573197811 ) ) ;
#16705 = CARTESIAN_POINT ( 'NONE',  ( 21.60666276258112717, 43.47550165074678574, -18.00814241470989430 ) ) ;
#16706 = CARTESIAN_POINT ( 'NONE',  ( 0.2972598230769930572, 14.33493731733933352, 0.000000000000000000 ) ) ;
#16707 = CARTESIAN_POINT ( 'NONE',  ( -162.0762913951021176, -27.08623940707624911, 29.48230308784761888 ) ) ;
#16708 = CARTESIAN_POINT ( 'NONE',  ( 14.38125909742180752, 55.17850393974265444, 40.00000000000002132 ) ) ;
#16709 = CARTESIAN_POINT ( 'NONE',  ( -39.84211263202143272, -32.75097567523309294, 13.56589830563916088 ) ) ;
#16710 = CARTESIAN_POINT ( 'NONE',  ( 200.0000000000000000, 19.99999999999995737, 40.00000000000002132 ) ) ;
#16711 = EDGE_CURVE ( 'NONE', #13429, #3360, #15319, .T. ) ;
#16712 = ORIENTED_EDGE ( 'NONE', *, *, #8737, .T. ) ;
#16713 = DIRECTION ( 'NONE',  ( 0.000000000000000000, 0.000000000000000000, 1.000000000000000000 ) ) ;
#16714 = CARTESIAN_POINT ( 'NONE',  ( 184.8905102610680444, -14.79361573936379415, -14.79361573936387941 ) ) ;
#16715 = CARTESIAN_POINT ( 'NONE',  ( -4.151555265633880332, -13.82020782288870109, 46.95165237382999379 ) ) ;
#16716 = CARTESIAN_POINT ( 'NONE',  ( -3.921555385250235393, 13.83441994316400958, -47.03297225793206593 ) ) ;
#16717 = CARTESIAN_POINT ( 'NONE',  ( 199.9999999999995453, -10.04557064260861843, 16.14007440661455206 ) ) ;
#16718 = CARTESIAN_POINT ( 'NONE',  ( -86.96347745069644475, 12.89780903124349898, 43.67073346367994446 ) ) ;
#16719 = LINE ( 'NONE', #10744, #724 ) ;
#16720 = CARTESIAN_POINT ( 'NONE',  ( 190.0000000000000000, 66.50000000000009948, 66.50000000000005684 ) ) ;
#16721 = CARTESIAN_POINT ( 'NONE',  ( -190.5535808404529234, -18.10342626500561991, 43.70553721439956263 ) ) ;
#16722 = CARTESIAN_POINT ( 'NONE',  ( 136.1360204305621266, -3.419521671106983309E-13, 35.03383547441296741 ) ) ;
#16723 = ADVANCED_FACE ( 'NONE', ( #6413 ), #10683, .T. ) ;
#16724 = CARTESIAN_POINT ( 'NONE',  ( 130.8568914410475088, -52.36146031193413108, -4.207082182990267150 ) ) ;
#16725 = CARTESIAN_POINT ( 'NONE',  ( 136.1360204305621266, 24.77266263493104148, 24.77266263493145004 ) ) ;
#16727 = CARTESIAN_POINT ( 'NONE',  ( -56.48582580120559982, 50.09629031063956717, 6.472252184284792875 ) ) ;
#16726 = CARTESIAN_POINT ( 'NONE',  ( -200.5022929845067949, 18.58571294254510065, -44.86988025226708743 ) ) ;
#16728 = CARTESIAN_POINT ( 'NONE',  ( -105.3755690713226727, -15.38646221621807619, 15.38646221621768362 ) ) ;
#16729 = CARTESIAN_POINT ( 'NONE',  ( 0.2972598230770130412, -54.33493731733936016, -2.449293598294708485E-15 ) ) ;
#16730 = CARTESIAN_POINT ( 'NONE',  ( 14.38125909742180752, 55.17850393974265444, 40.00000000000002132 ) ) ;
#16731 = CARTESIAN_POINT ( 'NONE',  ( -208.1127848780264742, -39.99999999999990763, -15.00245453012711394 ) ) ;
#16732 = CARTESIAN_POINT ( 'NONE',  ( -100.7734535825088500, 12.25131212657490209, -44.31723036834897300 ) ) ;
#16733 = DIRECTION ( 'NONE',  ( 0.000000000000000000, 0.000000000000000000, -1.000000000000000000 ) ) ;
#16734 = CARTESIAN_POINT ( 'NONE',  ( 170.2234770963711128, 17.36149277827028925, -39.20704971665377059 ) ) ;
#16735 = CARTESIAN_POINT ( 'NONE',  ( 184.8905102610680444, 43.07788698682572459, 13.49065550809829439 ) ) ;
#16736 = VERTEX_POINT ( 'NONE', #12668 ) ;
#16737 = CARTESIAN_POINT ( 'NONE',  ( -213.1075012329537230, 9.698598906462684965, 66.26714140138669507 ) ) ;
#16738 = CARTESIAN_POINT ( 'NONE',  ( -88.37877758188305677, 8.026456973721797894, 20.15391234940723564 ) ) ;
#16739 = CARTESIAN_POINT ( 'NONE',  ( -238.4067589809705794, 27.60227080167040370, 28.96627169325338613 ) ) ;
#16740 = CARTESIAN_POINT ( 'NONE',  ( -3.443169733045819303, -43.30433998020570385, -17.93724492941698401 ) ) ;
#16741 = ORIENTED_EDGE ( 'NONE', *, *, #117, .T. ) ;
#16742 = CARTESIAN_POINT ( 'NONE',  ( -1.828631717626211906, -47.79123445063621745, -13.94691770768551287 ) ) ;
#16743 = FACE_OUTER_BOUND ( 'NONE', #792, .T. ) ;
#16744 = ORIENTED_EDGE ( 'NONE', *, *, #4366, .T. ) ;
#16745 = CARTESIAN_POINT ( 'NONE',  ( 199.9999999999998579, 15.71915069317562264, -10.67410001769982308 ) ) ;
#16746 = CARTESIAN_POINT ( 'NONE',  ( -114.7537493279903202, -21.97305528828601595, -2.780162309559761180 ) ) ;
#16747 =( BOUNDED_CURVE ( )  B_SPLINE_CURVE ( 3, ( #2328, #16429, #8177, #8439, #10439, #10572, #24686 ),
 .UNSPECIFIED., .F., .F. ) 
 B_SPLINE_CURVE_WITH_KNOTS ( ( 4, 3, 4 ),
 ( 0.007504510840757329035, 0.02318599846099227146, 0.03886748608123005710 ),
 .UNSPECIFIED. ) 
 CURVE ( )  GEOMETRIC_REPRESENTATION_ITEM ( )  RATIONAL_B_SPLINE_CURVE ( ( 0.5852718452494382051, 0.6660804010233934980, 0.8043231192735807999, 1.000000000000000000, 0.8043231192735453838, 0.6660804010233435379, 0.5852718452493943513 ) ) 
 REPRESENTATION_ITEM ( '' )  );
#16748 = CARTESIAN_POINT ( 'NONE',  ( 136.1360204305621551, 4.966164525587085876, 40.00000000000002132 ) ) ;
#16749 = CARTESIAN_POINT ( 'NONE',  ( 19.06497207195980792, -18.24870850772710540, -38.31983398719647482 ) ) ;
#16750 = CARTESIAN_POINT ( 'NONE',  ( 199.0160554649137907, 14.01242985958090692, 14.27167877623515757 ) ) ;
#16751 = CARTESIAN_POINT ( 'NONE',  ( -198.0356074513804572, -39.15871834505931304, 17.40982414986437377 ) ) ;
#16752 = CARTESIAN_POINT ( 'NONE',  ( -208.1127848780264742, 39.99999999999979394, 55.00245453010936103 ) ) ;
#16753 = CARTESIAN_POINT ( 'NONE',  ( 91.82158438592156813, 40.00000000000009948, -17.20528682183286051 ) ) ;
#16754 = CARTESIAN_POINT ( 'NONE',  ( 180.0000000000000000, 2.292407966645821729E-14, -82.49999999999998579 ) ) ;
#16755 = CARTESIAN_POINT ( 'NONE',  ( -198.0356074513804572, -15.37879056873074290, -40.00000000000002132 ) ) ;
#16756 = CARTESIAN_POINT ( 'NONE',  ( -726.9846540392142060, -52.49999999999991473, 52.49999999999999289 ) ) ;
#16757 = CARTESIAN_POINT ( 'NONE',  ( -105.3755690713226727, -18.24025645688354302, -2.449293598294708485E-15 ) ) ;
#16758 = CARTESIAN_POINT ( 'NONE',  ( 200.0000000000000000, 14.14213562373083022, 42.42640687119289566 ) ) ;
#16759 = CARTESIAN_POINT ( 'NONE',  ( 104.1600437297060893, -8.548029202226684831, -20.63676802882099892 ) ) ;
#16760 = CARTESIAN_POINT ( 'NONE',  ( -105.2833435977142500, 11.73665196259849708, -17.94452063501608663 ) ) ;
#16761 = CARTESIAN_POINT ( 'NONE',  ( 130.8568914410475088, 39.99999999999969447, 34.05028731879830417 ) ) ;
#16762 = CARTESIAN_POINT ( 'NONE',  ( -280.0000000000000000, -1.237140859393462838E-13, 20.00000000000001421 ) ) ;
#16763 = CARTESIAN_POINT ( 'NONE',  ( 199.0263771359574889, -13.68429728450633753, 14.60718570525551563 ) ) ;
#16764 = DIRECTION ( 'NONE',  ( 0.9352143328345496887, -0.1355013631513355687, 0.3271292286619436052 ) ) ;
#16765 = CYLINDRICAL_SURFACE ( 'NONE', #22086, 4.999999999999997335 ) ;
#16766 = CARTESIAN_POINT ( 'NONE',  ( -30.26275506840322294, -57.76657404653985139, 1.198031551615709844 ) ) ;
#16767 = ORIENTED_EDGE ( 'NONE', *, *, #7337, .F. ) ;
#16769 = CARTESIAN_POINT ( 'NONE',  ( -40.07203023074529114, 32.10811084139960059, -16.33025453620214051 ) ) ;
#16768 = CARTESIAN_POINT ( 'NONE',  ( -77.65678946166498520, -4.464169626397992197, -21.58828686264906693 ) ) ;
#16770 = DIRECTION ( 'NONE',  ( 0.000000000000000000, 1.000000000000000000, 0.000000000000000000 ) ) ;
#16771 = CARTESIAN_POINT ( 'NONE',  ( -259.2033419157646676, -30.48217210827743884, -40.00000000000002132 ) ) ;
#16772 = EDGE_CURVE ( 'NONE', #12655, #14180, #10542, .T. ) ;
#16773 = CARTESIAN_POINT ( 'NONE',  ( -87.01701082927776554, -5.374668562248246850, -20.73853774320201637 ) ) ;
#16774 = CARTESIAN_POINT ( 'NONE',  ( -280.0000000000000000, -14.14213562373118549, 14.14213562373078936 ) ) ;
#16775 = ORIENTED_EDGE ( 'NONE', *, *, #13523, .T. ) ;
#16776 = ORIENTED_EDGE ( 'NONE', *, *, #22503, .F. ) ;
#16777 = DIRECTION ( 'NONE',  ( 0.000000000000000000, 1.000000000000000000, 0.000000000000000000 ) ) ;
#16778 = CARTESIAN_POINT ( 'NONE',  ( -105.4732637872226633, 8.153770687239410009, -19.68494377761406611 ) ) ;
#16779 = CARTESIAN_POINT ( 'NONE',  ( 8.273828130718225538, 18.58906013840518057, 44.87796109789316290 ) ) ;
#16780 = EDGE_CURVE ( 'NONE', #17459, #3571, #4834, .T. ) ;
#16781 = EDGE_LOOP ( 'NONE', ( #5871, #17713, #15548, #26081 ) ) ;
#16782 = ORIENTED_EDGE ( 'NONE', *, *, #15616, .T. ) ;
#16783 = CARTESIAN_POINT ( 'NONE',  ( 163.1118516004056573, -47.56205970284957374, 9.006482792074162802 ) ) ;
#16784 = CARTESIAN_POINT ( 'NONE',  ( 199.0147604500337764, -12.44374936594963899, -15.65999889774876941 ) ) ;
#16785 = CARTESIAN_POINT ( 'NONE',  ( -105.2053629887847421, 0.6703845944306704441, 21.49364769381508822 ) ) ;
#16786 = EDGE_CURVE ( 'NONE', #20259, #495, #3237, .T. ) ;
#16787 = CARTESIAN_POINT ( 'NONE',  ( 0.2972598230769990524, -18.14793986248724522, 38.42060263243662632 ) ) ;
#16788 = CYLINDRICAL_SURFACE ( 'NONE', #2594, 5.000000000000004441 ) ;
#16789 = CARTESIAN_POINT ( 'NONE',  ( 146.6084372240433709, 40.00000000000003553, 5.374981219217116468 ) ) ;
#16790 = CARTESIAN_POINT ( 'NONE',  ( -90.07798792367796636, 6.122142489605069318E-14, -22.27377874500495381 ) ) ;
#16791 = CARTESIAN_POINT ( 'NONE',  ( -200.0000000000000000, 75.00000000000000000, 0.000000000000000000 ) ) ;
#16792 = CARTESIAN_POINT ( 'NONE',  ( -162.0762913951020892, 4.094006889353306706E-13, -41.69427287682835015 ) ) ;
#16793 = AXIS2_PLACEMENT_3D ( 'NONE', #19422, #13427, #5078 ) ;
#16794 = CARTESIAN_POINT ( 'NONE',  ( -213.1075012329537230, 40.00000000000012790, -13.71589010951869980 ) ) ;
#16795 = CARTESIAN_POINT ( 'NONE',  ( -648.7609290488377383, 34.26580538984126179, 20.64023319344268970 ) ) ;
#16796 = FACE_OUTER_BOUND ( 'NONE', #2832, .T. ) ;
#16797 = CARTESIAN_POINT ( 'NONE',  ( 199.0123267138131098, 18.14094429105657369, 8.417911433729377890 ) ) ;
#16798 = CARTESIAN_POINT ( 'NONE',  ( -174.2681662550721171, 16.26527976854427493, 39.26785901291280112 ) ) ;
#16799 = CARTESIAN_POINT ( 'NONE',  ( -86.96347745069645896, -12.89780903124443689, 43.67073346367968156 ) ) ;
#16800 = DIRECTION ( 'NONE',  ( 0.000000000000000000, 0.000000000000000000, -1.000000000000000000 ) ) ;
#16801 = CARTESIAN_POINT ( 'NONE',  ( 184.8905102610680444, 14.79361573936366092, 41.77492675556006674 ) ) ;
#16802 = DIRECTION ( 'NONE',  ( 1.000000000000000000, 1.836970198721030427E-16, -0.000000000000000000 ) ) ;
#16803 = CIRCLE ( 'NONE', #18508, 31.79780246617542616 ) ;
#16804 = AXIS2_PLACEMENT_3D ( 'NONE', #15859, #22009, #5767 ) ;
#16805 = CARTESIAN_POINT ( 'NONE',  ( 184.8905102610680444, 43.07788698682591644, -13.49065550809769221 ) ) ;
#16806 = CARTESIAN_POINT ( 'NONE',  ( -659.5461728292011685, 43.13043488670722780, 12.84875797882843962 ) ) ;
#16807 = CARTESIAN_POINT ( 'NONE',  ( 199.9999999999999432, 20.00000000000013856, 0.000000000000000000 ) ) ;
#16808 = CARTESIAN_POINT ( 'NONE',  ( -86.96347745069644475, 12.89780903124349898, 43.67073346367994446 ) ) ;
#16809 = CARTESIAN_POINT ( 'NONE',  ( 170.2234770963711128, -15.44714144992813409, 40.00000000000002132 ) ) ;
#16810 = CARTESIAN_POINT ( 'NONE',  ( -600.9160842859510012, 38.46169296933204862, -23.38072629326452301 ) ) ;
#16811 = VERTEX_POINT ( 'NONE', #6544 ) ;
#16812 = CARTESIAN_POINT ( 'NONE',  ( -56.48582580120558561, 3.151766524733697544E-13, -30.84685318188644132 ) ) ;
#16813 = DIRECTION ( 'NONE',  ( 1.000000000000000000, -1.937599346585394162E-16, -0.000000000000000000 ) ) ;
#16814 = CARTESIAN_POINT ( 'NONE',  ( 156.5537079553356818, -11.28159757857240919, 27.23618587942422309 ) ) ;
#16815 = ORIENTED_EDGE ( 'NONE', *, *, #19870, .F. ) ;
#16816 = ORIENTED_EDGE ( 'NONE', *, *, #24953, .F. ) ;
#16817 = CARTESIAN_POINT ( 'NONE',  ( 19.06497207195980792, 54.19242893257844429, 40.00000000000002132 ) ) ;
#16818 = EDGE_CURVE ( 'NONE', #12261, #15079, #21499, .T. ) ;
#16819 = SURFACE_STYLE_USAGE ( .BOTH. , #19087 ) ;
#16820 = AXIS2_PLACEMENT_3D ( 'NONE', #19242, #23372, #25502 ) ;
#16821 = CIRCLE ( 'NONE', #11714, 10.00000000000000000 ) ;
#16822 = CARTESIAN_POINT ( 'NONE',  ( -110.0368417077420986, -18.74474319001871336, 7.441767003031916516 ) ) ;
#16823 = B_SPLINE_CURVE_WITH_KNOTS ( 'NONE', 3,
 ( #8533, #828, #19175, #6665, #959, #22911 ),
 .UNSPECIFIED., .F., .F.,
 ( 4, 2, 4 ),
 ( -0.0001324603514649706955, 0.04003639359266478182, 0.08020524753679453278 ),
 .UNSPECIFIED. ) ;
#16824 = CARTESIAN_POINT ( 'NONE',  ( 165.3321726437878283, -18.76308274334254378, -18.76308274334263615 ) ) ;
#16825 = CARTESIAN_POINT ( 'NONE',  ( -198.0012279766650352, 14.15883993157184761, -49.19397028317932552 ) ) ;
#16826 = CARTESIAN_POINT ( 'NONE',  ( 199.9999999999998010, 6.097523047862603462, -17.99825575681430223 ) ) ;
#16827 = VECTOR ( 'NONE', #21091, 1000.000000000000000 ) ;
#16828 = CARTESIAN_POINT ( 'NONE',  ( 199.9999999999999716, -7.851927509958055218, -17.31649898218073957 ) ) ;
#16829 = VECTOR ( 'NONE', #14415, 1000.000000000000000 ) ;
#16830 = CARTESIAN_POINT ( 'NONE',  ( 14.38125909742181463, 10.73282306403652875, -67.30136555895941797 ) ) ;
#16831 = CARTESIAN_POINT ( 'NONE',  ( 192.4448373802101173, -14.14213562370342281, 42.42640687122062104 ) ) ;
#16832 = B_SPLINE_CURVE_WITH_KNOTS ( 'NONE', 3,
 ( #20426, #22296, #12699, #6444, #16825, #18824 ),
 .UNSPECIFIED., .F., .F.,
 ( 4, 2, 4 ),
 ( -5.998616621412680422E-08, 0.005995031700373287635, 0.01199012338691278837 ),
 .UNSPECIFIED. ) ;
#16833 = CARTESIAN_POINT ( 'NONE',  ( -105.3174728402125453, -18.50892203404854897, -10.86052875576579346 ) ) ;
#16834 = CARTESIAN_POINT ( 'NONE',  ( 151.7948205124836250, -3.202120068677277203E-13, 33.23291073765553705 ) ) ;
#16835 = CIRCLE ( 'NONE', #5364, 14.99999999999999822 ) ;
#16836 = CARTESIAN_POINT ( 'NONE',  ( -238.4067589809705794, -0.6820004457913585449, -0.6820004457913265705 ) ) ;
#16837 = LINE ( 'NONE', #879, #2367 ) ;
#16838 = CARTESIAN_POINT ( 'NONE',  ( -188.2995950289364089, -23.44932284465861727, -43.00522595870986464 ) ) ;
#16839 = CARTESIAN_POINT ( 'NONE',  ( 4.995406935893305977, -39.06748935135212264, 39.06748935135171763 ) ) ;
#16840 = CARTESIAN_POINT ( 'NONE',  ( 199.0058351560425365, 17.78440418358302111, -9.144608015618983288 ) ) ;
#16842 = CARTESIAN_POINT ( 'NONE',  ( -208.1127848780264742, 39.99999999999992895, 15.00245453012683683 ) ) ;
#16841 = CARTESIAN_POINT ( 'NONE',  ( -162.0762913951020892, 1.198031840385732849, -1.198031840385733515 ) ) ;
#16843 = CARTESIAN_POINT ( 'NONE',  ( 44.82887508604880367, 36.15717056697129550, -18.94256811184066081 ) ) ;
#16844 = CARTESIAN_POINT ( 'NONE',  ( -280.0000000000000000, -20.00000000000006750, 0.000000000000000000 ) ) ;
#16845 = CARTESIAN_POINT ( 'NONE',  ( 170.2234770963711128, -17.36149277826985937, -17.36149277826995174 ) ) ;
#16846 = CARTESIAN_POINT ( 'NONE',  ( 91.82158438592158234, -17.20528682183298486, 0.000000000000000000 ) ) ;
#16847 = ORIENTED_EDGE ( 'NONE', *, *, #26231, .T. ) ;
#16848 = CARTESIAN_POINT ( 'NONE',  ( 9.006212071516715767, -49.32687279762742349, 14.17897189020562188 ) ) ;
#16849 = CARTESIAN_POINT ( 'NONE',  ( 184.8905102610680444, -20.92133201514440799, 40.00000000000002132 ) ) ;
#16850 = AXIS2_PLACEMENT_3D ( 'NONE', #12870, #770, #4766 ) ;
#16851 = ORIENTED_EDGE ( 'NONE', *, *, #16147, .F. ) ;
#16852 = CARTESIAN_POINT ( 'NONE',  ( 23.37394308801978937, 23.33966569535129310, -42.85717664514559999 ) ) ;
#16853 = AXIS2_PLACEMENT_3D ( 'NONE', #10041, #24417, #9907 ) ;
#16854 = CARTESIAN_POINT ( 'NONE',  ( 14.38125909742181285, -17.55144818341476309, 39.01709431150910490 ) ) ;
#16855 = CARTESIAN_POINT ( 'NONE',  ( -39.58644176656172675, -13.59899295350269810, 32.83087322326096569 ) ) ;
#16856 = CARTESIAN_POINT ( 'NONE',  ( 8.602182264176247983, 18.59145335917338926, -44.88373884391542390 ) ) ;
#16857 = CARTESIAN_POINT ( 'NONE',  ( 199.0263189878286028, -15.57072488730636017, 12.56115478513486217 ) ) ;
#16858 = CARTESIAN_POINT ( 'NONE',  ( 4.995406935893283773, 39.06748935135171052, 17.50105314357239195 ) ) ;
#16859 = CARTESIAN_POINT ( 'NONE',  ( -315.0000000000000568, -4.857225732735059864E-14, 0.000000000000000000 ) ) ;
#16860 = CARTESIAN_POINT ( 'NONE',  ( -189.0540493709916632, -17.95404051684981894, 43.34488811517340423 ) ) ;
#16861 = CARTESIAN_POINT ( 'NONE',  ( 14.38125909742181108, 1.616281842095393922E-13, -15.17850393972633682 ) ) ;
#16862 = CARTESIAN_POINT ( 'NONE',  ( -213.1075012329537230, -9.698598906450557777, 9.698598906450415669 ) ) ;
#16863 = CARTESIAN_POINT ( 'NONE',  ( 4.995406935893297984, 10.78321810390233892, -67.35176059882522281 ) ) ;
#16864 = CARTESIAN_POINT ( 'NONE',  ( 199.9999999999999432, 14.14213562373093680, 14.14213562373114641 ) ) ;
#16866 = CARTESIAN_POINT ( 'NONE',  ( -30.26275506840325136, 57.76657404653985139, -1.198031551615314161 ) ) ;
#16865 = CARTESIAN_POINT ( 'NONE',  ( -199.9999999999999716, 82.50000000000008527, -52.49999999999977973 ) ) ;
#16867 = CARTESIAN_POINT ( 'NONE',  ( -213.1075012329537230, 66.26714140138673770, -9.698598906462034819 ) ) ;
#16868 = CARTESIAN_POINT ( 'NONE',  ( -280.0000000000000568, 19.99999999999996092, 40.00000000000002132 ) ) ;
#16869 = CARTESIAN_POINT ( 'NONE',  ( -135.8532207217289738, -9.153146818113595984, -40.00000000000002132 ) ) ;
#16870 = CARTESIAN_POINT ( 'NONE',  ( 0.2972598230769938343, 10.13633138497472252, 10.13633138497475628 ) ) ;
#16871 = CARTESIAN_POINT ( 'NONE',  ( 200.0000000000000000, 52.49999999999987210, -82.49999999999998579 ) ) ;
#16872 = CARTESIAN_POINT ( 'NONE',  ( -135.8532207217289738, -21.81201906317757633, -21.81201906317793515 ) ) ;
#16873 = CARTESIAN_POINT ( 'NONE',  ( -4.039451493210501454, 43.00522595894040734, -23.44932283416630270 ) ) ;
#16874 = ORIENTED_EDGE ( 'NONE', *, *, #1024, .T. ) ;
#16875 = CARTESIAN_POINT ( 'NONE',  ( -192.9588430854690273, 10.23066800231970319, 66.79921049724369198 ) ) ;
#16876 = CARTESIAN_POINT ( 'NONE',  ( -87.13361725312203987, -16.15936047674203024, -14.23663594861907988 ) ) ;
#16877 = CARTESIAN_POINT ( 'NONE',  ( 163.1118516004056573, -9.006482792069636645, 9.006482792069567367 ) ) ;
#16878 = CARTESIAN_POINT ( 'NONE',  ( 3.869409319523309687, -48.96737585071549148, -14.12455301876188507 ) ) ;
#16879 = ORIENTED_EDGE ( 'NONE', *, *, #5900, .F. ) ;
#16880 = CARTESIAN_POINT ( 'NONE',  ( 130.8568914410475372, -34.05028731879786363, 0.000000000000000000 ) ) ;
#16881 = CARTESIAN_POINT ( 'NONE',  ( -105.4741150117383341, -8.366608964593364561, -19.60045294982747777 ) ) ;
#16882 = ADVANCED_FACE ( 'NONE', ( #25189 ), #6938, .F. ) ;
#16883 = CARTESIAN_POINT ( 'NONE',  ( 199.9999999999999716, 14.88808753490056880, -11.80862348214050606 ) ) ;
#16884 = CARTESIAN_POINT ( 'NONE',  ( -114.7252611291634139, -21.81972725943360913, 3.452297386453273109 ) ) ;
#16885 = CARTESIAN_POINT ( 'NONE',  ( 170.2234770963711128, 15.44714144992819094, 2.449293598294708485E-15 ) ) ;
#16886 = CARTESIAN_POINT ( 'NONE',  ( -106.9675868842832358, 19.33814434321038078, 8.010121658085223473 ) ) ;
#16887 = CARTESIAN_POINT ( 'NONE',  ( 199.0151032989660678, 15.24552994868030531, 12.94849756636627447 ) ) ;
#16888 = CARTESIAN_POINT ( 'NONE',  ( 57.59792236341148453, -54.84617931850879557, 1.722363176414566155 ) ) ;
#16889 = CARTESIAN_POINT ( 'NONE',  ( -86.96347745069645896, 39.99999999999994316, 18.24025645688366737 ) ) ;
#16890 = CARTESIAN_POINT ( 'NONE',  ( -135.8532207217289738, 40.00000000000002842, -9.153146818113432559 ) ) ;
#16891 = CARTESIAN_POINT ( 'NONE',  ( 200.0000000000000000, 69.29737539576909455, -75.30386416458597409 ) ) ;
#16892 = CARTESIAN_POINT ( 'NONE',  ( 4.995406935893307754, -55.24977328854835434, -2.449293598294708485E-15 ) ) ;
#16894 = CARTESIAN_POINT ( 'NONE',  ( 190.0000000000000000, 82.50000000000008527, 52.49999999999979394 ) ) ;
#16893 = CARTESIAN_POINT ( 'NONE',  ( 23.64688638900294038, -13.78084749393264907, -46.70960658758787076 ) ) ;
#16895 = CARTESIAN_POINT ( 'NONE',  ( -56.48582580120557850, -30.84685318188645198, -2.449293598294708485E-15 ) ) ;
#16896 = CARTESIAN_POINT ( 'NONE',  ( -105.3755690713226727, -12.89780903124413847, 12.89780903124398037 ) ) ;
#16897 = CARTESIAN_POINT ( 'NONE',  ( 149.5797498300189261, -12.18602109748318441, -29.41965740490883263 ) ) ;
#16898 = CARTESIAN_POINT ( 'NONE',  ( -114.7538884075326564, 13.57382480621628673, -17.50182194317628515 ) ) ;
#16899 = CARTESIAN_POINT ( 'NONE',  ( -100.7734535825088500, 40.00000000000017764, -17.32597176626768487 ) ) ;
#16900 = CARTESIAN_POINT ( 'NONE',  ( -280.0000000000000000, -14.14213562373098831, -14.14213562373098654 ) ) ;
#16901 = CARTESIAN_POINT ( 'NONE',  ( -126.6834156231682300, -24.89646324320138859, -9.107266674873804035 ) ) ;
#16902 = LINE ( 'NONE', #2542, #22951 ) ;
#16903 = CARTESIAN_POINT ( 'NONE',  ( -162.0762913951020892, -57.76657433524000851, 1.198031840315820329 ) ) ;
#16904 = ORIENTED_EDGE ( 'NONE', *, *, #17112, .T. ) ;
#16906 = CARTESIAN_POINT ( 'NONE',  ( -70.35386311717272179, 23.12931224224253768, -8.707385196623391721 ) ) ;
#16905 = CARTESIAN_POINT ( 'NONE',  ( 146.6084372240433993, 24.48358557860307272, 24.48358557860347418 ) ) ;
#16907 = CARTESIAN_POINT ( 'NONE',  ( -109.1264249741437027, -13.72187187123250673, 33.12752917269451558 ) ) ;
#16908 = CARTESIAN_POINT ( 'NONE',  ( -280.0000000000000000, -20.00000000000006750, -2.449293598294708485E-15 ) ) ;
#16909 = CARTESIAN_POINT ( 'NONE',  ( -105.4288990061682654, 9.009177719101042925, 19.35827336168831891 ) ) ;
#16910 = CARTESIAN_POINT ( 'NONE',  ( -362.0709805440841365, -4.504554366608264653E-14, -28.79780246617542616 ) ) ;
#16911 = ORIENTED_EDGE ( 'NONE', *, *, #2240, .F. ) ;
#16912 = ORIENTED_EDGE ( 'NONE', *, *, #4305, .F. ) ;
#16913 = CARTESIAN_POINT ( 'NONE',  ( 199.9999999999999716, 2.469089442616056562, 18.84997742926038455 ) ) ;
#16914 = CARTESIAN_POINT ( 'NONE',  ( -89.91498783729078070, 8.087768383257817106, -20.43892340018621212 ) ) ;
#16915 = ORIENTED_EDGE ( 'NONE', *, *, #20205, .F. ) ;
#16916 = ORIENTED_EDGE ( 'NONE', *, *, #4782, .T. ) ;
#16917 =( BOUNDED_CURVE ( )  B_SPLINE_CURVE ( 3, ( #18782, #829, #6929, #15046 ),
 .UNSPECIFIED., .F., .F. ) 
 B_SPLINE_CURVE_WITH_KNOTS ( ( 4, 4 ),
 ( 0.007854122480128121128, 0.01576650722534447477 ),
 .UNSPECIFIED. ) 
 CURVE ( )  GEOMETRIC_REPRESENTATION_ITEM ( )  RATIONAL_B_SPLINE_CURVE ( ( 0.5857864376268409057, 0.5560595459730206525, 0.5340584217468142825, 0.5197830649482216847 ) ) 
 REPRESENTATION_ITEM ( '' )  );
#16918 = CARTESIAN_POINT ( 'NONE',  ( -100.7734535825088500, -44.31723036834903695, 12.25131212657476709 ) ) ;
#16919 = CARTESIAN_POINT ( 'NONE',  ( 199.0175917791061977, -16.16856137136818816, -11.77441583767826039 ) ) ;
#16920 = CARTESIAN_POINT ( 'NONE',  ( -110.0723150831436783, -5.015078513972359708, 19.55249150545837367 ) ) ;
#16921 = CARTESIAN_POINT ( 'NONE',  ( 19.06497207195980792, -18.24870850772763475, 38.31983398719622613 ) ) ;
#16922 = FACE_OUTER_BOUND ( 'NONE', #25599, .T. ) ;
#16923 = CARTESIAN_POINT ( 'NONE',  ( 57.59792236341146321, 40.00000000000004263, -2.435789363418021214 ) ) ;
#16924 = CARTESIAN_POINT ( 'NONE',  ( -198.0012279374157345, -24.77357825033869787, 44.79720170867067708 ) ) ;
#16925 = DIRECTION ( 'NONE',  ( -1.000000000000000000, 0.000000000000000000, 0.000000000000000000 ) ) ;
#16926 = CARTESIAN_POINT ( 'NONE',  ( 57.59792236341147742, 4.064940816252731242E-13, -37.56421063658186199 ) ) ;
#16927 = CARTESIAN_POINT ( 'NONE',  ( -192.9588430854690273, 40.00000000000014211, -14.46834944099927966 ) ) ;
#16928 = CARTESIAN_POINT ( 'NONE',  ( -87.01139150504059216, 18.62802765663150595, 10.64887401541982825 ) ) ;
#16929 = CARTESIAN_POINT ( 'NONE',  ( -210.0000000000000284, -52.49999999999992895, -52.49999999999999289 ) ) ;
#16930 = CARTESIAN_POINT ( 'NONE',  ( 199.0058386706367912, 17.79887573832666092, -9.116163937183429766 ) ) ;
#16931 = CARTESIAN_POINT ( 'NONE',  ( -190.5535326094083075, 18.10342187830005400, 43.70552662395296295 ) ) ;
#16932 = CARTESIAN_POINT ( 'NONE',  ( -259.2033419157646676, 6.730120644403426944, 6.730120644403592145 ) ) ;
#16933 = CARTESIAN_POINT ( 'NONE',  ( -210.0000000000000568, 82.50000000000008527, 52.49999999999980105 ) ) ;
#16934 = CARTESIAN_POINT ( 'NONE',  ( -238.4067589809705794, 27.60227080167040370, 28.96627169325338613 ) ) ;
#16935 = CARTESIAN_POINT ( 'NONE',  ( -86.99952317292415671, -18.62540174576058405, 10.54562204240063927 ) ) ;
#16936 = CARTESIAN_POINT ( 'NONE',  ( -91.56559293963834989, -12.25131212657475466, -12.25131212657495361 ) ) ;
#16937 = DIRECTION ( 'NONE',  ( 0.000000000000000000, 0.000000000000000000, -1.000000000000000000 ) ) ;
#16938 = CARTESIAN_POINT ( 'NONE',  ( 19.06497207195980792, -14.19242893257839988, 40.00000000000002132 ) ) ;
#16939 = CARTESIAN_POINT ( 'NONE',  ( -213.1075012329537230, 66.26714140138673770, -9.698598906462034819 ) ) ;
#16940 = CARTESIAN_POINT ( 'NONE',  ( 146.6084372240433709, -5.374981219216948602, 40.00000000000002132 ) ) ;
#16941 = CARTESIAN_POINT ( 'NONE',  ( -600.5150573586311111, 38.73722737577749342, 22.90562922617326080 ) ) ;
#16942 = ORIENTED_EDGE ( 'NONE', *, *, #4541, .F. ) ;
#16943 = CARTESIAN_POINT ( 'NONE',  ( 91.82158438592159655, -39.99999999999976552, -22.79471317813512599 ) ) ;
#16944 = CARTESIAN_POINT ( 'NONE',  ( 199.0061329731654496, 7.677669731782176932, -18.46232380042365051 ) ) ;
#16945 = PLANE ( 'NONE',  #13661 ) ;
#16946 = ORIENTED_EDGE ( 'NONE', *, *, #24784, .F. ) ;
#16947 = EDGE_LOOP ( 'NONE', ( #1623, #10095, #13748, #17411 ) ) ;
#16948 = VERTEX_POINT ( 'NONE', #709 ) ;
#16949 = CARTESIAN_POINT ( 'NONE',  ( -135.8532207217289738, 30.84685318188643421, 40.00000000000002132 ) ) ;
#16950 = CARTESIAN_POINT ( 'NONE',  ( -105.4741150117383199, -19.77569912955117459, -7.943527260750404828 ) ) ;
#16951 = AXIS2_PLACEMENT_3D ( 'NONE', #16791, #14793, #971 ) ;
#16952 = CARTESIAN_POINT ( 'NONE',  ( -114.5514240057833462, -20.88736325016649076, 6.817200166920974524 ) ) ;
#16953 = EDGE_CURVE ( 'NONE', #3360, #12515, #9288, .T. ) ;
#16954 = CARTESIAN_POINT ( 'NONE',  ( -188.2995950289364941, -13.82811170417257607, 46.99046209955427855 ) ) ;
#16955 = CARTESIAN_POINT ( 'NONE',  ( 136.1360204305621266, 1.473277640373554421E-13, -35.03383547441296741 ) ) ;
#16956 = CARTESIAN_POINT ( 'NONE',  ( 199.9999999999996021, 4.009690090792337180, -18.57554820616829261 ) ) ;
#16957 = ADVANCED_FACE ( 'NONE', ( #15557 ), #10467, .T. ) ;
#16958 = CARTESIAN_POINT ( 'NONE',  ( 200.0000000000000000, 1.231416217928662515, -18.97163116072034938 ) ) ;
#16959 = CARTESIAN_POINT ( 'NONE',  ( 19.06497207195981858, 10.03556273973516078, -66.60410523465806421 ) ) ;
#16960 = CARTESIAN_POINT ( 'NONE',  ( 151.7948205124836250, 23.49921654116328540, 23.49921654116366554 ) ) ;
#16961 = CARTESIAN_POINT ( 'NONE',  ( -105.2054292634446284, -16.15935121071317226, -14.23664521671883065 ) ) ;
#16962 = CARTESIAN_POINT ( 'NONE',  ( -30.26275506840323359, 4.336144384597734078E-13, -41.69427246844629309 ) ) ;
#16963 = DIRECTION ( 'NONE',  ( 0.9698969544100559670, -0.2249791742613554413, 0.09318942523042274273 ) ) ;
#16964 = CARTESIAN_POINT ( 'NONE',  ( -2.654373026594472496, 13.89837698318165415, 47.46285323120913802 ) ) ;
#16965 = EDGE_CURVE ( 'NONE', #13683, #11812, #10235, .T. ) ;
#16966 = ADVANCED_FACE ( 'NONE', ( #13564 ), #25315, .F. ) ;
#16967 = CARTESIAN_POINT ( 'NONE',  ( -238.4067589809705794, -0.6820004458488042598, 57.25054294077229855 ) ) ;
#16968 = CARTESIAN_POINT ( 'NONE',  ( 199.0053212086165502, 15.02621665087036362, -13.25052931267129885 ) ) ;
#16970 = CARTESIAN_POINT ( 'NONE',  ( -280.0000000000000000, 1.839446121267387017E-14, -20.00000000000001421 ) ) ;
#16969 = CARTESIAN_POINT ( 'NONE',  ( -30.26275506840324070, 1.198031551616030033, -1.198031551616006496 ) ) ;
#16971 = CARTESIAN_POINT ( 'NONE',  ( -626.9846540392142060, 75.00000000000000000, -60.00000000000000000 ) ) ;
#16972 = CARTESIAN_POINT ( 'NONE',  ( 4.995406935893297096, 10.78321810387837232, 67.35176059880234334 ) ) ;
#16973 = CARTESIAN_POINT ( 'NONE',  ( -238.4067589809705794, 40.96449427990177128, 40.00000000000002132 ) ) ;
#16974 = CIRCLE ( 'NONE', #8901, 34.99999999999999289 ) ;
#16975 = ORIENTED_EDGE ( 'NONE', *, *, #21595, .T. ) ;
#16976 = CARTESIAN_POINT ( 'NONE',  ( 1.925538622597735117, -44.35335385591510260, 24.44644315489020414 ) ) ;
#16977 = CARTESIAN_POINT ( 'NONE',  ( -162.0762913951021176, 1.694272876828294194, -40.00000000000002132 ) ) ;
#16978 = ORIENTED_EDGE ( 'NONE', *, *, #21180, .F. ) ;
#16979 = DIRECTION ( 'NONE',  ( 0.000000000000000000, 0.000000000000000000, 1.000000000000000000 ) ) ;
#16980 = CARTESIAN_POINT ( 'NONE',  ( -4.061681315507545520, -13.82654462146593133, 46.98276670624663609 ) ) ;
#16981 = CARTESIAN_POINT ( 'NONE',  ( -87.07906654914069122, 21.13868447709362641, 3.689035289844212251 ) ) ;
#16982 = CARTESIAN_POINT ( 'NONE',  ( -2.654373026594466278, -13.89837698318132198, -47.46285323120923749 ) ) ;
#16983 = CARTESIAN_POINT ( 'NONE',  ( 199.0207495982873809, -19.04631292825652622, -6.112231798784620196 ) ) ;
#16984 = CARTESIAN_POINT ( 'NONE',  ( 170.2234770963711128, 10.92277846919147066, 45.64576402573197811 ) ) ;
#16985 = CARTESIAN_POINT ( 'NONE',  ( -87.07756624671603163, -21.12895881757819438, 3.737545040698849963 ) ) ;
#16986 =( NAMED_UNIT ( * ) PLANE_ANGLE_UNIT ( ) SI_UNIT ( $, .RADIAN. ) );
#16987 = CARTESIAN_POINT ( 'NONE',  ( -193.3669098795969319, -18.32287322059158896, 44.23532903077781953 ) ) ;
#16988 = CARTESIAN_POINT ( 'NONE',  ( -238.4067589809705794, 27.60227080167080160, -28.96627169325299533 ) ) ;
#16989 = AXIS2_PLACEMENT_3D ( 'NONE', #12511, #16770, #557 ) ;
#16990 = CARTESIAN_POINT ( 'NONE',  ( 130.8568914410475088, 52.36146031193420924, 4.207082182989907437 ) ) ;
#16991 = CARTESIAN_POINT ( 'NONE',  ( -56.48582580120559982, -34.75652343174584047, -21.81201906317815187 ) ) ;
#16992 = CARTESIAN_POINT ( 'NONE',  ( -213.1075012329537230, -9.698598906450422774, -9.698598906450550672 ) ) ;
#16994 = CARTESIAN_POINT ( 'NONE',  ( 200.0000000000000000, 42.42640687119267540, 14.14213562373153543 ) ) ;
#16993 = CARTESIAN_POINT ( 'NONE',  ( -162.0762913951021176, 27.08623940707639477, -29.48230308784743059 ) ) ;
#16995 = CARTESIAN_POINT ( 'NONE',  ( 151.7948205124836250, 4.785054706301759886, -4.785054706301612448 ) ) ;
#16996 = CARTESIAN_POINT ( 'NONE',  ( -259.2033419157646676, 9.517827891722582478, 40.00000000000002132 ) ) ;
#16997 = CARTESIAN_POINT ( 'NONE',  ( -198.0356074513804572, 15.37879056873067007, 0.000000000000000000 ) ) ;
#16998 = CARTESIAN_POINT ( 'NONE',  ( 151.7948205124836534, 4.785054706298574878, -51.78348778862537927 ) ) ;
#16999 = DIRECTION ( 'NONE',  ( 1.836970198721030181E-16, -1.000000000000000000, 0.000000000000000000 ) ) ;
#17000 = CARTESIAN_POINT ( 'NONE',  ( -213.1075012329537230, -37.98287015391257881, 18.58567234101111509 ) ) ;
#17001 = DIRECTION ( 'NONE',  ( 0.000000000000000000, -1.321694076934715579E-16, -1.000000000000000000 ) ) ;
#17002 = ORIENTED_EDGE ( 'NONE', *, *, #14820, .F. ) ;
#17003 = CARTESIAN_POINT ( 'NONE',  ( -100.7734535825088500, -16.03295912088716335, 40.53558337403673306 ) ) ;
#17004 = CARTESIAN_POINT ( 'NONE',  ( -77.70094361819319317, -18.98776814046944494, -11.20662771258744428 ) ) ;
#17005 = CARTESIAN_POINT ( 'NONE',  ( 0.2972598230770100991, -38.42060263243686791, 38.42060263243645579 ) ) ;
#17006 = CARTESIAN_POINT ( 'NONE',  ( -87.13361725327072804, -21.49321519333431141, 0.6860286135013640152 ) ) ;
#17007 = EDGE_LOOP ( 'NONE', ( #18063, #4823, #24521, #16 ) ) ;
#17008 = CARTESIAN_POINT ( 'NONE',  ( -105.3174410934715439, -10.86122935356454100, -18.50851042455845885 ) ) ;
#17009 = VECTOR ( 'NONE', #5877, 1000.000000000000000 ) ;
#17010 = CARTESIAN_POINT ( 'NONE',  ( 199.9999999999998579, 7.403094706059546226, -17.49952075364730675 ) ) ;
#17011 = CARTESIAN_POINT ( 'NONE',  ( -114.4944481313176396, -20.59122811151893373, -7.435744517473755089 ) ) ;
#17012 = CARTESIAN_POINT ( 'NONE',  ( 4.995406935893288214, 55.24977328854835434, 2.449293598294708485E-15 ) ) ;
#17013 = CYLINDRICAL_SURFACE ( 'NONE', #11336, 75.00000000000000000 ) ;
#17014 = CARTESIAN_POINT ( 'NONE',  ( 199.0202951899208017, 7.027923415129357032, 18.72965638665138144 ) ) ;
#17015 =( BOUNDED_SURFACE ( )  B_SPLINE_SURFACE ( 3, 3, ( 
 ( #5922, #13754, #21882, #10177, #14030, #24146, #2203, #16290, #5785, #18281, #7902, #16021, #26160, #13892, #22160, #25888, #3939, #26027, #20154, #1936, #16156, #6057, #20424, #22293, #4205, #22026, #9777, #12172, #20291, #10312 ),
 ( #67, #8175, #7630, #11901, #15765, #17767, #11387, #5669, #20046, #11922, #26185, #23893, #3679, #21641, #9525, #21772, #13775, #1294, #1824, #21904, #11787, #17633, #9402, #23635, #11516, #19907, #7923, #9927, #18033, #15634 ),
 ( #3545, #9663, #7526, #9795, #23511, #19509, #5285, #25909, #11645, #17508, #1691, #17899, #5540, #7650, #26046, #7783, #22047, #25775, #3820, #13392, #19769, #21517, #25648, #15899, #1558, #24028, #3291, #13912, #5414, #5805 ),
 ( #7394, #15507, #13516, #3414, #19641, #23759, #1424, #13647, #16311, #8324, #14577, #24166, #12584, #5941, #20576, #20174, #22183, #16448, #4091, #2348, #14314, #22577, #2479, #12448, #12317, #3956, #24572, #14049, #86, #10461 ),
 ( #4482, #12054, #1957, #10063, #8195, #24311, #6328, #18169, #2222, #20713, #18299, #489, #20312, #26316, #14450, #2089, #8059, #24707, #18573, #6077, #16175, #4356, #6462, #353, #24435, #8457, #16576, #14179, #10196, #22314 ),
 ( #6203, #22448, #12190, #16040, #4228, #20444, #10330, #18439, #214, #22706, #10591, #18706, #21368, #887, #7120, #14838, #24838, #15100, #23108, #13243, #620, #19232, #25366, #8996, #23361, #6726, #17100, #2886, #22843, #25233 ),
 ( #16844, #6856, #5138, #6589, #14711, #12714, #755, #24977, #6985, #20842, #21107, #3136, #10857, #19356, #12855, #16706, #23235, #20973, #2617, #17226, #3011, #22971, #10731, #5011, #15230, #1012, #8859, #13116, #21237, #4618 ) ),
 .UNSPECIFIED., .T., .F., .F. ) 
 B_SPLINE_SURFACE_WITH_KNOTS ( ( 4, 3, 4 ),
 ( 4, 2, 2, 2, 2, 2, 2, 2, 2, 2, 2, 2, 2, 2, 4 ),
 ( 0.000000000000000000, 0.5000000000000000000, 1.000000000000000000 ),
 ( 0.000000000000000000, 0.1357259735107005372, 0.1651108541090157700, 0.1944957347073310028, 0.3598804999793158710, 0.3867117631979620773, 0.4135430264166082281, 0.5789277916885930964, 0.6062785021374117456, 0.6336292125862302838, 0.8508620842112317728, 0.8814014469398914198, 0.9119408096685510667, 0.9559704048342755334, 1.000000000000000000 ),
 .UNSPECIFIED. ) 
 GEOMETRIC_REPRESENTATION_ITEM ( )  RATIONAL_B_SPLINE_SURFACE ( (
 ( 1.000000000000000000, 1.000000000000000000, 1.000000000000000000, 1.000000000000000000, 1.000000000000000000, 1.000000000000000000, 1.000000000000000000, 1.000000000000000000, 1.000000000000000000, 1.000000000000000000, 1.000000000000000000, 1.000000000000000000, 1.000000000000000000, 1.000000000000000000, 1.000000000000000000, 1.000000000000000000, 1.000000000000000000, 1.000000000000000000, 1.000000000000000000, 1.000000000000000000, 1.000000000000000000, 1.000000000000000000, 1.000000000000000000, 1.000000000000000000, 1.000000000000000000, 1.000000000000000000, 1.000000000000000000, 1.000000000000000000, 1.000000000000000000, 1.000000000000000000),
 ( 0.3333333333333333703, 0.3333333333333333703, 0.3333333333333333703, 0.3333333333333333703, 0.3333333333333333703, 0.3333333333333333703, 0.3333333333333333703, 0.3333333333333333703, 0.3333333333333333703, 0.3333333333333333703, 0.3333333333333333703, 0.3333333333333333703, 0.3333333333333333703, 0.3333333333333333703, 0.3333333333333333703, 0.3333333333333333703, 0.3333333333333333703, 0.3333333333333333703, 0.3333333333333333703, 0.3333333333333333703, 0.3333333333333333703, 0.3333333333333333703, 0.3333333333333333703, 0.3333333333333333703, 0.3333333333333333703, 0.3333333333333333703, 0.3333333333333333703, 0.3333333333333333703, 0.3333333333333333703, 0.3333333333333333703),
 ( 0.3333333333333333703, 0.3333333333333333703, 0.3333333333333333703, 0.3333333333333333703, 0.3333333333333333703, 0.3333333333333333703, 0.3333333333333333703, 0.3333333333333333703, 0.3333333333333333703, 0.3333333333333333703, 0.3333333333333333703, 0.3333333333333333703, 0.3333333333333333703, 0.3333333333333333703, 0.3333333333333333703, 0.3333333333333333703, 0.3333333333333333703, 0.3333333333333333703, 0.3333333333333333703, 0.3333333333333333703, 0.3333333333333333703, 0.3333333333333333703, 0.3333333333333333703, 0.3333333333333333703, 0.3333333333333333703, 0.3333333333333333703, 0.3333333333333333703, 0.3333333333333333703, 0.3333333333333333703, 0.3333333333333333703),
 ( 1.000000000000000000, 1.000000000000000000, 1.000000000000000000, 1.000000000000000000, 1.000000000000000000, 1.000000000000000000, 1.000000000000000000, 1.000000000000000000, 1.000000000000000000, 1.000000000000000000, 1.000000000000000000, 1.000000000000000000, 1.000000000000000000, 1.000000000000000000, 1.000000000000000000, 1.000000000000000000, 1.000000000000000000, 1.000000000000000000, 1.000000000000000000, 1.000000000000000000, 1.000000000000000000, 1.000000000000000000, 1.000000000000000000, 1.000000000000000000, 1.000000000000000000, 1.000000000000000000, 1.000000000000000000, 1.000000000000000000, 1.000000000000000000, 1.000000000000000000),
 ( 0.3333333333333333703, 0.3333333333333333703, 0.3333333333333333703, 0.3333333333333333703, 0.3333333333333333703, 0.3333333333333333703, 0.3333333333333333703, 0.3333333333333333703, 0.3333333333333333703, 0.3333333333333333703, 0.3333333333333333703, 0.3333333333333333703, 0.3333333333333333703, 0.3333333333333333703, 0.3333333333333333703, 0.3333333333333333703, 0.3333333333333333703, 0.3333333333333333703, 0.3333333333333333703, 0.3333333333333333703, 0.3333333333333333703, 0.3333333333333333703, 0.3333333333333333703, 0.3333333333333333703, 0.3333333333333333703, 0.3333333333333333703, 0.3333333333333333703, 0.3333333333333333703, 0.3333333333333333703, 0.3333333333333333703),
 ( 0.3333333333333333703, 0.3333333333333333703, 0.3333333333333333703, 0.3333333333333333703, 0.3333333333333333703, 0.3333333333333333703, 0.3333333333333333703, 0.3333333333333333703, 0.3333333333333333703, 0.3333333333333333703, 0.3333333333333333703, 0.3333333333333333703, 0.3333333333333333703, 0.3333333333333333703, 0.3333333333333333703, 0.3333333333333333703, 0.3333333333333333703, 0.3333333333333333703, 0.3333333333333333703, 0.3333333333333333703, 0.3333333333333333703, 0.3333333333333333703, 0.3333333333333333703, 0.3333333333333333703, 0.3333333333333333703, 0.3333333333333333703, 0.3333333333333333703, 0.3333333333333333703, 0.3333333333333333703, 0.3333333333333333703),
 ( 1.000000000000000000, 1.000000000000000000, 1.000000000000000000, 1.000000000000000000, 1.000000000000000000, 1.000000000000000000, 1.000000000000000000, 1.000000000000000000, 1.000000000000000000, 1.000000000000000000, 1.000000000000000000, 1.000000000000000000, 1.000000000000000000, 1.000000000000000000, 1.000000000000000000, 1.000000000000000000, 1.000000000000000000, 1.000000000000000000, 1.000000000000000000, 1.000000000000000000, 1.000000000000000000, 1.000000000000000000, 1.000000000000000000, 1.000000000000000000, 1.000000000000000000, 1.000000000000000000, 1.000000000000000000, 1.000000000000000000, 1.000000000000000000, 1.000000000000000000) ) ) 
 REPRESENTATION_ITEM ( '' )  SURFACE ( )  );
#17016 = CARTESIAN_POINT ( 'NONE',  ( 200.0000000000000000, -14.14213562373122457, 42.42640687119282461 ) ) ;
#17017 = CARTESIAN_POINT ( 'NONE',  ( 163.1118516004056573, -1.695744499706194789E-14, 12.73709011382475254 ) ) ;
#17018 = CARTESIAN_POINT ( 'NONE',  ( 192.4448373802101173, 39.99999999999998579, 19.99999999996075317 ) ) ;
#17019 = CARTESIAN_POINT ( 'NONE',  ( -87.13361725327074225, 15.19799821270847850, -15.19799821270833284 ) ) ;
#17020 = CARTESIAN_POINT ( 'NONE',  ( -198.0356074513804572, -55.37879056871328487, -40.00000000000002132 ) ) ;
#17022 = CARTESIAN_POINT ( 'NONE',  ( -607.2519390358020246, 32.98910822842147894, 22.67520286530086793 ) ) ;
#17021 = CARTESIAN_POINT ( 'NONE',  ( 22.78333232259009122, -17.88247728649339052, -43.17211919388243047 ) ) ;
#17023 = CARTESIAN_POINT ( 'NONE',  ( 151.7948205124836534, -6.767089262349000656, -40.00000000000002132 ) ) ;
#17024 = CARTESIAN_POINT ( 'NONE',  ( 4.995406935893293543, -10.78321810389005364, 10.78321810388994173 ) ) ;
#17025 = CARTESIAN_POINT ( 'NONE',  ( -100.7734535825088500, 40.00000000000017764, -17.32597176626768487 ) ) ;
#17026 = CARTESIAN_POINT ( 'NONE',  ( -210.0000000000000284, 69.99999999999998579, 0.000000000000000000 ) ) ;
#17027 = CARTESIAN_POINT ( 'NONE',  ( 146.6084372240433709, -39.99999999999993605, -5.374981219217395356 ) ) ;
#17028 = DIRECTION ( 'NONE',  ( -1.000000000000000000, 0.000000000000000000, 0.000000000000000000 ) ) ;
#17029 = EDGE_CURVE ( 'NONE', #14634, #525, #1329, .T. ) ;
#17030 = CARTESIAN_POINT ( 'NONE',  ( 159.7742640750898317, -25.95918014511565985, -10.75264448419334684 ) ) ;
#17031 = CARTESIAN_POINT ( 'NONE',  ( -100.7734535825088500, 40.53558337403654832, 16.03295912088756481 ) ) ;
#17032 = CARTESIAN_POINT ( 'NONE',  ( 91.82158438592159655, -16.11829626346147393, 16.11829626346132116 ) ) ;
#17033 = VERTEX_POINT ( 'NONE', #19186 ) ;
#17035 = CARTESIAN_POINT ( 'NONE',  ( -5.787027468457909052, 42.67020100828210616, -17.67457596682473664 ) ) ;
#17034 = CARTESIAN_POINT ( 'NONE',  ( -77.90255099906769942, -8.064892378657791738, -20.29001641120690635 ) ) ;
#17036 = DIRECTION ( 'NONE',  ( 0.9698969544411999433, -0.2249791741464770845, -0.09318942518362427485 ) ) ;
#17037 = CARTESIAN_POINT ( 'NONE',  ( 146.6084372240433993, -5.374981219216945938, -2.449293598294708485E-15 ) ) ;
#17038 = CARTESIAN_POINT ( 'NONE',  ( -87.13361725327072804, -21.49321519333431141, -3.542586001259484843E-15 ) ) ;
#17039 = CARTESIAN_POINT ( 'NONE',  ( -189.6939181379374588, 43.50327460064623608, -18.01964634722715530 ) ) ;
#17040 =( LENGTH_UNIT ( ) NAMED_UNIT ( * ) SI_UNIT ( .MILLI., .METRE. ) );
#17041 = EDGE_LOOP ( 'NONE', ( #1901, #18273 ) ) ;
#17042 = ORIENTED_EDGE ( 'NONE', *, *, #21012, .T. ) ;
#17043 = CARTESIAN_POINT ( 'NONE',  ( 199.9999999999999432, -6.708851862405343702, 17.79758909344539219 ) ) ;
#17044 = CARTESIAN_POINT ( 'NONE',  ( -102.4309680866260521, 8.087567261726858803, -20.43798635336598934 ) ) ;
#17045 = VERTEX_POINT ( 'NONE', #9073 ) ;
#17046 = ORIENTED_EDGE ( 'NONE', *, *, #15610, .T. ) ;
#17047 = CARTESIAN_POINT ( 'NONE',  ( -280.0000000000000568, -14.14213562373108601, 42.42640687119285303 ) ) ;
#17048 = CARTESIAN_POINT ( 'NONE',  ( 199.0200497209392267, -18.54142962866078648, -7.504851164020625021 ) ) ;
#17049 = AXIS2_PLACEMENT_3D ( 'NONE', #3674, #25903, #9522 ) ;
#17050 = CARTESIAN_POINT ( 'NONE',  ( -105.2958943010082749, -4.721182065458395805, 20.90688085069918500 ) ) ;
#17051 = CARTESIAN_POINT ( 'NONE',  ( -259.2033419157646676, -6.730120644403667640, 49.83842185052029805 ) ) ;
#17052 = CONICAL_SURFACE ( 'NONE', #25546, 39.99999999999997158, 0.4944367829892074018 ) ;
#17053 = CARTESIAN_POINT ( 'NONE',  ( 98.29820294270297154, 18.47759065022021474, -7.653668647299666894 ) ) ;
#17054 = CARTESIAN_POINT ( 'NONE',  ( 14.38125909742180930, 39.99999999999982947, 55.17850393971022527 ) ) ;
#17055 = CIRCLE ( 'NONE', #20452, 10.00000000000004796 ) ;
#17056 = LINE ( 'NONE', #18925, #1962 ) ;
#17057 = ADVANCED_FACE ( 'NONE', ( #15188 ), #23314, .T. ) ;
#17058 = CARTESIAN_POINT ( 'NONE',  ( -626.9846540392097722, 75.00000000000000000, 65.00000000000002842 ) ) ;
#17059 = CARTESIAN_POINT ( 'NONE',  ( 184.8905102610680444, -40.00000000000021316, 20.92133201514402430 ) ) ;
#17060 = CARTESIAN_POINT ( 'NONE',  ( -105.3755690713226585, -39.99999999999985079, -18.24025645688394448 ) ) ;
#17061 = FACE_OUTER_BOUND ( 'NONE', #1768, .T. ) ;
#17062 = DIRECTION ( 'NONE',  ( 0.000000000000000000, 0.000000000000000000, -1.000000000000000000 ) ) ;
#17063 = CARTESIAN_POINT ( 'NONE',  ( 199.0053213077726753, 13.66600449016087993, -14.61040478752057226 ) ) ;
#17064 = CARTESIAN_POINT ( 'NONE',  ( -194.4222775680326265, 14.07715774765984840, 48.65439176088747786 ) ) ;
#17065 = CARTESIAN_POINT ( 'NONE',  ( 151.7948205124835681, -4.785054706298876859, 51.78348778862533663 ) ) ;
#17066 = DIRECTION ( 'NONE',  ( 0.000000000000000000, 1.000000000000000000, 0.000000000000000000 ) ) ;
#17067 = CARTESIAN_POINT ( 'NONE',  ( -162.0762913951021176, 27.08623940707598265, 29.48230308784781428 ) ) ;
#17068 = CARTESIAN_POINT ( 'NONE',  ( -77.61421004776265420, -12.97751843348499889, 17.87698779689324979 ) ) ;
#17069 = CARTESIAN_POINT ( 'NONE',  ( 136.1360204305621266, 53.05693388239320285, -3.511608612530223716 ) ) ;
#17070 = CARTESIAN_POINT ( 'NONE',  ( -652.3021900505264057, 37.95920247636578182, 24.17282378433309020 ) ) ;
#17071 = CARTESIAN_POINT ( 'NONE',  ( -200.0000000000000000, 52.50000000000007816, 52.49999999999999289 ) ) ;
#17072 = VERTEX_POINT ( 'NONE', #17311 ) ;
#17073 = CARTESIAN_POINT ( 'NONE',  ( -259.2033419157646676, 49.83842185052017015, 6.730120644404137487 ) ) ;
#17074 = CARTESIAN_POINT ( 'NONE',  ( -86.96347745069645896, 21.75974354311648895, -0.000000000000000000 ) ) ;
#17075 = CARTESIAN_POINT ( 'NONE',  ( -593.2841520101219430, 43.99625175998158966, -9.521709705159564052 ) ) ;
#17076 = ORIENTED_EDGE ( 'NONE', *, *, #545, .F. ) ;
#17077 = CARTESIAN_POINT ( 'NONE',  ( -135.8532207217289738, -39.99999999999972289, -30.84685318188688541 ) ) ;
#17078 = CARTESIAN_POINT ( 'NONE',  ( 199.0102713619699841, -4.331938195896105626, -19.53328621734312875 ) ) ;
#17079 = CARTESIAN_POINT ( 'NONE',  ( 126.3230993689413140, -11.72464299830521384, 28.30579214049032899 ) ) ;
#17080 = EDGE_LOOP ( 'NONE', ( #2655, #13051, #16911, #23111 ) ) ;
#17081 = EDGE_LOOP ( 'NONE', ( #21589, #25939 ) ) ;
#17082 = ORIENTED_EDGE ( 'NONE', *, *, #1201, .F. ) ;
#17083 = CARTESIAN_POINT ( 'NONE',  ( 146.6084372240433709, 5.374981219216996564, 40.00000000000002132 ) ) ;
#17084 = CYLINDRICAL_SURFACE ( 'NONE', #24883, 74.99999999999995737 ) ;
#17085 = CIRCLE ( 'NONE', #18799, 69.99999999999994316 ) ;
#17086 = DIRECTION ( 'NONE',  ( -1.000000000000000000, -1.836970198721030181E-16, -0.000000000000000000 ) ) ;
#17087 = CARTESIAN_POINT ( 'NONE',  ( 163.1118516004056573, 1.251511021549353291E-13, -27.26290988616872824 ) ) ;
#17088 = CARTESIAN_POINT ( 'NONE',  ( 200.0000000000001705, 6.971423609723053971, -17.67803530771774589 ) ) ;
#17089 = CARTESIAN_POINT ( 'NONE',  ( 199.9999999999999432, 8.677819433020733442, -16.90353765624616500 ) ) ;
#17090 = CARTESIAN_POINT ( 'NONE',  ( -30.26275506840324070, 1.198031551616724366, -57.76657404653984429 ) ) ;
#17091 = CARTESIAN_POINT ( 'NONE',  ( 199.9999999999999432, 14.14213562373093680, 14.14213562373114641 ) ) ;
#17092 = CARTESIAN_POINT ( 'NONE',  ( -105.2054292635175585, -15.19799821370228798, -15.19799821370232173 ) ) ;
#17093 = CARTESIAN_POINT ( 'NONE',  ( -86.96347745069644475, 1.775309070576523494E-13, -18.24025645688352881 ) ) ;
#17094 = CARTESIAN_POINT ( 'NONE',  ( -198.0356074513804572, -10.87444709759714634, -10.87444709759729911 ) ) ;
#17095 = FACE_OUTER_BOUND ( 'NONE', #3015, .T. ) ;
#17096 = CARTESIAN_POINT ( 'NONE',  ( 146.6084372240433993, -3.800685668858652999, 3.800685668858636568 ) ) ;
#17097 = CARTESIAN_POINT ( 'NONE',  ( 199.0102747309263975, 19.53166102356907885, 4.339329946343584155 ) ) ;
#17099 = CARTESIAN_POINT ( 'NONE',  ( 14.38125909742181108, -5.035366881890652543E-14, 15.17850393972633682 ) ) ;
#17098 = CARTESIAN_POINT ( 'NONE',  ( 136.1360204305621551, -24.77266263493081766, -31.79587985999290112 ) ) ;
#17100 = CARTESIAN_POINT ( 'NONE',  ( 170.2234770963711128, -24.55285855007184281, -40.00000000000002132 ) ) ;
#17101 = CARTESIAN_POINT ( 'NONE',  ( -30.26275506840324070, 1.198031551615912571, 57.76657404653985139 ) ) ;
#17102 = CARTESIAN_POINT ( 'NONE',  ( 57.59792236341147031, 37.56421063658187620, 40.00000000000002132 ) ) ;
#17103 = ORIENTED_EDGE ( 'NONE', *, *, #25821, .T. ) ;
#17104 = EDGE_CURVE ( 'NONE', #19850, #5806, #6209, .T. ) ;
#17105 = CARTESIAN_POINT ( 'NONE',  ( 8.273828130744583120, -44.87796109790054544, 18.58906013840162785 ) ) ;
#17106 = CARTESIAN_POINT ( 'NONE',  ( 14.38125909742180752, 15.17850393972634038, -40.00000000000002132 ) ) ;
#17107 = LINE ( 'NONE', #19238, #3886 ) ;
#17108 = ADVANCED_FACE ( 'NONE', ( #17431 ), #25571, .T. ) ;
#17109 = CARTESIAN_POINT ( 'NONE',  ( -91.56559293963834989, -16.03295912088716335, 40.53558337403673306 ) ) ;
#17110 = CARTESIAN_POINT ( 'NONE',  ( 136.1360204305621551, -39.99999999999987921, -35.03383547441310242 ) ) ;
#17111 = CARTESIAN_POINT ( 'NONE',  ( -87.09798021405659085, 21.26125105737227372, 2.995673697387337686 ) ) ;
#17112 = EDGE_CURVE ( 'NONE', #19812, #21839, #5472, .T. ) ;
#17113 = EDGE_CURVE ( 'NONE', #16811, #12394, #8978, .T. ) ;
#17114 = CARTESIAN_POINT ( 'NONE',  ( -77.90255099906865155, 8.064892378658621297, -20.29001641120614252 ) ) ;
#17115 = CARTESIAN_POINT ( 'NONE',  ( 199.0263771353516233, -14.14574067859894413, 14.14574067859863682 ) ) ;
#17116 = CARTESIAN_POINT ( 'NONE',  ( -208.1127848780264742, 67.17687982763172272, -10.60833733270698254 ) ) ;
#17117 = DIRECTION ( 'NONE',  ( 0.000000000000000000, 0.000000000000000000, -1.000000000000000000 ) ) ;
#17118 = B_SPLINE_CURVE_WITH_KNOTS ( 'NONE', 3,
 ( #13867, #24259, #12013, #24124, #14405, #22133 ),
 .UNSPECIFIED., .F., .F.,
 ( 4, 2, 4 ),
 ( 0.000000000000000000, 0.03937794852163883919, 0.07875589704327767837 ),
 .UNSPECIFIED. ) ;
#17119 =( LENGTH_UNIT ( ) NAMED_UNIT ( * ) SI_UNIT ( .MILLI., .METRE. ) );
#17120 = CARTESIAN_POINT ( 'NONE',  ( -105.3755690713226585, 43.67073346367988051, -12.89780903124366418 ) ) ;
#17121 = CARTESIAN_POINT ( 'NONE',  ( 136.1360204305621266, 53.05693388239316022, 3.511608612530967566 ) ) ;
#17122 = CARTESIAN_POINT ( 'NONE',  ( -77.90255099906853786, 8.644468104252327478, -20.04994828524281303 ) ) ;
#17123 = CARTESIAN_POINT ( 'NONE',  ( 4.995406935893293543, -10.78321810388990265, -10.78321810389009272 ) ) ;
#17125 = CARTESIAN_POINT ( 'NONE',  ( 192.4448373802101173, 14.14213562370261279, 42.42640687122091236 ) ) ;
#17124 = CARTESIAN_POINT ( 'NONE',  ( -198.9233928134160578, 24.80620717269982833, -44.84148042516462596 ) ) ;
#17126 = CARTESIAN_POINT ( 'NONE',  ( -86.96347745069644475, 12.89780903124419353, -12.89780903124389333 ) ) ;
#17127 = CARTESIAN_POINT ( 'NONE',  ( -86.96347745069644475, 18.24025645688350750, -40.00000000000002132 ) ) ;
#17128 = CARTESIAN_POINT ( 'NONE',  ( 163.1118516004056573, 37.29075403953160617, -19.27778845539222985 ) ) ;
#17129 = FACE_OUTER_BOUND ( 'NONE', #14810, .T. ) ;
#17130 = CARTESIAN_POINT ( 'NONE',  ( -238.4067589809705794, -57.25054294077233408, -0.6820004458489551391 ) ) ;
#17131 = CARTESIAN_POINT ( 'NONE',  ( -151.4802849342813715, 31.86309571753157854, -16.17241510390819670 ) ) ;
#17132 = ORIENTED_EDGE ( 'NONE', *, *, #9776, .T. ) ;
#17133 = CARTESIAN_POINT ( 'NONE',  ( -105.3755690713226727, 12.89780903124400879, 12.89780903124407452 ) ) ;
#17134 = CARTESIAN_POINT ( 'NONE',  ( -77.55640685876512919, -15.64922766773197971, -15.64922766773223906 ) ) ;
#17135 = CARTESIAN_POINT ( 'NONE',  ( -105.3755690713226585, 43.67073346367970288, 12.89780903124427702 ) ) ;
#17136 = CARTESIAN_POINT ( 'NONE',  ( -4.421177063219155379, -42.89273859401222211, -23.37490463203747382 ) ) ;
#17137 = VERTEX_POINT ( 'NONE', #13662 ) ;
#17138 = CARTESIAN_POINT ( 'NONE',  ( -188.2506440019887464, -42.99080317017353536, 23.43978047293204980 ) ) ;
#17139 = CARTESIAN_POINT ( 'NONE',  ( 200.0000000000000284, -14.89093438834758842, -11.81132417993805639 ) ) ;
#17140 = CARTESIAN_POINT ( 'NONE',  ( 22.76838195347369620, -17.88421977190821011, 43.17632592580125817 ) ) ;
#17141 = EDGE_CURVE ( 'NONE', #7950, #8666, #265, .T. ) ;
#17142 = CARTESIAN_POINT ( 'NONE',  ( 146.6084372240433709, -34.62501878078303008, -40.00000000000002132 ) ) ;
#17143 = CARTESIAN_POINT ( 'NONE',  ( 190.0000000000000000, 75.00000000000004263, 9.184850993605150311E-15 ) ) ;
#17144 = CARTESIAN_POINT ( 'NONE',  ( 199.0123267138131098, 18.14094429105657369, 8.417911433729377890 ) ) ;
#17145 = CARTESIAN_POINT ( 'NONE',  ( -91.56559293963834989, -40.53558337403692491, 16.03295912088671571 ) ) ;
#17146 = CARTESIAN_POINT ( 'NONE',  ( 146.6084372240433709, -40.00000000000001421, 5.374981219216829587 ) ) ;
#17147 = CARTESIAN_POINT ( 'NONE',  ( -192.9588430854689989, -8.596193650988133061E-14, 14.46834944099969533 ) ) ;
#17148 = DIRECTION ( 'NONE',  ( 0.000000000000000000, 0.000000000000000000, 1.000000000000000000 ) ) ;
#17149 = CARTESIAN_POINT ( 'NONE',  ( 163.1118516004056573, 27.26290988616876021, -40.00000000000002132 ) ) ;
#17151 = CARTESIAN_POINT ( 'NONE',  ( -192.9588430854689989, -10.23066800230756890, 10.23066800230742501 ) ) ;
#17150 = CARTESIAN_POINT ( 'NONE',  ( 22.80622392652972508, -17.87980911537404438, -43.16567765897917752 ) ) ;
#17152 = CARTESIAN_POINT ( 'NONE',  ( 146.6084372240433709, -5.374981219216948602, 40.00000000000002132 ) ) ;
#17153 = CARTESIAN_POINT ( 'NONE',  ( 57.59792236341147031, 30.00663442387683588, 26.56190807104703211 ) ) ;
#17154 = CARTESIAN_POINT ( 'NONE',  ( -198.0356074513804572, 40.00000000000056843, -55.37879056871282302 ) ) ;
#17155 = CARTESIAN_POINT ( 'NONE',  ( -105.3178975792744865, 18.51275824395281333, -10.85284064411650817 ) ) ;
#17156 = CARTESIAN_POINT ( 'NONE',  ( 163.1118516004056573, -39.99999999999986500, -12.73709011382517353 ) ) ;
#17157 = CARTESIAN_POINT ( 'NONE',  ( 199.0249982833957176, -5.192600369583379560, 19.31944532238548362 ) ) ;
#17158 = CARTESIAN_POINT ( 'NONE',  ( 135.5348526930097250, -30.20724113681565726, -12.51224896074355009 ) ) ;
#17159 = CARTESIAN_POINT ( 'NONE',  ( -259.2033419157646676, 49.83842185052017015, 6.730120644404137487 ) ) ;
#17160 = CARTESIAN_POINT ( 'NONE',  ( 130.8568914410475088, 52.36146031193420924, 4.207082182989907437 ) ) ;
#17161 = ORIENTED_EDGE ( 'NONE', *, *, #15781, .F. ) ;
#17163 = CARTESIAN_POINT ( 'NONE',  ( -3.524834090817577259, 43.28235980537106542, -17.92814044289665887 ) ) ;
#17162 = CARTESIAN_POINT ( 'NONE',  ( -105.3755690713226727, 15.38646221621771737, 15.38646221621800514 ) ) ;
#17164 = CARTESIAN_POINT ( 'NONE',  ( 167.0466155511619775, 23.44215416552595954, -9.710058186601713714 ) ) ;
#17165 = CARTESIAN_POINT ( 'NONE',  ( 19.06497207195980792, -14.19242893257839988, 40.00000000000002132 ) ) ;
#17166 = CARTESIAN_POINT ( 'NONE',  ( -266.9101291198153376, 5.510910596163085611E-15, 44.99999999999997158 ) ) ;
#17167 = CARTESIAN_POINT ( 'NONE',  ( -189.2667466962275569, 43.39859272266281920, -17.97628569363235229 ) ) ;
#17168 = DIRECTION ( 'NONE',  ( 1.000000000000000000, 0.000000000000000000, 0.000000000000000000 ) ) ;
#17169 = ORIENTED_EDGE ( 'NONE', *, *, #225, .F. ) ;
#17170 = VERTEX_POINT ( 'NONE', #25661 ) ;
#17171 = CARTESIAN_POINT ( 'NONE',  ( -208.1127848780265026, -10.60833733269551971, 10.60833733269537049 ) ) ;
#17172 = CARTESIAN_POINT ( 'NONE',  ( 48.46158931187878238, -35.02055581498660075, -18.19743074333930721 ) ) ;
#17173 = ORIENTED_EDGE ( 'NONE', *, *, #15877, .F. ) ;
#17174 = ORIENTED_EDGE ( 'NONE', *, *, #15552, .F. ) ;
#17175 = CARTESIAN_POINT ( 'NONE',  ( 199.0205961407162931, -18.94296041394271768, -6.425165802706580997 ) ) ;
#17176 = CARTESIAN_POINT ( 'NONE',  ( -110.0685463886633926, -5.325649136221389135, 19.46857821975921965 ) ) ;
#17177 = CARTESIAN_POINT ( 'NONE',  ( 0.2972598230770011618, 10.13633138497462305, 66.70487387989858519 ) ) ;
#17178 = CARTESIAN_POINT ( 'NONE',  ( 57.59792236341147031, -1.722363176415032004, -1.722363176415048880 ) ) ;
#17179 = CARTESIAN_POINT ( 'NONE',  ( 19.06497207195979726, 39.99999999999997158, 14.19242893257854554 ) ) ;
#17180 = CARTESIAN_POINT ( 'NONE',  ( -200.0000000000000000, -47.66874763508945279, 16.05666331275199354 ) ) ;
#17181 = CARTESIAN_POINT ( 'NONE',  ( -4.039451493210481026, -46.99046209229796034, -13.82811171175467102 ) ) ;
#17182 = CARTESIAN_POINT ( 'NONE',  ( -198.0356074513804572, -39.99999999999990052, -15.37879056873112482 ) ) ;
#17183 = CARTESIAN_POINT ( 'NONE',  ( -192.9588430854690273, 40.00000000000055422, -54.46834944101679810 ) ) ;
#17184 = CARTESIAN_POINT ( 'NONE',  ( -77.55640685876515761, 15.64922766773203833, 15.64922766773210761 ) ) ;
#17185 = CARTESIAN_POINT ( 'NONE',  ( -83.21262154144251610, -33.12752917118416462, -13.72187187061500779 ) ) ;
#17186 = CARTESIAN_POINT ( 'NONE',  ( -200.0000000000000568, 22.35311919176605500, -45.06067021511782400 ) ) ;
#17187 = CARTESIAN_POINT ( 'NONE',  ( -138.9613198122422375, 27.95779845120243934, -13.65853124629182247 ) ) ;
#17188 = DIRECTION ( 'NONE',  ( 0.000000000000000000, -1.321694076934715579E-16, -1.000000000000000000 ) ) ;
#17189 = CARTESIAN_POINT ( 'NONE',  ( -193.0908541284702551, -48.38978395451684378, 14.03723495791117948 ) ) ;
#17190 = DIRECTION ( 'NONE',  ( -1.836970198721030181E-16, 1.000000000000000000, 0.000000000000000000 ) ) ;
#17191 = CARTESIAN_POINT ( 'NONE',  ( -77.56349232223320200, -14.64315958560953490, 16.60062240782924547 ) ) ;
#17192 = CARTESIAN_POINT ( 'NONE',  ( -86.96347745069643054, -41.18208027870611687, 15.38646221621750954 ) ) ;
#17193 = CARTESIAN_POINT ( 'NONE',  ( -660.7618416459580430, 44.05453155840947943, -9.478650601227100125 ) ) ;
#17194 = CARTESIAN_POINT ( 'NONE',  ( 170.0000000000428315, 17.64300463311351308, -17.64300463311329992 ) ) ;
#17195 = EDGE_CURVE ( 'NONE', #7311, #858, #395, .T. ) ;
#17196 = EDGE_LOOP ( 'NONE', ( #2830, #7346, #25815, #91 ) ) ;
#17197 = CARTESIAN_POINT ( 'NONE',  ( 19.06497207195979726, 38.31983398719604139, 18.24870850772803976 ) ) ;
#17198 = DIRECTION ( 'NONE',  ( 0.000000000000000000, 0.000000000000000000, 1.000000000000000000 ) ) ;
#17199 = FACE_OUTER_BOUND ( 'NONE', #20217, .T. ) ;
#17200 = ORIENTED_EDGE ( 'NONE', *, *, #8930, .T. ) ;
#17201 = CARTESIAN_POINT ( 'NONE',  ( -259.2033419157646676, -39.99999999999975131, -30.48217210827782608 ) ) ;
#17202 = CARTESIAN_POINT ( 'NONE',  ( 199.0228991319552563, -19.97028783757971127, -1.189345221019080245 ) ) ;
#17203 = ADVANCED_FACE ( 'NONE', ( #19404 ), #18963, .F. ) ;
#17204 = CARTESIAN_POINT ( 'NONE',  ( -199.9999999999999432, 10.02640517461776426, -53.44529986889236284 ) ) ;
#17205 = VERTEX_POINT ( 'NONE', #25789 ) ;
#17206 = ORIENTED_EDGE ( 'NONE', *, *, #2985, .T. ) ;
#17207 = CARTESIAN_POINT ( 'NONE',  ( -30.26275506840324070, 41.69427246844628598, 2.449293598294708485E-15 ) ) ;
#17208 = ADVANCED_FACE ( 'NONE', ( #3428 ), #17648, .F. ) ;
#17209 = ADVANCED_FACE ( 'NONE', ( #5682 ), #15529, .T. ) ;
#17210 = CARTESIAN_POINT ( 'NONE',  ( -77.56334768864783769, -14.65129183225244169, 16.59360462362402089 ) ) ;
#17211 = CARTESIAN_POINT ( 'NONE',  ( 19.06497207195981858, -40.00000000000007105, 14.19242893257826665 ) ) ;
#17212 = CARTESIAN_POINT ( 'NONE',  ( 199.9999999999999147, -15.17855064416508526, -11.43956010876637563 ) ) ;
#17213 = AXIS2_PLACEMENT_3D ( 'NONE', #4900, #2774, #5032 ) ;
#17214 = CARTESIAN_POINT ( 'NONE',  ( -86.86493150571118349, 8.366608963953861888, 19.60045294882763400 ) ) ;
#17215 = CARTESIAN_POINT ( 'NONE',  ( -47.50817905883608461, -12.56548180746172427, -30.33575659736102281 ) ) ;
#17216 = CARTESIAN_POINT ( 'NONE',  ( 192.4448373802100889, 14.14213562375873678, 14.14213562375894817 ) ) ;
#17217 = CARTESIAN_POINT ( 'NONE',  ( -200.0000000000000000, -61.50000000000002132, -66.50000000000005684 ) ) ;
#17218 = CARTESIAN_POINT ( 'NONE',  ( 146.6084372240433709, -39.99999999999993605, -5.374981219217395356 ) ) ;
#17219 = CARTESIAN_POINT ( 'NONE',  ( -105.4741150117366431, -7.943527260727707429, 19.77569912956141707 ) ) ;
#17220 = B_SPLINE_CURVE_WITH_KNOTS ( 'NONE', 3,
 ( #13056, #10933, #6924, #25043, #688, #23046, #2417, #10666, #10393, #15041, #14513, #4821, #22645, #285 ),
 .UNSPECIFIED., .F., .F.,
 ( 4, 2, 2, 2, 2, 2, 4 ),
 ( 0.0003146819161548550822, 0.002410867973033469468, 0.004507054029912084016, 0.008699426143669313979, 0.01079561220054792853, 0.01289179825742654481, 0.01708417037118376697 ),
 .UNSPECIFIED. ) ;
#17221 = CARTESIAN_POINT ( 'NONE',  ( 184.8905102610680444, 20.92133201514447549, 0.000000000000000000 ) ) ;
#17222 = CARTESIAN_POINT ( 'NONE',  ( -198.0356074513804288, -39.15871834505936278, 39.15871834505892224 ) ) ;
#17223 = CARTESIAN_POINT ( 'NONE',  ( -192.9588430854690273, -14.46834944099973264, -40.00000000000002132 ) ) ;
#17225 = CARTESIAN_POINT ( 'NONE',  ( 91.82158438592158234, 7.693928927950222250E-14, -17.20528682183300262 ) ) ;
#17224 = CARTESIAN_POINT ( 'NONE',  ( -259.2033419157646676, -35.01439189186523748, -21.55415060305881170 ) ) ;
#17226 = CARTESIAN_POINT ( 'NONE',  ( 57.59792236341147031, -2.435789363418150444, 0.000000000000000000 ) ) ;
#17227 = CARTESIAN_POINT ( 'NONE',  ( 19.06497207195980792, -18.24870850772763475, 38.31983398719622613 ) ) ;
#17228 = CARTESIAN_POINT ( 'NONE',  ( -86.96347745069644475, 18.24025645688351105, 2.449293598294708485E-15 ) ) ;
#17229 = VERTEX_POINT ( 'NONE', #1308 ) ;
#17230 = CARTESIAN_POINT ( 'NONE',  ( 8.209392600961981756, -44.89226883836379045, 24.84362085273889065 ) ) ;
#17231 = AXIS2_PLACEMENT_3D ( 'NONE', #7541, #21283, #9543 ) ;
#17232 = CARTESIAN_POINT ( 'NONE',  ( -135.8532207217289738, 30.84685318188643777, -40.00000000000002132 ) ) ;
#17233 = CARTESIAN_POINT ( 'NONE',  ( -716.9846540392142060, 0.000000000000000000, -44.99999999999997158 ) ) ;
#17234 = CARTESIAN_POINT ( 'NONE',  ( 4.995406935893290878, 39.06748935135185263, 39.06748935135198764 ) ) ;
#17235 = CARTESIAN_POINT ( 'NONE',  ( -238.4067589809705794, -4.716212492215116094E-14, 0.9644942799825824142 ) ) ;
#17236 = CARTESIAN_POINT ( 'NONE',  ( -82.23757706630857456, 20.18845287563442170, 0.8296373908661033303 ) ) ;
#17237 = AXIS2_PLACEMENT_3D ( 'NONE', #18420, #8178, #6574 ) ;
#17238 = CIRCLE ( 'NONE', #21081, 30.00000000000000355 ) ;
#17239 = AXIS2_PLACEMENT_3D ( 'NONE', #23039, #18498, #4814 ) ;
#17240 = CARTESIAN_POINT ( 'NONE',  ( -77.90022806218999563, 8.352332316461417605, -20.16431395584788433 ) ) ;
#17241 = CARTESIAN_POINT ( 'NONE',  ( 199.9999999999998295, 0.2943743412949595961, 19.00910698902408669 ) ) ;
#17242 = CARTESIAN_POINT ( 'NONE',  ( -208.1127848780265026, 10.60833733269551615, -10.60833733269529766 ) ) ;
#17243 = CARTESIAN_POINT ( 'NONE',  ( 169.9999999999999432, -21.59613885783095100, 12.70659020859084620 ) ) ;
#17244 = CARTESIAN_POINT ( 'NONE',  ( -135.8532207217289738, -6.472252184284280396, 6.472252184284099208 ) ) ;
#17245 = CARTESIAN_POINT ( 'NONE',  ( -198.0356074513804572, 17.40982414986501325, -39.15871834505897198 ) ) ;
#17246 = ADVANCED_FACE ( 'NONE', ( #9675 ), #25536, .F. ) ;
#17247 = CARTESIAN_POINT ( 'NONE',  ( 170.2234770963711128, 17.36149277826973503, 39.20704971665401217 ) ) ;
#17248 = CARTESIAN_POINT ( 'NONE',  ( -77.90255099906769942, -20.29001641120661859, 8.064892378658379712 ) ) ;
#17249 = CARTESIAN_POINT ( 'NONE',  ( -30.26275506840324070, -1.198031551616016266, -1.198031551616031587 ) ) ;
#17250 = CIRCLE ( 'NONE', #5780, 4.999999999999962697 ) ;
#17252 = CARTESIAN_POINT ( 'NONE',  ( -259.2033419157646676, -6.730120644403663199, 6.730120644403451813 ) ) ;
#17251 = DIRECTION ( 'NONE',  ( 0.9352143323239846540, 0.3271292299042263818, -0.1355013636760585005 ) ) ;
#17253 = CARTESIAN_POINT ( 'NONE',  ( 192.4448373802101173, 42.42640687116487896, 14.14213562375934075 ) ) ;
#17254 = CARTESIAN_POINT ( 'NONE',  ( -213.1075012329537230, 13.71589010951907994, 0.000000000000000000 ) ) ;
#17255 = CARTESIAN_POINT ( 'NONE',  ( -213.1075012329537230, 37.98287015391236565, -18.58567234101138510 ) ) ;
#17256 = CARTESIAN_POINT ( 'NONE',  ( -348.0000000000001137, -4.857225732735059864E-14, 0.000000000000000000 ) ) ;
#17257 = CARTESIAN_POINT ( 'NONE',  ( -30.26275506840322294, -57.76657404653985139, -1.198031551616531853 ) ) ;
#17258 = EDGE_CURVE ( 'NONE', #8490, #15233, #14046, .T. ) ;
#17259 = CARTESIAN_POINT ( 'NONE',  ( -129.2303492452213334, 24.84170067253468162, -11.67678589738752670 ) ) ;
#17260 = EDGE_LOOP ( 'NONE', ( #14951, #12347 ) ) ;
#17261 = PRESENTATION_LAYER_ASSIGNMENT (  '', '', ( #18539 ) ) ;
#17262 = CARTESIAN_POINT ( 'NONE',  ( 170.2234770963711128, 10.92277846919201068, 10.92277846919202133 ) ) ;
#17263 = DIRECTION ( 'NONE',  ( -1.000000000000000000, -1.836970198721030181E-16, -0.000000000000000000 ) ) ;
#17264 = CARTESIAN_POINT ( 'NONE',  ( 20.69615274311417963, 13.93598092273866840, 47.71500688528227130 ) ) ;
#17265 = CARTESIAN_POINT ( 'NONE',  ( -70.28815428308283231, -22.81668038576722424, -9.450978466024738012 ) ) ;
#17266 = ORIENTED_EDGE ( 'NONE', *, *, #10146, .T. ) ;
#17267 = CARTESIAN_POINT ( 'NONE',  ( -144.0562564041998712, -31.27039870039539338, 10.50946916240340201 ) ) ;
#17268 = CARTESIAN_POINT ( 'NONE',  ( 200.0000000000000000, -14.79283710360616944, -11.93388616463377438 ) ) ;
#17269 = AXIS2_PLACEMENT_3D ( 'NONE', #13827, #24224, #7835 ) ;
#17270 = CARTESIAN_POINT ( 'NONE',  ( 22.70429368897842437, -17.89136451867717881, 43.19357487035005505 ) ) ;
#17271 = B_SPLINE_CURVE_WITH_KNOTS ( 'NONE', 3,
 ( #681, #25034, #2278, #417, #16371, #8790, #279, #8521, #2816, #6787, #19036, #14507 ),
 .UNSPECIFIED., .F., .F.,
 ( 4, 2, 2, 2, 2, 4 ),
 ( 1.398578778534940505E-17, 0.004680202113614262589, 0.009360404227228511301, 0.01170050528403563696, 0.01404060634084276088, 0.01872080845445705036 ),
 .UNSPECIFIED. ) ;
#17272 = CARTESIAN_POINT ( 'NONE',  ( 60.28378959960998174, 15.72633063278336785, -31.18416451506176656 ) ) ;
#17273 = CARTESIAN_POINT ( 'NONE',  ( 199.0155347402294410, 14.70064717653387554, 13.56132639103557125 ) ) ;
#17274 = CARTESIAN_POINT ( 'NONE',  ( 146.6084372240433709, -32.08495691632075619, 24.48358557860298035 ) ) ;
#17275 = CARTESIAN_POINT ( 'NONE',  ( -86.96347745069644475, 5.999880687339585546E-14, -21.75974354311649961 ) ) ;
#17277 = AXIS2_PLACEMENT_3D ( 'NONE', #25731, #3247, #9620 ) ;
#17276 = DIRECTION ( 'NONE',  ( 0.000000000000000000, 1.000000000000000000, 0.000000000000000000 ) ) ;
#17278 = EDGE_CURVE ( 'NONE', #2697, #17673, #11800, .T. ) ;
#17279 = DIRECTION ( 'NONE',  ( -1.303213150798907793E-16, 1.000000000000000000, -1.682156097916904081E-16 ) ) ;
#17280 = CARTESIAN_POINT ( 'NONE',  ( 184.8905102610680444, 20.92133201514447194, -40.00000000000002132 ) ) ;
#17282 = CARTESIAN_POINT ( 'NONE',  ( -618.4965464916332394, 27.78215535369033873, 28.77840465361206412 ) ) ;
#17281 = CARTESIAN_POINT ( 'NONE',  ( 23.40652632868016880, -13.79856377312466975, -46.79646383233838947 ) ) ;
#17283 = CARTESIAN_POINT ( 'NONE',  ( -280.0000000000000000, 19.99999999999996092, -0.000000000000000000 ) ) ;
#17284 = CARTESIAN_POINT ( 'NONE',  ( -135.8532207217289738, 6.472252184284186249, -6.472252184284142729 ) ) ;
#17285 = CARTESIAN_POINT ( 'NONE',  ( -192.9588430854690273, 40.00000000000014211, -14.46834944099927966 ) ) ;
#17286 = CARTESIAN_POINT ( 'NONE',  ( -110.0471271032897960, 8.580892274481946913, -18.26740471933098675 ) ) ;
#17287 = CARTESIAN_POINT ( 'NONE',  ( 136.1360204305621551, -39.99999999999994316, -4.966164525587488221 ) ) ;
#17288 = CARTESIAN_POINT ( 'NONE',  ( 126.3221657595859568, -28.30549010001853816, -11.72451788904508696 ) ) ;
#17289 = CARTESIAN_POINT ( 'NONE',  ( 130.8568914410475372, -24.07718906447255947, 24.07718906447199458 ) ) ;
#17290 = CARTESIAN_POINT ( 'NONE',  ( -208.1127848780264742, 17.67593391476624021, 38.89260858015742883 ) ) ;
#17291 = EDGE_CURVE ( 'NONE', #22653, #11219, #3264, .T. ) ;
#17292 = ADVANCED_FACE ( 'NONE', ( #24181 ), #3972, .F. ) ;
#17293 = ORIENTED_EDGE ( 'NONE', *, *, #6153, .F. ) ;
#17295 = CARTESIAN_POINT ( 'NONE',  ( 12.77879914706121234, 44.80239647191536534, -18.55776024547099823 ) ) ;
#17294 = DIRECTION ( 'NONE',  ( 0.000000000000000000, 1.000000000000000000, 0.000000000000000000 ) ) ;
#17296 = CARTESIAN_POINT ( 'NONE',  ( 192.4448373802101173, -19.99999999996057554, 40.00000000000002132 ) ) ;
#17297 = CARTESIAN_POINT ( 'NONE',  ( -259.2033419157646676, -6.730120644403663199, 6.730120644403451813 ) ) ;
#17298 = CARTESIAN_POINT ( 'NONE',  ( -192.9370391624948411, 48.35015248260834397, -14.03127550870980222 ) ) ;
#17299 = DIRECTION ( 'NONE',  ( 0.000000000000000000, 0.000000000000000000, 1.000000000000000000 ) ) ;
#17300 = ORIENTED_EDGE ( 'NONE', *, *, #4702, .T. ) ;
#17301 = VERTEX_POINT ( 'NONE', #10076 ) ;
#17302 = CARTESIAN_POINT ( 'NONE',  ( -86.96347745069644475, 15.38646221621793586, -15.38646221621778842 ) ) ;
#17303 = CARTESIAN_POINT ( 'NONE',  ( 98.29820294267318559, -18.47759065023121039, -7.653668647304145090 ) ) ;
#17304 = VERTEX_POINT ( 'NONE', #20325 ) ;
#17305 = ORIENTED_EDGE ( 'NONE', *, *, #3959, .F. ) ;
#17306 = CARTESIAN_POINT ( 'NONE',  ( 199.9999999999999147, -8.688421465551046552, 16.91138275242808575 ) ) ;
#17307 = CARTESIAN_POINT ( 'NONE',  ( -280.0000000000000000, -14.14213562373118371, 14.14213562373078936 ) ) ;
#17308 = CARTESIAN_POINT ( 'NONE',  ( 14.38125909742181285, -17.55144818341476309, 39.01709431150910490 ) ) ;
#17309 = CARTESIAN_POINT ( 'NONE',  ( 210.0000000000000284, 63.70262460423112572, -57.69613583541415380 ) ) ;
#17310 = CARTESIAN_POINT ( 'NONE',  ( -162.0762913951020892, -3.568845385355699554E-14, 1.694272876828323948 ) ) ;
#17311 = CARTESIAN_POINT ( 'NONE',  ( 190.0000000000001137, -30.00000000000000711, 3.673940397442064700E-15 ) ) ;
#17312 = DIRECTION ( 'NONE',  ( 0.000000000000000000, -0.3028247695821854046, 0.9530462522498561739 ) ) ;
#17313 = CARTESIAN_POINT ( 'NONE',  ( -30.26275506840323359, -39.99999999999959499, -41.69427246844670520 ) ) ;
#17314 = CARTESIAN_POINT ( 'NONE',  ( -162.0762913951021176, 40.00000000000042633, -41.69427287672947102 ) ) ;
#17315 = FACE_OUTER_BOUND ( 'NONE', #2160, .T. ) ;
#17316 = CARTESIAN_POINT ( 'NONE',  ( 57.59792236341147031, 1.722363176415065089, -1.722363176415036445 ) ) ;
#17317 = CARTESIAN_POINT ( 'NONE',  ( -200.0000000000000000, -52.49999999999972289, -82.49999999999998579 ) ) ;
#17318 = CARTESIAN_POINT ( 'NONE',  ( -192.9370391625626837, 14.03127550871173668, 48.35015248262227772 ) ) ;
#17319 = DIRECTION ( 'NONE',  ( -1.000000000000000000, 0.000000000000000000, 0.000000000000000000 ) ) ;
#17320 = CARTESIAN_POINT ( 'NONE',  ( -77.55672185583976841, 16.64541244683857713, -14.65061613763128534 ) ) ;
#17321 = DIRECTION ( 'NONE',  ( 1.000000000000000000, 1.836970198721030181E-16, 0.000000000000000000 ) ) ;
#17322 = CARTESIAN_POINT ( 'NONE',  ( -77.84504298479346573, -19.81984129311347331, 9.297284891546427232 ) ) ;
#17323 = CARTESIAN_POINT ( 'NONE',  ( -105.3755690713226727, 12.89780903124400879, 12.89780903124407452 ) ) ;
#17324 = CARTESIAN_POINT ( 'NONE',  ( -238.4067589809705794, -28.96627169325352469, 27.60227080167035041 ) ) ;
#17325 = CARTESIAN_POINT ( 'NONE',  ( -660.0479240540959154, 43.50642481262257633, -11.71509576873842740 ) ) ;
#17326 = DIRECTION ( 'NONE',  ( 0.000000000000000000, 1.000000000000000000, 0.000000000000000000 ) ) ;
#17327 = VERTEX_POINT ( 'NONE', #7937 ) ;
#17328 = CARTESIAN_POINT ( 'NONE',  ( 91.82158438592158234, 44.40256751092319121, 12.16597498400105515 ) ) ;
#17329 = CARTESIAN_POINT ( 'NONE',  ( 23.37394308801976450, 13.80096434448266685, 46.80823611210199431 ) ) ;
#17330 = DIRECTION ( 'NONE',  ( 0.000000000000000000, -1.000000000000000000, -0.000000000000000000 ) ) ;
#17331 = ORIENTED_EDGE ( 'NONE', *, *, #15952, .F. ) ;
#17332 = CARTESIAN_POINT ( 'NONE',  ( 146.6084372240433709, -40.00000000000036238, 34.62501878078263218 ) ) ;
#17333 = CARTESIAN_POINT ( 'NONE',  ( -3.069599232962567648, -23.65302469262814000, 43.28003856805346317 ) ) ;
#17334 = CARTESIAN_POINT ( 'NONE',  ( 3.854700064722261565, -44.60002223906898422, 24.62824689552009261 ) ) ;
#17335 = ORIENTED_EDGE ( 'NONE', *, *, #25881, .F. ) ;
#17336 = VERTEX_POINT ( 'NONE', #12460 ) ;
#17337 = UNCERTAINTY_MEASURE_WITH_UNIT (LENGTH_MEASURE( 1.000000000000000082E-05 ), #12387, 'distance_accuracy_value', 'NONE');
#17338 = CARTESIAN_POINT ( 'NONE',  ( -195.1685814578706015, -44.46431112711578493, -24.52825302094467830 ) ) ;
#17339 = CARTESIAN_POINT ( 'NONE',  ( 57.59792236341146321, 40.00000000000004263, -2.435789363418021214 ) ) ;
#17340 = CARTESIAN_POINT ( 'NONE',  ( -716.9846540392142060, 5.510910596163085611E-15, 44.99999999999997158 ) ) ;
#17341 = B_SPLINE_CURVE_WITH_KNOTS ( 'NONE', 3,
 ( #8577, #4207, #16688, #24820, #16292, #16157 ),
 .UNSPECIFIED., .F., .F.,
 ( 4, 2, 4 ),
 ( 1.484016138952788438E-15, 0.03937685683732576603, 0.07875371367465004713 ),
 .UNSPECIFIED. ) ;
#17342 = FACE_BOUND ( 'NONE', #6630, .T. ) ;
#17343 = CARTESIAN_POINT ( 'NONE',  ( 4.995406935893297984, -40.00000000000007816, 15.24977328854818914 ) ) ;
#17344 = CARTESIAN_POINT ( 'NONE',  ( 199.9999999999999147, -13.00175152101318510, -13.87559618198639022 ) ) ;
#17345 = CYLINDRICAL_SURFACE ( 'NONE', #5809, 39.99999999999994316 ) ;
#17346 = CARTESIAN_POINT ( 'NONE',  ( 91.82158438592158234, -12.16597498397778843, 12.16597498397750954 ) ) ;
#17347 = CARTESIAN_POINT ( 'NONE',  ( 0.2972598230769923355, 18.14793986248751168, -38.42060263243650553 ) ) ;
#17348 = CARTESIAN_POINT ( 'NONE',  ( -89.91461477837958682, 20.29478540188764413, 8.406375358913457774 ) ) ;
#17349 = CARTESIAN_POINT ( 'NONE',  ( -198.0356074513804572, 5.461327841961909642E-13, -55.37879056873073580 ) ) ;
#17350 = CARTESIAN_POINT ( 'NONE',  ( 98.29820294272414571, 7.653668647302724892, 18.47759065022804137 ) ) ;
#17351 = CARTESIAN_POINT ( 'NONE',  ( 199.9999999999999432, 20.00000000000013856, 0.000000000000000000 ) ) ;
#17352 = CARTESIAN_POINT ( 'NONE',  ( 19.06497207195981858, -10.03556273973469715, 66.60410523465813526 ) ) ;
#17353 = CARTESIAN_POINT ( 'NONE',  ( 170.2234770963711128, 24.55285855007190676, -40.00000000000002132 ) ) ;
#17354 = EDGE_CURVE ( 'NONE', #6105, #9566, #9939, .T. ) ;
#17356 = CARTESIAN_POINT ( 'NONE',  ( 163.1118516004056573, 1.251511021549353291E-13, -27.26290988616872824 ) ) ;
#17355 = CARTESIAN_POINT ( 'NONE',  ( 21.15138808362603839, -43.47948264999420331, -23.80076113581845831 ) ) ;
#17357 = CARTESIAN_POINT ( 'NONE',  ( -280.0000000000000000, 14.14213562373088351, 14.14213562373098654 ) ) ;
#17358 = CARTESIAN_POINT ( 'NONE',  ( 91.82158438592158234, 22.79471317813472098, 2.449293598294708485E-15 ) ) ;
#17360 = ORIENTED_EDGE ( 'NONE', *, *, #15447, .F. ) ;
#17359 = AXIS2_PLACEMENT_3D ( 'NONE', #7477, #19722, #13730 ) ;
#17361 = CARTESIAN_POINT ( 'NONE',  ( 17.24092899316222827, -44.34059580270437095, 18.36647614520138205 ) ) ;
#17362 = LINE ( 'NONE', #25499, #4735 ) ;
#17363 = CARTESIAN_POINT ( 'NONE',  ( -86.96347745069644475, -15.38646221621796073, 41.18208027870593924 ) ) ;
#17364 = CARTESIAN_POINT ( 'NONE',  ( 4.995406935893290878, -5.232665749138292703E-14, 15.24977328854832592 ) ) ;
#17365 = CARTESIAN_POINT ( 'NONE',  ( -77.58090675230904765, 21.99687198915249908, -2.639383879333266236 ) ) ;
#17366 = B_SPLINE_CURVE_WITH_KNOTS ( 'NONE', 3,
 ( #18520, #301, #2173, #8008, #12525, #20263 ),
 .UNSPECIFIED., .F., .F.,
 ( 4, 2, 4 ),
 ( -6.000000000146255584E-08, 0.04016968421219987984, 0.08033942842439978360 ),
 .UNSPECIFIED. ) ;
#17367 = CARTESIAN_POINT ( 'NONE',  ( 22.40986519363266538, -13.85314893102481903, -47.15972762675180974 ) ) ;
#17368 = CARTESIAN_POINT ( 'NONE',  ( 199.9999999999999147, -9.100092698529554269, 16.69133291234032868 ) ) ;
#17369 = CARTESIAN_POINT ( 'NONE',  ( -655.2474585732728656, 38.71397089290621807, -10.07298238254288769 ) ) ;
#17370 = CARTESIAN_POINT ( 'NONE',  ( -77.55632011649659319, 0.6824138086283418891, -22.13182254413152705 ) ) ;
#17371 = CARTESIAN_POINT ( 'NONE',  ( 184.8905102610680444, 13.49065550809757497, 43.07788698682593065 ) ) ;
#17372 = VECTOR ( 'NONE', #10184, 1000.000000000000000 ) ;
#17373 = CARTESIAN_POINT ( 'NONE',  ( 136.1360204305621266, 53.05693388239320285, -3.511608612530223716 ) ) ;
#17374 = CARTESIAN_POINT ( 'NONE',  ( 192.4448373802101173, 14.14213562375862665, 42.42640687116509213 ) ) ;
#17375 = DIRECTION ( 'NONE',  ( -1.000000000000000000, 1.836970198721030181E-16, 0.000000000000000000 ) ) ;
#17376 = CARTESIAN_POINT ( 'NONE',  ( -56.48582580120558561, -21.81201906317755146, -21.81201906317792449 ) ) ;
#17378 = CARTESIAN_POINT ( 'NONE',  ( -280.0000000000000000, -14.14213562373118549, 14.14213562373078936 ) ) ;
#17377 = CARTESIAN_POINT ( 'NONE',  ( 163.1118516004056573, 19.27778845539265618, -37.29075403953135037 ) ) ;
#17379 = CARTESIAN_POINT ( 'NONE',  ( -105.3755690713226585, -15.38646221621738164, -41.18208027870615240 ) ) ;
#17380 = CARTESIAN_POINT ( 'NONE',  ( 184.8905102610680444, -20.92133201514440799, -40.00000000000002132 ) ) ;
#17381 = CYLINDRICAL_SURFACE ( 'NONE', #13624, 39.99999999999994316 ) ;
#17382 = CARTESIAN_POINT ( 'NONE',  ( -210.0000000000000284, -66.50000000000001421, -66.50000000000005684 ) ) ;
#17383 = CARTESIAN_POINT ( 'NONE',  ( 57.59792236341147031, -26.56190807104712448, 30.00663442387673285 ) ) ;
#17384 = CARTESIAN_POINT ( 'NONE',  ( -188.2870673237731012, 43.00153493964115370, -23.44688076656412434 ) ) ;
#17385 = VERTEX_POINT ( 'NONE', #5955 ) ;
#17386 = CARTESIAN_POINT ( 'NONE',  ( 0.2972598230769907257, 66.70487387989857098, 10.13633138497486641 ) ) ;
#17387 = CARTESIAN_POINT ( 'NONE',  ( -77.78737254111192101, -19.58908437138761727, -9.951945538203670338 ) ) ;
#17388 = CARTESIAN_POINT ( 'NONE',  ( 37.15749683965372441, 12.76981037574219968, 41.79699086514150252 ) ) ;
#17389 = CARTESIAN_POINT ( 'NONE',  ( -39.81953879990965817, -34.34246706537491889, -11.17638696932914932 ) ) ;
#17390 = EDGE_LOOP ( 'NONE', ( #2454, #20720, #23016, #1043, #25589, #24071, #15289 ) ) ;
#17391 = CARTESIAN_POINT ( 'NONE',  ( -188.8383598209452998, -43.28885971699677526, 17.93083279444634215 ) ) ;
#17392 = CARTESIAN_POINT ( 'NONE',  ( 200.0000000000000284, -8.407999580957739028, -17.04516676560209376 ) ) ;
#17393 = CARTESIAN_POINT ( 'NONE',  ( 22.92196489051308816, -13.82589419143179121, 46.97629733301284460 ) ) ;
#17394 = AXIS2_PLACEMENT_3D ( 'NONE', #16512, #14904, #18638 ) ;
#17395 = CARTESIAN_POINT ( 'NONE',  ( -112.9836683000657587, 19.65633339690261749, 8.141919879520816750 ) ) ;
#17396 = CARTESIAN_POINT ( 'NONE',  ( 199.0062801237116332, 7.031410157601610145, -18.72090521856086198 ) ) ;
#17397 = CARTESIAN_POINT ( 'NONE',  ( -77.55640685876514340, -1.398619866344356533, 22.13135000837099753 ) ) ;
#17398 = CARTESIAN_POINT ( 'NONE',  ( -259.2033419157646676, 40.00000000000000711, -9.517827891722491884 ) ) ;
#17399 = CARTESIAN_POINT ( 'NONE',  ( 57.59792236341147031, 1.908507979671054758E-14, -2.435789363418160658 ) ) ;
#17400 = LINE ( 'NONE', #9419, #24912 ) ;
#17401 = CARTESIAN_POINT ( 'NONE',  ( -213.1075012329537230, -53.71589010953668719, -40.00000000000002132 ) ) ;
#17403 = CARTESIAN_POINT ( 'NONE',  ( -601.6837166637907330, 36.60574833829470265, -16.14880282736276840 ) ) ;
#17402 = CARTESIAN_POINT ( 'NONE',  ( 67.67011021016655548, -12.13550330130990851, -29.29769665558049851 ) ) ;
#17404 = CARTESIAN_POINT ( 'NONE',  ( -162.0762913951021176, -1.694272876828353702, 40.00000000000002132 ) ) ;
#17405 = CARTESIAN_POINT ( 'NONE',  ( 192.4448373802100889, 14.14213562375893574, -14.14213562375874922 ) ) ;
#17406 = CARTESIAN_POINT ( 'NONE',  ( 151.7948205124836250, -3.202120068677277203E-13, 33.23291073765553705 ) ) ;
#17407 = CARTESIAN_POINT ( 'NONE',  ( -91.56559293963834989, -40.00000000000027711, 22.67402823373149801 ) ) ;
#17408 = CIRCLE ( 'NONE', #4634, 5.000000000000046185 ) ;
#17409 = B_SPLINE_SURFACE_WITH_KNOTS ( 'NONE', 1, 3, ( 
 ( #4273, #10111, #14228, #14364, #8238, #4144, #12361, #2395, #11971, #24754, #6374, #26236, #18212, #12236, #20492, #8106, #8373, #2135, #10373, #6508, #264, #18483, #14618, #6120, #18354, #3869, #22228, #14492, #20619, #24620, #18621, #2005, #10507, #1874, #22625, #4400, #20095, #12494, #20360, #9977, #18085, #7970, #16089, #24219, #22367, #5990, #14099, #134, #4004, #12103, #16356, #24489, #20227, #24356, #6251, #21152, #2797, #17014, #13034, #10773, #5053, #2668, #14884, #535, #1055, #7158, #25151, #12630, #800, #6902, #7028, #21279, #2926, #18886, #15019, #8640, #4799, #664, #16750, #19021, #8773, #14752, #17273, #20757, #16887, #22753, #23149, #22883, #12764, #12900, #25018, #21015, #4661, #11035, #11157, #4921, #20889, #17144, #9039, #24882, #10909, #2527, #25278, #6638, #8904, #19145, #6772, #15147, #19272, #18752, #4532, #929, #23277, #10644, #13159, #3050, #9160, #25406, #23023, #25787, #13786, #17522, #21921, #1703, #21654, #5179, #11282, #17778, #3426, #13530, #17914, #5681, #23524, #25924, #23648, #5427, #15518, #3304, #11527, #15274, #19652, #15400, #1438, #7405, #9537, #17646, #9810, #7537, #19522, #1307, #23404, #15649, #7284, #5296, #23774, #9415, #5551, #13404, #13660, #3693, #21783, #21529, #9674, #1569, #9290, #3556, #13282, #7665, #17396, #11659, #19783, #25660, #15776, #11799, #19403, #21404, #23905, #19919, #3177, #26057, #1185, #25535, #11399, #8204, #18314, #6338, #10075, #14460, #20585, #14194, #24043, #3832, #10339, #22326, #6087, #10473, #24582, #16054, #18448, #16189, #24322, #8070, #22194, #4101, #7795, #12202, #7936, #20323, #26329, #2100, #10209, #2360, #96, #12068, #16322, #12458, #18180, #24449, #18588, #26199, #224, #22591, #6215, #4368, #5954, #15911, #5821, #8338, #14327, #13924, #20457, #22459, #22059, #16460, #11933, #2231, #20060, #4239, #1837, #9938, #12329, #18046, #24179, #14063, #3971, #20186, #1970, #22853, #25119, #6739, #20985, #16983, #14721, #9008, #6601, #18853, #4493, #5023, #11131, #2766, #16587, #4763, #10875, #11005, #25245, #6871, #4628, #18989, #12595, #8739, #12731, #20725, #22987, #20853, #18716, #21249, #24719, #2898, #6474, #13001, #8468, #10742, #6996, #14588, #12867, #23248, #365, #2633, #633, #4891, #16857, #24988, #14985, #14851, #767, #23119, #8873, #17115 ),
 ( #21121, #19115, #898, #15117, #8608, #13128, #10604, #22716, #3024, #2493, #501, #16717, #24849, #21885, #11499, #25761, #17368, #5270, #17491, #19625, #23374, #15748, #1410, #17616, #13373, #5150, #19370, #7254, #15619, #3662, #7633, #5652, #11372, #19244, #25379, #13255, #15243, #25633, #21378, #17241, #9646, #3148, #19751, #11251, #1027, #23742, #7379, #9126, #1541, #13501, #25892, #1157, #23876, #15373, #13758, #3399, #25505, #9261, #9511, #7131, #19493, #23496, #21503, #3274, #1277, #9384, #15490, #21623, #7509, #5523, #23618, #5400, #13630, #21754, #3528, #11629, #17749, #19889, #8305, #14299, #7767, #18016, #12038, #12175, #26164, #16294, #10047, #18284, #24557, #8179, #8042, #6060, #4209, #22433, #1807, #24420, #20029, #18152, #20295, #15881, #16431, #2073, #10180, #5926, #24008, #11904, #7905, #6184, #22561, #197, #6312, #3941, #11770, #17881, #5788, #13895, #26300, #22029, #9779, #2206, #3802, #12300, #9910, #1672, #20427, #16159, #26030, #10315, #14164, #18421, #16024, #14431, #24149, #14033, #22297, #22164, #20158, #70, #1939, #24293, #4073, #8579, #2464, #20560, #19092, #605, #24963, #18962, #22955, #10574, #14694, #14823, #8712, #4603, #4733, #2874, #12432, #872, #6841, #337, #18689, #12700, #12843, #473, #8847, #2602, #10844, #17088, #743, #16826, #6709, #23096, #14961, #20696, #16956, #12563, #10716, #8980, #2331, #10441, #8441, #22827, #18558, #25220, #4867, #16560, #6973, #16690, #20828, #20959, #24688, #2740, #24822, #6445, #12971, #25094, #6575, #14561, #21092, #10982, #15087, #18825, #4340, #22692, #4467, #9236, #17466, #3246, #15592, #25727, #11602, #5126, #5244, #7107, #11102, #7479, #9618, #21225, #1000, #19725, #25863, #15465, #3369, #21353, #17344, #21468, #9103, #19219, #11350, #25350, #2998, #13598, #17212, #23717, #15219, #4999, #1384, #19466, #13104, #5498, #25609, #3504, #23349, #1511, #19342, #17722, #7352, #3122, #13230, #13476, #11226, #23473, #7607, #1132, #25480, #7229, #23220, #1253, #23592, #11470, #5371, #15347, #13349, #21598, #9357, #19596, #9485, #21728, #17589, #12274, #18255, #11739, #21998, #15994, #16127, #3768, #20266, #14001, #22268, #2176, #12142, #12011, #10014, #8148, #36, #5757, #2045, #23980, #22131, #4180, #13732, #5626, #19858, #7872, #21858, #20402, #16263, #3632 ) ),
 .UNSPECIFIED., .F., .T., .F.,
 ( 2, 2 ),
 ( 4, 2, 2, 2, 2, 2, 2, 2, 2, 2, 2, 2, 2, 2, 2, 2, 2, 2, 2, 2, 2, 2, 2, 2, 2, 2, 2, 2, 2, 2, 2, 2, 2, 2, 2, 2, 2, 2, 2, 2, 2, 2, 2, 2, 2, 2, 2, 2, 2, 2, 2, 2, 2, 2, 2, 2, 2, 2, 2, 2, 2, 2, 2, 2, 2, 2, 2, 2, 2, 2, 2, 2, 2, 2, 2, 2, 2, 2, 2, 2, 2, 2, 2, 2, 2, 2, 2, 2, 2, 2, 2, 2, 2, 2, 2, 2, 2, 2, 2, 2, 2, 2, 2, 2, 2, 2, 2, 2, 2, 2, 2, 2, 2, 2, 2, 2, 2, 2, 2, 2, 2, 2, 2, 2, 2, 2, 2, 2, 2, 2, 2, 2, 2, 2, 2, 2, 2, 2, 2, 2, 2, 2, 2, 2, 2, 2, 2, 2, 4 ),
 ( 0.000000000000000000, 1.000000000000000000 ),
 ( 0.001986339241202381145, 0.003842975313193646575, 0.004771293349189279290, 0.005235452367187095647, 0.005699611385184912005, 0.006163770403182728362, 0.006627929421180544720, 0.007092088439178361077, 0.007556247457176177434, 0.008484565493171810149, 0.009412883529167442864, 0.01034120156516307558, 0.01126951960115870829, 0.01173367861915652552, 0.01219783763715434101, 0.01266199665515215650, 0.01312615567314997372, 0.01405447370914560644, 0.01498279174514123915, 0.01683942781713250458, 0.01776774585312813903, 0.01869606388912377001, 0.01916022290712158377, 0.01962438192511940099, 0.02008854094311721822, 0.02055269996111503544, 0.02148101799711066989, 0.02240933603310630087, 0.02333765406910193185, 0.02426597210509756630, 0.02519429014109320075, 0.02565844915909101798, 0.02612260817708883173, 0.02658676719508664549, 0.02705092621308446271, 0.02797924424908009716, 0.02983588032107136259, 0.03076419835706699357, 0.03122835737506481080, 0.03169251639306262802, 0.03215667541106044525, 0.03262083442905826247, 0.03354915246505389692, 0.03447747050104953137, 0.03540578853704515888, 0.03633410657304078639, 0.03726242460903642084, 0.03772658362703423807, 0.03819074264503205529, 0.03865490166302987252, 0.03911906068102768974, 0.04004737871702332419, 0.04097569675301895864, 0.04283233282501022060, 0.04376065086100584811, 0.04468896889700148256, 0.04561728693299711701, 0.04654560496899275146, 0.04840224104098402036, 0.04933055907697965481, 0.05025887711297528232, 0.05072303613097309261, 0.05118719514897090983, 0.05165135416696872706, 0.05211551318496654428, 0.05304383122096217873, 0.05397214925695781318, 0.05490046729295344763, 0.05582878532894908208, 0.05675710336494471653, 0.05722126238294253375, 0.05768542140094034404, 0.05814958041893815432, 0.05861373943693597155, 0.05954205747293160600, 0.06139869354492287490, 0.06325532961691412992, 0.06511196568890539882, 0.06604028372490103327, 0.06696860176089666772, 0.06743276077889448494, 0.06789691979689230217, 0.06836107881489011939, 0.06882523783288793662, 0.06975355586888357107, 0.07068187390487920552, 0.07161019194087483997, 0.07253850997687047442, 0.07300266899486829164, 0.07346682801286610887, 0.07393098703086392609, 0.07439514604886174332, 0.07485930506685956054, 0.07532346408485737776, 0.07625178212085299834, 0.07810841819284425336, 0.07903673622883988781, 0.07950089524683770503, 0.07996505426483552226, 0.08042921328283333948, 0.08089337230083115671, 0.08182169033682679116, 0.08275000837282242561, 0.08367832640881806006, 0.08460664444481369451, 0.08553496248080932896, 0.08646328051680496340, 0.08692743953480278063, 0.08739159855280059785, 0.08785575757079841508, 0.08831991658879623230, 0.08924823462479186675, 0.09110487069678312178, 0.09203318873277874235, 0.09296150676877437680, 0.09342566578677219402, 0.09388982480477001125, 0.09435398382276782847, 0.09481814284076564570, 0.09574646087676128015, 0.09667477891275691460, 0.09760309694875254904, 0.09853141498474818349, 0.09899557400274600072, 0.09945973302074381794, 0.09992389203874163517, 0.1003880510567394524, 0.1022446871287307213, 0.1041013232007219902, 0.1050296412367176246, 0.1054938002547154419, 0.1059579592727132452, 0.1064221182907110486, 0.1068862773087088658, 0.1078145953447045002, 0.1096712314166957691, 0.1105995494526914036, 0.1115278674886870380, 0.1124561855246826725, 0.1133845035606783069, 0.1143128215966739414, 0.1152411396326695758, 0.1170977757046608447, 0.1180260937406564792, 0.1184902527586542964, 0.1189544117766521136, 0.1194185707946499309, 0.1198827298126477481, 0.1208110478486433687 ),
 .UNSPECIFIED. ) ;
#17410 = CARTESIAN_POINT ( 'NONE',  ( 105.6376868227169297, -21.14845495492350480, -8.759976865565771931 ) ) ;
#17411 = ORIENTED_EDGE ( 'NONE', *, *, #15250, .F. ) ;
#17413 = CARTESIAN_POINT ( 'NONE',  ( -4.037857402784110761, 46.99101396955047250, -13.82822410908676858 ) ) ;
#17412 = CARTESIAN_POINT ( 'NONE',  ( -350.0000000000001137, 20.53474504356807273, 0.000000000000000000 ) ) ;
#17414 = CARTESIAN_POINT ( 'NONE',  ( -208.1127848780264742, -15.00245453012673202, 40.00000000000002132 ) ) ;
#17415 = AXIS2_PLACEMENT_3D ( 'NONE', #12418, #324, #18269 ) ;
#17416 = DIRECTION ( 'NONE',  ( 0.01051738792036951628, 0.3656191332804069605, -0.9307051272721219570 ) ) ;
#17417 = DIRECTION ( 'NONE',  ( 0.000000000000000000, 0.000000000000000000, 1.000000000000000000 ) ) ;
#17418 = ORIENTED_EDGE ( 'NONE', *, *, #20550, .F. ) ;
#17419 = ORIENTED_EDGE ( 'NONE', *, *, #16483, .F. ) ;
#17420 = CARTESIAN_POINT ( 'NONE',  ( -678.9461782662789346, 75.00000000000000000, -29.99999999999836220 ) ) ;
#17421 = CARTESIAN_POINT ( 'NONE',  ( 167.0466155511619490, 9.710058186601976615, -23.44215416552584230 ) ) ;
#17422 = CARTESIAN_POINT ( 'NONE',  ( -89.92902785008706701, 8.088236460650101378, -20.44110050034134929 ) ) ;
#17423 = EDGE_CURVE ( 'NONE', #15298, #3201, #6341, .T. ) ;
#17424 = ORIENTED_EDGE ( 'NONE', *, *, #3710, .F. ) ;
#17425 = CARTESIAN_POINT ( 'NONE',  ( 199.9999999999999147, 0.6045081272180472531, 19.00173049909658474 ) ) ;
#17426 = CARTESIAN_POINT ( 'NONE',  ( -348.0000000000001137, -4.857225732735059864E-14, 0.000000000000000000 ) ) ;
#17427 = ADVANCED_FACE ( 'NONE', ( #14196, #12069, #8206, #18450, #20587, #24325 ), #6089, .F. ) ;
#17428 = CARTESIAN_POINT ( 'NONE',  ( 14.38125909742180397, 67.30136555895953165, 10.73282306403583242 ) ) ;
#17429 = CARTESIAN_POINT ( 'NONE',  ( -199.9999999999999432, 42.45148791631907415, -35.57044988732096868 ) ) ;
#17430 = CARTESIAN_POINT ( 'NONE',  ( -105.3755690713226727, 5.661656051307470077E-14, -21.75974354311649961 ) ) ;
#17431 = FACE_OUTER_BOUND ( 'NONE', #6697, .T. ) ;
#17432 = CARTESIAN_POINT ( 'NONE',  ( -77.90255099906853786, 8.644468104252323926, -20.04994828524279882 ) ) ;
#17433 = EDGE_CURVE ( 'NONE', #14785, #15268, #8072, .T. ) ;
#17434 = EDGE_CURVE ( 'NONE', #2322, #12353, #19390, .T. ) ;
#17435 = DIRECTION ( 'NONE',  ( 0.000000000000000000, 1.000000000000000000, 0.000000000000000000 ) ) ;
#17436 = VECTOR ( 'NONE', #23680, 1000.000000000000000 ) ;
#17437 = CARTESIAN_POINT ( 'NONE',  ( -135.8532207217289738, -40.00000000000014211, 9.153146818113153671 ) ) ;
#17438 = CARTESIAN_POINT ( 'NONE',  ( -91.56559293963836410, 40.00000000000019185, -17.32597176626768487 ) ) ;
#17439 = CARTESIAN_POINT ( 'NONE',  ( 170.2234770963711128, 17.36149277827004411, -17.36149277826983095 ) ) ;
#17440 = CARTESIAN_POINT ( 'NONE',  ( -192.9588430854689989, -8.596193650988133061E-14, 14.46834944099969533 ) ) ;
#17441 = CARTESIAN_POINT ( 'NONE',  ( -198.9234529670043798, 24.80620787431004004, 44.84148137681157209 ) ) ;
#17442 = CARTESIAN_POINT ( 'NONE',  ( 137.0939645874030930, 30.33050608226186995, 12.56330697291266318 ) ) ;
#17443 = CARTESIAN_POINT ( 'NONE',  ( -77.55640685876515761, -15.64922766773196905, -15.64922766773223195 ) ) ;
#17444 = CARTESIAN_POINT ( 'NONE',  ( 0.2972598230769976091, -10.13633138497479180, 10.13633138497468522 ) ) ;
#17445 = CARTESIAN_POINT ( 'NONE',  ( -77.79216379506679857, 20.86722748066878097, -6.767643439074305434 ) ) ;
#17446 = CARTESIAN_POINT ( 'NONE',  ( 192.4448373802101173, -42.42640687122073473, 14.14213562370301780 ) ) ;
#17447 = CARTESIAN_POINT ( 'NONE',  ( 170.2234770963711128, -10.92277846919187034, -10.92277846919209594 ) ) ;
#17448 = CARTESIAN_POINT ( 'NONE',  ( -654.5133026298142340, 39.46589736862178199, -21.64282600963380432 ) ) ;
#17449 = CARTESIAN_POINT ( 'NONE',  ( 0.4289717129526279260, 24.25042218720268750, 44.08776571100843711 ) ) ;
#17450 = VERTEX_POINT ( 'NONE', #16324 ) ;
#17451 = CARTESIAN_POINT ( 'NONE',  ( 199.9999999999999432, 14.14213562373110911, -14.14213562373072364 ) ) ;
#17452 = CARTESIAN_POINT ( 'NONE',  ( 163.1118516004056573, 27.26290988616875310, 0.000000000000000000 ) ) ;
#17453 = CARTESIAN_POINT ( 'NONE',  ( -188.2995950289364089, -13.82811170417104840, -46.99046209955525200 ) ) ;
#17454 = ORIENTED_EDGE ( 'NONE', *, *, #17746, .T. ) ;
#17455 = CARTESIAN_POINT ( 'NONE',  ( 184.8905102610680444, -40.00000000000021316, 20.92133201514402430 ) ) ;
#17456 = CARTESIAN_POINT ( 'NONE',  ( 199.0248560840425682, -19.46388604182612880, 4.665080622506349251 ) ) ;
#17457 = CARTESIAN_POINT ( 'NONE',  ( -77.90255099906772784, 8.644468104261493480, 20.04994828523958361 ) ) ;
#17458 = VERTEX_POINT ( 'NONE', #24045 ) ;
#17459 = VERTEX_POINT ( 'NONE', #5822 ) ;
#17460 = CIRCLE ( 'NONE', #22146, 69.99999999999998579 ) ;
#17461 = CARTESIAN_POINT ( 'NONE',  ( -135.8532207217289738, -21.81201906317758343, -34.75652343174620995 ) ) ;
#17462 = CARTESIAN_POINT ( 'NONE',  ( 91.82158438592158234, -6.516925787240506436E-14, 22.79471317813470321 ) ) ;
#17463 = DIRECTION ( 'NONE',  ( 0.000000000000000000, 0.000000000000000000, -1.000000000000000000 ) ) ;
#17464 = CARTESIAN_POINT ( 'NONE',  ( 0.2972598230769959993, 38.42060263243713081, -38.42060263243619289 ) ) ;
#17465 = CARTESIAN_POINT ( 'NONE',  ( -56.48582580120558561, -1.205267837095813407E-13, 30.84685318188644132 ) ) ;
#17466 = CARTESIAN_POINT ( 'NONE',  ( 199.9999999999999432, -6.993216068016765874, -17.67234381275832433 ) ) ;
#17467 = AXIS2_PLACEMENT_3D ( 'NONE', #12449, #5574, #20077 ) ;
#17468 = CARTESIAN_POINT ( 'NONE',  ( -77.55640685876515761, 15.64922766773205254, 15.64922766773212182 ) ) ;
#17469 = CARTESIAN_POINT ( 'NONE',  ( 4.995406935893289102, 10.78321810389013002, -10.78321810388986712 ) ) ;
#17470 = CARTESIAN_POINT ( 'NONE',  ( 14.38125909742180752, 17.55144818341503665, -39.01709431150898411 ) ) ;
#17471 = CARTESIAN_POINT ( 'NONE',  ( -105.3175882261758147, -20.76660717853137683, 5.408274864390659076 ) ) ;
#17472 = CARTESIAN_POINT ( 'NONE',  ( -213.1075012329537230, 5.259461644596141978E-13, -53.71589010951915100 ) ) ;
#17473 = FACE_OUTER_BOUND ( 'NONE', #15389, .T. ) ;
#17474 = CARTESIAN_POINT ( 'NONE',  ( 0.2972598230769983307, -14.33493731733933352, 0.000000000000000000 ) ) ;
#17475 = CARTESIAN_POINT ( 'NONE',  ( 170.2234770963711128, -15.44714144992812699, -40.00000000000002132 ) ) ;
#17476 = CARTESIAN_POINT ( 'NONE',  ( 146.6084372240433709, 24.48358557860311180, 32.08495691632071356 ) ) ;
#17477 = CARTESIAN_POINT ( 'NONE',  ( -198.0356074513804572, -55.37879056871328487, -40.00000000000002132 ) ) ;
#17479 = CARTESIAN_POINT ( 'NONE',  ( -109.1264249741438448, 13.72187187124579211, 33.12752917268907993 ) ) ;
#17478 = CARTESIAN_POINT ( 'NONE',  ( 130.8568914410475372, -24.07718906447255947, 24.07718906447199458 ) ) ;
#17480 = CARTESIAN_POINT ( 'NONE',  ( -100.7734535825088358, -2.560096224687585342E-13, 22.67402823373191723 ) ) ;
#17481 = CARTESIAN_POINT ( 'NONE',  ( 136.1360204305621551, -24.77266263493126885, 31.79587985999256006 ) ) ;
#17482 = CARTESIAN_POINT ( 'NONE',  ( 0.2972598230769930017, 54.33493731733938148, -40.00000000000002132 ) ) ;
#17483 = ORIENTED_EDGE ( 'NONE', *, *, #15149, .F. ) ;
#17484 = CARTESIAN_POINT ( 'NONE',  ( 23.35901252181239229, -46.81387818480112628, 13.80180065670254663 ) ) ;
#17485 = VECTOR ( 'NONE', #18477, 1000.000000000000000 ) ;
#17486 = CARTESIAN_POINT ( 'NONE',  ( -190.0000000000000000, 71.50000000000009948, -66.50000000000005684 ) ) ;
#17487 = CARTESIAN_POINT ( 'NONE',  ( -135.8532207217289738, 21.81201906317767936, 21.81201906317778239 ) ) ;
#17488 = DIRECTION ( 'NONE',  ( -1.000000000000000000, 1.836970198721030181E-16, 0.000000000000000000 ) ) ;
#17489 = CARTESIAN_POINT ( 'NONE',  ( -77.55380018288633437, 22.14554968447874472, -1.229295861724395866 ) ) ;
#17490 = CARTESIAN_POINT ( 'NONE',  ( -7.297127544328012583, 13.59739983758589865, -45.86058602274966489 ) ) ;
#17491 = CARTESIAN_POINT ( 'NONE',  ( 199.9999999999997726, -8.411091645968788555, 17.05096182211362432 ) ) ;
#17492 = EDGE_CURVE ( 'NONE', #14740, #24783, #24452, .T. ) ;
#17493 = LINE ( 'NONE', #24258, #21941 ) ;
#17494 = CARTESIAN_POINT ( 'NONE',  ( -77.67315633212632520, -4.804802313621894250, -21.50043107020669098 ) ) ;
#17495 = CARTESIAN_POINT ( 'NONE',  ( 146.6084372240433993, -24.48358557860353457, 24.48358557860296258 ) ) ;
#17496 = CARTESIAN_POINT ( 'NONE',  ( -56.48582580120558561, 6.472252184284607246, -50.09629031063960269 ) ) ;
#17497 = CARTESIAN_POINT ( 'NONE',  ( -200.0000000000000000, 71.50000000000009948, 66.50000000000005684 ) ) ;
#17498 = DIRECTION ( 'NONE',  ( 0.000000000000000000, 0.7071067811865443531, 0.7071067811865507924 ) ) ;
#17499 = CARTESIAN_POINT ( 'NONE',  ( 19.06497207195982568, -38.31983398719592770, -38.31983398719660272 ) ) ;
#17500 = AXIS2_PLACEMENT_3D ( 'NONE', #5487, #23339, #13221 ) ;
#17502 = CARTESIAN_POINT ( 'NONE',  ( -105.3755690713226585, -43.67073346367964604, -12.89780903124457545 ) ) ;
#17501 = CARTESIAN_POINT ( 'NONE',  ( 91.82158438592156813, 40.45024623143973486, -16.11829626348390931 ) ) ;
#17503 = CARTESIAN_POINT ( 'NONE',  ( 170.2234770963711128, 39.20704971665372796, 17.36149277827039583 ) ) ;
#17504 = DIRECTION ( 'NONE',  ( 1.000000000000000000, 1.836970198721030181E-16, 0.000000000000000000 ) ) ;
#17505 = CARTESIAN_POINT ( 'NONE',  ( 199.9999999999999432, -14.14213562373096345, -14.14213562373104871 ) ) ;
#17506 = DIRECTION ( 'NONE',  ( 0.000000000000000000, 1.000000000000000000, 0.000000000000000000 ) ) ;
#17507 = CARTESIAN_POINT ( 'NONE',  ( -238.4067589809705794, -0.6820004457913585449, -0.6820004457913265705 ) ) ;
#17508 = CARTESIAN_POINT ( 'NONE',  ( -105.3755690713226585, 18.24025645688349684, 40.00000000000002132 ) ) ;
#17510 = EDGE_CURVE ( 'NONE', #11213, #23831, #10897, .T. ) ;
#17509 = VERTEX_POINT ( 'NONE', #12331 ) ;
#17511 = CARTESIAN_POINT ( 'NONE',  ( 4.995406935893283773, 39.06748935135195211, -17.50105314357185193 ) ) ;
#17512 = CARTESIAN_POINT ( 'NONE',  ( 26.79002001241197561, 41.25333065883494044, 17.08768905195128340 ) ) ;
#17513 = CARTESIAN_POINT ( 'NONE',  ( 83.06440094970915311, 10.91839312111565263, 23.65491511366958832 ) ) ;
#17514 = CARTESIAN_POINT ( 'NONE',  ( -4.660840668352645544, -42.82207049670927290, -23.32816686155640440 ) ) ;
#17515 = EDGE_CURVE ( 'NONE', #13098, #19453, #2636, .T. ) ;
#17516 = ORIENTED_EDGE ( 'NONE', *, *, #18047, .T. ) ;
#17517 = CARTESIAN_POINT ( 'NONE',  ( -188.8948201289225608, -43.30398576617490392, 17.93709820916094699 ) ) ;
#17518 = CARTESIAN_POINT ( 'NONE',  ( 200.0000000000000568, 2.630809070280605511, -18.81871160794394982 ) ) ;
#17519 = CARTESIAN_POINT ( 'NONE',  ( 22.79879570922440024, -17.88067497375698522, 43.16776802602890228 ) ) ;
#17520 = EDGE_CURVE ( 'NONE', #2033, #20449, #16262, .T. ) ;
#17521 = CARTESIAN_POINT ( 'NONE',  ( 36.88256715627346694, 16.19941669821687569, -39.10885149560213847 ) ) ;
#17522 = CARTESIAN_POINT ( 'NONE',  ( 199.0070875033960078, 19.58406838943379569, -4.039067077891903779 ) ) ;
#17523 = CARTESIAN_POINT ( 'NONE',  ( -97.72675010090307524, -20.56394680065911729, -8.987772175319559409 ) ) ;
#17524 = CARTESIAN_POINT ( 'NONE',  ( 151.7948205124836534, 40.00000000000017053, -33.23291073765538783 ) ) ;
#17525 = CARTESIAN_POINT ( 'NONE',  ( -77.90255099906771363, -8.064892378658779393, 20.29001641120648003 ) ) ;
#17526 = CYLINDRICAL_SURFACE ( 'NONE', #13815, 29.99999999999999645 ) ;
#17527 = CARTESIAN_POINT ( 'NONE',  ( 151.7948205124836534, -6.767089262349006873, 40.00000000000002132 ) ) ;
#17529 = DIRECTION ( 'NONE',  ( 1.000000000000000000, 1.836970198721030181E-16, -0.000000000000000000 ) ) ;
#17528 = CARTESIAN_POINT ( 'NONE',  ( 199.0053211804427633, 14.13331159297750617, -14.14343255912447361 ) ) ;
#17530 = CARTESIAN_POINT ( 'NONE',  ( 19.06497207195982924, -54.19242893257843008, 40.00000000000002132 ) ) ;
#17531 = CARTESIAN_POINT ( 'NONE',  ( -280.0000000000000000, 19.99999999999996092, -0.000000000000000000 ) ) ;
#17532 = CARTESIAN_POINT ( 'NONE',  ( 91.82158438592158234, -17.20528682183298486, 0.000000000000000000 ) ) ;
#17533 = CARTESIAN_POINT ( 'NONE',  ( 91.82158438592156813, 39.99999999999986500, 17.20528682183341473 ) ) ;
#17534 = CARTESIAN_POINT ( 'NONE',  ( -86.96347745069643054, -39.99999999999985079, -18.24025645688394448 ) ) ;
#17535 = CARTESIAN_POINT ( 'NONE',  ( 146.5085219967539842, -29.94471555035083199, -12.40350730235989829 ) ) ;
#17536 = ORIENTED_EDGE ( 'NONE', *, *, #3266, .F. ) ;
#17538 = CARTESIAN_POINT ( 'NONE',  ( -1.087763065927251471, 43.78960619332519855, -24.03018639662559508 ) ) ;
#17537 = DIRECTION ( 'NONE',  ( -1.000000000000000000, 0.000000000000000000, 0.000000000000000000 ) ) ;
#17539 = CARTESIAN_POINT ( 'NONE',  ( -86.96347745069643054, -18.24025645688353947, 40.00000000000002132 ) ) ;
#17540 = CARTESIAN_POINT ( 'NONE',  ( -91.56559293963834989, -16.03295912088728414, 16.03295912088688269 ) ) ;
#17541 = CARTESIAN_POINT ( 'NONE',  ( -190.7345856381636793, 43.65254615102346492, -23.92884448221996152 ) ) ;
#17542 = DIRECTION ( 'NONE',  ( -1.000000000000000000, 0.000000000000000000, 0.000000000000000000 ) ) ;
#17543 = ORIENTED_EDGE ( 'NONE', *, *, #1337, .F. ) ;
#17544 = ORIENTED_EDGE ( 'NONE', *, *, #4556, .T. ) ;
#17545 = DIRECTION ( 'NONE',  ( 0.000000000000000000, 0.000000000000000000, 1.000000000000000000 ) ) ;
#17546 = CARTESIAN_POINT ( 'NONE',  ( 149.5797498300189545, 12.18602109748342777, -29.41965740490875802 ) ) ;
#17547 = ORIENTED_EDGE ( 'NONE', *, *, #11999, .F. ) ;
#17548 = VERTEX_POINT ( 'NONE', #22719 ) ;
#17549 = EDGE_LOOP ( 'NONE', ( #24868, #11788, #6143, #21648 ) ) ;
#17550 = CARTESIAN_POINT ( 'NONE',  ( 200.0000000000000568, -6.707298731100607370, 17.79007541258576452 ) ) ;
#17551 = DIRECTION ( 'NONE',  ( -1.000000000000000000, -0.000000000000000000, -0.000000000000000000 ) ) ;
#17552 = CARTESIAN_POINT ( 'NONE',  ( 151.7948205124836534, 33.06932595376365924, -23.49921654116018743 ) ) ;
#17553 = CARTESIAN_POINT ( 'NONE',  ( -199.9999999999999716, 35.57044988732193502, -42.45148791632000496 ) ) ;
#17554 = CARTESIAN_POINT ( 'NONE',  ( -238.4067589809705794, -4.716212492215116094E-14, 0.9644942799825824142 ) ) ;
#17555 = CARTESIAN_POINT ( 'NONE',  ( 23.37394308801977871, -13.80096434448300613, 46.80823611210190904 ) ) ;
#17556 = CARTESIAN_POINT ( 'NONE',  ( -626.9846540392142060, 75.00000000000000000, 0.000000000000000000 ) ) ;
#17557 = CARTESIAN_POINT ( 'NONE',  ( -238.4067589809705794, -4.716212492215116094E-14, 0.9644942799825824142 ) ) ;
#17558 = CARTESIAN_POINT ( 'NONE',  ( -53.37717264285771535, -29.42738956023914199, -10.11115224722892769 ) ) ;
#17559 = CARTESIAN_POINT ( 'NONE',  ( -213.1075012329537230, -39.99999999999948841, -53.71589010950208376 ) ) ;
#17560 = CARTESIAN_POINT ( 'NONE',  ( -114.5444905533725262, -9.939131763645404405, 19.55376799570613500 ) ) ;
#17561 = CARTESIAN_POINT ( 'NONE',  ( 146.6084372240433993, 24.48358557860341733, -24.48358557860313311 ) ) ;
#17562 = CARTESIAN_POINT ( 'NONE',  ( -259.2033419157646676, -1.438356298054549103E-14, -9.517827891722632216 ) ) ;
#17563 = CARTESIAN_POINT ( 'NONE',  ( 146.6084372240433993, 24.48358557860341733, -24.48358557860313311 ) ) ;
#17564 = CARTESIAN_POINT ( 'NONE',  ( 153.3020327024398171, 28.42252382389414933, 11.77299484472951541 ) ) ;
#17565 = ADVANCED_FACE ( 'NONE', ( #4496 ), #15120, .F. ) ;
#17566 = CARTESIAN_POINT ( 'NONE',  ( 190.0000000000000000, 66.50000000000009948, -66.50000000000005684 ) ) ;
#17567 = CARTESIAN_POINT ( 'NONE',  ( 19.06497207195981147, -10.03556273973439517, 10.03556273973429214 ) ) ;
#17568 = CARTESIAN_POINT ( 'NONE',  ( 0.2972598230769957217, -4.999556039334937811E-14, 14.33493731733933352 ) ) ;
#17569 = CARTESIAN_POINT ( 'NONE',  ( -100.7734535825088500, -16.03295912088716335, 40.53558337403673306 ) ) ;
#17570 = CARTESIAN_POINT ( 'NONE',  ( 91.82158438592159655, -44.40256751092341858, 12.16597498400012434 ) ) ;
#17571 = CARTESIAN_POINT ( 'NONE',  ( -129.2303573020097645, -11.67678754046080591, -24.84170325987118133 ) ) ;
#17572 = CARTESIAN_POINT ( 'NONE',  ( 170.0000000000000853, 9.369682556672316309, -22.62041470344884075 ) ) ;
#17573 = ORIENTED_EDGE ( 'NONE', *, *, #18926, .T. ) ;
#17574 = CARTESIAN_POINT ( 'NONE',  ( 0.2972598230769959993, 38.42060263243713081, -38.42060263243619289 ) ) ;
#17575 = DIRECTION ( 'NONE',  ( 0.000000000000000000, -1.000000000000000000, 0.000000000000000000 ) ) ;
#17576 = CARTESIAN_POINT ( 'NONE',  ( 180.0000000000000000, -66.50000000000001421, 66.50000000000005684 ) ) ;
#17577 = ORIENTED_EDGE ( 'NONE', *, *, #21527, .T. ) ;
#17578 = CARTESIAN_POINT ( 'NONE',  ( 19.06497207195981858, -39.99999999999987210, -14.19242893257882621 ) ) ;
#17579 = EDGE_CURVE ( 'NONE', #14912, #3577, #2396, .T. ) ;
#17580 = CARTESIAN_POINT ( 'NONE',  ( 199.0250265424592726, -19.30222243252582714, 5.292048582057746309 ) ) ;
#17581 = CARTESIAN_POINT ( 'NONE',  ( -47.50817905881373804, 12.56548180736879772, 30.33575659748668940 ) ) ;
#17582 = ORIENTED_EDGE ( 'NONE', *, *, #24937, .T. ) ;
#17583 = ORIENTED_EDGE ( 'NONE', *, *, #7406, .T. ) ;
#17584 = CARTESIAN_POINT ( 'NONE',  ( 170.2234770963711128, 17.36149277827004411, -17.36149277826983095 ) ) ;
#17585 = CARTESIAN_POINT ( 'NONE',  ( 136.1360204305621266, 5.219216885335291329E-15, 4.966164525587064560 ) ) ;
#17586 = CARTESIAN_POINT ( 'NONE',  ( -88.37877758187804034, -20.15391234954027055, -8.026456973411162821 ) ) ;
#17587 = CARTESIAN_POINT ( 'NONE',  ( -91.56559293963834989, 12.25131212657497848, -12.25131212657469426 ) ) ;
#17588 = CARTESIAN_POINT ( 'NONE',  ( 14.38125909742181818, -1.924622159709266762E-13, 55.17850393972636880 ) ) ;
#17589 = CARTESIAN_POINT ( 'NONE',  ( 199.9999999999998295, -18.94756416210704941, 1.560766781390804381 ) ) ;
#17590 = CARTESIAN_POINT ( 'NONE',  ( -259.2033419157646676, -1.438356298054549103E-14, -9.517827891722632216 ) ) ;
#17591 = FACE_BOUND ( 'NONE', #22485, .T. ) ;
#17592 = CARTESIAN_POINT ( 'NONE',  ( -4.580761711675023662, -17.81010960708106339, -42.99740816077124350 ) ) ;
#17593 = CARTESIAN_POINT ( 'NONE',  ( 192.4448373802101173, 42.42640687122089815, -14.14213562370272470 ) ) ;
#17594 = PRODUCT_DEFINITION ( 'UNKNOWN', '', #12568, #1121 ) ;
#17595 = CARTESIAN_POINT ( 'NONE',  ( -199.9999999999998579, 44.86878812508723513, -24.82633483071237634 ) ) ;
#17596 = CARTESIAN_POINT ( 'NONE',  ( -91.56559293963834989, -2.543181659092656077E-13, 22.67402823373191723 ) ) ;
#17597 = CARTESIAN_POINT ( 'NONE',  ( 85.88498456118406921, 8.769910164384999263, 23.37206003906720397 ) ) ;
#17598 = CARTESIAN_POINT ( 'NONE',  ( -238.4067589809705794, -0.9644942799826262680, 0.000000000000000000 ) ) ;
#17599 = CARTESIAN_POINT ( 'NONE',  ( -30.26275506840323004, -41.69427246844627888, -40.00000000000002132 ) ) ;
#17600 = CARTESIAN_POINT ( 'NONE',  ( -280.0000000000000568, 42.42640687119274645, 14.14213562373118194 ) ) ;
#17601 = CARTESIAN_POINT ( 'NONE',  ( 4.995406935893294431, -15.24977328854832415, -40.00000000000002132 ) ) ;
#17603 = CARTESIAN_POINT ( 'NONE',  ( -86.95492397413735830, -9.645500094587582396, -19.11844798802007617 ) ) ;
#17602 = CARTESIAN_POINT ( 'NONE',  ( 22.68416413276407795, -43.06288726621011875, -23.49220544186193038 ) ) ;
#17604 = CARTESIAN_POINT ( 'NONE',  ( -91.56559293963834989, -2.543181659092656077E-13, 22.67402823373191723 ) ) ;
#17605 = CARTESIAN_POINT ( 'NONE',  ( -86.96347745069644475, 12.89780903124401057, 12.89780903124407629 ) ) ;
#17606 = EDGE_CURVE ( 'NONE', #4564, #10703, #24490, .T. ) ;
#17607 = CARTESIAN_POINT ( 'NONE',  ( -135.8532207217289738, 30.84685318188643066, 2.449293598294708485E-15 ) ) ;
#17608 = ORIENTED_EDGE ( 'NONE', *, *, #19953, .F. ) ;
#17609 = CARTESIAN_POINT ( 'NONE',  ( 23.35901252181232479, -42.86175755505330898, 23.34306388117434139 ) ) ;
#17610 = CARTESIAN_POINT ( 'NONE',  ( -77.90255099906767100, -8.064892378658175431, 20.29001641120675004 ) ) ;
#17611 = CARTESIAN_POINT ( 'NONE',  ( 200.0000000000000000, -14.14213562373106114, 42.42640687119278908 ) ) ;
#17612 = CARTESIAN_POINT ( 'NONE',  ( -30.26275506840324070, -40.00000000000003553, 1.694272468446120117 ) ) ;
#17613 = CARTESIAN_POINT ( 'NONE',  ( 0.2972598230769938343, 10.13633138497486286, -10.13633138497461594 ) ) ;
#17614 = CARTESIAN_POINT ( 'NONE',  ( 19.06497207195980792, 14.19242893257840699, -40.00000000000002132 ) ) ;
#17615 = CARTESIAN_POINT ( 'NONE',  ( -114.4364955367327497, -20.04994829327637262, -8.644468109209869411 ) ) ;
#17616 = CARTESIAN_POINT ( 'NONE',  ( 199.9999999999998010, -6.124229907523811356, 17.99904841416608292 ) ) ;
#17617 = CARTESIAN_POINT ( 'NONE',  ( -77.70933353446504555, -5.475739710260814519, -21.30703284266700592 ) ) ;
#17618 = CARTESIAN_POINT ( 'NONE',  ( -208.1127848780265026, 10.60833733269551615, -10.60833733269529766 ) ) ;
#17619 = CARTESIAN_POINT ( 'NONE',  ( -208.1127848780264742, -38.89260858015704514, -38.89260858015768463 ) ) ;
#17620 =( GEOMETRIC_REPRESENTATION_CONTEXT ( 3 ) GLOBAL_UNCERTAINTY_ASSIGNED_CONTEXT ( ( #11221 ) ) GLOBAL_UNIT_ASSIGNED_CONTEXT ( ( #25985, #24513, #13985 ) ) REPRESENTATION_CONTEXT ( 'NONE', 'WORKASPACE' ) );
#17621 = CARTESIAN_POINT ( 'NONE',  ( -77.70103186979810062, -21.35019956121274731, -5.501793373024266742 ) ) ;
#17622 = CARTESIAN_POINT ( 'NONE',  ( -190.0000000000000000, -61.50000000000001421, 66.50000000000005684 ) ) ;
#17623 = CARTESIAN_POINT ( 'NONE',  ( -213.1075012329537230, -9.698598906462304825, -66.26714140138675191 ) ) ;
#17625 = CARTESIAN_POINT ( 'NONE',  ( 151.7948205124836534, -23.49921654115981084, -33.06932595376387951 ) ) ;
#17624 = CARTESIAN_POINT ( 'NONE',  ( -86.96347745069643054, 15.38646221621821297, -41.18208027870583265 ) ) ;
#17626 = CARTESIAN_POINT ( 'NONE',  ( -86.96347745069644475, -15.38646221621807442, 15.38646221621768184 ) ) ;
#17627 = CARTESIAN_POINT ( 'NONE',  ( 190.0000000000000000, -52.49999999999991473, 52.49999999999999289 ) ) ;
#17628 = DIRECTION ( 'NONE',  ( 1.000000000000000000, -1.937599346585394162E-16, -0.000000000000000000 ) ) ;
#17629 = CARTESIAN_POINT ( 'NONE',  ( -192.9588430854690273, -40.00000000000011369, 14.46834944099955855 ) ) ;
#17630 = AXIS2_PLACEMENT_3D ( 'NONE', #9505, #24142, #25754 ) ;
#17631 = CARTESIAN_POINT ( 'NONE',  ( 184.8905102610680444, 14.79361573936375507, 14.79361573936398067 ) ) ;
#17632 = AXIS2_PLACEMENT_3D ( 'NONE', #23988, #7747, #13876 ) ;
#17633 = CARTESIAN_POINT ( 'NONE',  ( 130.8568914410475088, -34.05028731879786363, 40.00000000000002132 ) ) ;
#17634 = ORIENTED_EDGE ( 'NONE', *, *, #23848, .T. ) ;
#17635 = CARTESIAN_POINT ( 'NONE',  ( -280.0000000000000000, -14.14213562373098831, -14.14213562373098654 ) ) ;
#17636 = FACE_OUTER_BOUND ( 'NONE', #24901, .T. ) ;
#17637 = CARTESIAN_POINT ( 'NONE',  ( 22.98934664983071841, 17.85845455616048483, 43.11412319250736402 ) ) ;
#17638 = CARTESIAN_POINT ( 'NONE',  ( 192.4448373802100889, -20.00000000003938538, 0.000000000000000000 ) ) ;
#17639 = ORIENTED_EDGE ( 'NONE', *, *, #24784, .T. ) ;
#17640 = CARTESIAN_POINT ( 'NONE',  ( -188.4701769959648061, -47.05181236278195911, 13.83721050407064190 ) ) ;
#17641 = AXIS2_PLACEMENT_3D ( 'NONE', #1644, #10283, #18392 ) ;
#17642 = MANIFOLD_SOLID_BREP ( 'Chamfer1', #14709 ) ;
#17643 = CARTESIAN_POINT ( 'NONE',  ( 199.9999999999998863, -15.98179559645994097, -10.29177186004950961 ) ) ;
#17644 = CARTESIAN_POINT ( 'NONE',  ( 67.78092418467272751, -12.11998378903902385, 29.26022923861282266 ) ) ;
#17645 = CARTESIAN_POINT ( 'NONE',  ( 13.28449813601589824, 14.15462405554525382, -49.16593779332317382 ) ) ;
#17646 = CARTESIAN_POINT ( 'NONE',  ( 199.0054653064281922, 16.25946365448332998, -11.63817148238572940 ) ) ;
#17647 = AXIS2_PLACEMENT_3D ( 'NONE', #481, #16567, #19098 ) ;
#17648 = CYLINDRICAL_SURFACE ( 'NONE', #4533, 5.000000000000046185 ) ;
#17649 = CARTESIAN_POINT ( 'NONE',  ( 0.2972598230769956662, 39.99999999999983658, 54.33493731733950938 ) ) ;
#17650 = CARTESIAN_POINT ( 'NONE',  ( -100.7734535825088358, 6.065416334915073333E-14, -22.67402823373191723 ) ) ;
#17651 = CARTESIAN_POINT ( 'NONE',  ( -210.0000000000000284, -52.49999999999991473, 52.49999999999999289 ) ) ;
#17652 = CARTESIAN_POINT ( 'NONE',  ( -208.1127848780264742, -55.00245453010926866, 40.00000000000002132 ) ) ;
#17654 = CARTESIAN_POINT ( 'NONE',  ( -600.4664386284592865, 37.45914613463217080, -14.03654238641473562 ) ) ;
#17653 = CARTESIAN_POINT ( 'NONE',  ( 67.79414719525901489, -14.15005687183196237, -28.72755866871360553 ) ) ;
#17655 = CARTESIAN_POINT ( 'NONE',  ( -100.7734535825088500, 22.67402823373189946, 40.00000000000002132 ) ) ;
#17657 = CARTESIAN_POINT ( 'NONE',  ( -238.4067589809705794, -40.96449427990185654, -40.00000000000002132 ) ) ;
#17656 = VECTOR ( 'NONE', #26058, 1000.000000000000000 ) ;
#17658 = CARTESIAN_POINT ( 'NONE',  ( 57.59792236341147031, -2.435789363418150000, 40.00000000000002132 ) ) ;
#17659 = CARTESIAN_POINT ( 'NONE',  ( 146.6084372240433709, 40.00000000000010658, -5.374981219216549810 ) ) ;
#17660 = CARTESIAN_POINT ( 'NONE',  ( -199.9999999999999432, 14.17215463606929227, 49.28189405767592746 ) ) ;
#17661 = CARTESIAN_POINT ( 'NONE',  ( -162.0762913951020892, -1.198031840385767266, -1.198031840385758384 ) ) ;
#17662 = ORIENTED_EDGE ( 'NONE', *, *, #8472, .T. ) ;
#17663 = CARTESIAN_POINT ( 'NONE',  ( -87.13361725327072804, 21.49321519333427233, -1.448021113139547951E-30 ) ) ;
#17664 = CARTESIAN_POINT ( 'NONE',  ( 200.0000000000000000, 20.00000000000013856, 40.00000000000002132 ) ) ;
#17665 = EDGE_CURVE ( 'NONE', #6802, #11453, #24177, .T. ) ;
#17666 = CARTESIAN_POINT ( 'NONE',  ( -188.5332420855723683, 47.07509783863601172, -13.84065984176399233 ) ) ;
#17667 = DIRECTION ( 'NONE',  ( 0.000000000000000000, 0.000000000000000000, 1.000000000000000000 ) ) ;
#17668 = VERTEX_POINT ( 'NONE', #10745 ) ;
#17669 = VERTEX_POINT ( 'NONE', #18856 ) ;
#17670 = AXIS2_PLACEMENT_3D ( 'NONE', #9699, #9835, #21946 ) ;
#17671 = CARTESIAN_POINT ( 'NONE',  ( -190.0000000000000284, -82.49999999999990052, 52.49999999999977973 ) ) ;
#17672 = CARTESIAN_POINT ( 'NONE',  ( -87.13361725327072804, 8.813415818526478339E-15, 21.49321519333429009 ) ) ;
#17673 = VERTEX_POINT ( 'NONE', #23251 ) ;
#17674 = CARTESIAN_POINT ( 'NONE',  ( -198.0356074513804572, 15.37879056873066830, -40.00000000000002132 ) ) ;
#17675 = CARTESIAN_POINT ( 'NONE',  ( -100.0968563617724527, -20.72609133247079427, 8.149320301504525688 ) ) ;
#17676 = ORIENTED_EDGE ( 'NONE', *, *, #9009, .T. ) ;
#17677 = CARTESIAN_POINT ( 'NONE',  ( 200.0000000000001421, -10.70065846580424207, 15.71346033962178446 ) ) ;
#17678 = CARTESIAN_POINT ( 'NONE',  ( -188.5332420855686166, 13.84065984174896435, 47.07509783864872333 ) ) ;
#17679 = AXIS2_PLACEMENT_3D ( 'NONE', #8875, #4495, #6873 ) ;
#17680 = CARTESIAN_POINT ( 'NONE',  ( -259.2033419157646676, 49.83842185052027673, -6.730120644403441155 ) ) ;
#17681 = CARTESIAN_POINT ( 'NONE',  ( -199.9999999999999432, 39.01096890182095223, -39.01096890182004273 ) ) ;
#17682 = CARTESIAN_POINT ( 'NONE',  ( 4.995406935893290878, -5.232665749138292703E-14, 15.24977328854832592 ) ) ;
#17683 = CARTESIAN_POINT ( 'NONE',  ( 4.990270234119178028, -14.15117691407206379, 49.14367003637716635 ) ) ;
#17684 = CARTESIAN_POINT ( 'NONE',  ( -83.21262154144253032, 13.72187187061549274, -33.12752917118393015 ) ) ;
#17685 = DIRECTION ( 'NONE',  ( 0.000000000000000000, -1.000000000000000000, 0.000000000000000000 ) ) ;
#17686 = FACE_OUTER_BOUND ( 'NONE', #19849, .T. ) ;
#17687 = CARTESIAN_POINT ( 'NONE',  ( 170.2234770963711128, -39.99999999999982947, -15.44714144992858529 ) ) ;
#17688 = CARTESIAN_POINT ( 'NONE',  ( -105.2053629887588500, -15.67233752939762503, 14.72427054407682157 ) ) ;
#17689 = CARTESIAN_POINT ( 'NONE',  ( 151.7948205124835681, -4.785054706298153882, -51.78348778862540058 ) ) ;
#17690 = CARTESIAN_POINT ( 'NONE',  ( -208.1127848780265026, -9.061048840815752106E-14, 15.00245453012669472 ) ) ;
#17691 = CARTESIAN_POINT ( 'NONE',  ( 57.59792236341148453, -54.84617931850877426, -1.722363176415331099 ) ) ;
#17692 = CARTESIAN_POINT ( 'NONE',  ( -99.29480781227083241, 8.165122821357551075, 20.80016781325174335 ) ) ;
#17693 = CARTESIAN_POINT ( 'NONE',  ( 98.29820294267528880, -14.14213562373450017, -14.14213562373441668 ) ) ;
#17694 = CARTESIAN_POINT ( 'NONE',  ( 0.2972598230769883387, 40.00000000000017053, -14.33493731733891607 ) ) ;
#17695 = CARTESIAN_POINT ( 'NONE',  ( -280.0000000000000568, -40.00000000000014211, 19.99999999999987210 ) ) ;
#17696 = CARTESIAN_POINT ( 'NONE',  ( -105.3755690713226585, -15.38646221621796251, 41.18208027870593924 ) ) ;
#17697 =( BOUNDED_CURVE ( )  B_SPLINE_CURVE ( 3, ( #20328, #2105, #22596, #12603 ),
 .UNSPECIFIED., .F., .F. ) 
 B_SPLINE_CURVE_WITH_KNOTS ( ( 4, 4 ),
 ( 0.01388163287021765106, 0.02359082919310009213 ),
 .UNSPECIFIED. ) 
 CURVE ( )  GEOMETRIC_REPRESENTATION_ITEM ( )  RATIONAL_B_SPLINE_CURVE ( ( 1.000000000000000000, 0.8672072324488967476, 0.7608653435686154598, 0.6809743333591562475 ) ) 
 REPRESENTATION_ITEM ( '' )  );
#17698 = CARTESIAN_POINT ( 'NONE',  ( -162.0762913951020607, -57.76657433537922515, -1.198031840455874963 ) ) ;
#17699 = CARTESIAN_POINT ( 'NONE',  ( -166.3490736461184838, -12.23457872956201697, -39.29841219602351288 ) ) ;
#17700 = CARTESIAN_POINT ( 'NONE',  ( 130.8568914410475372, 24.07718906447243867, -24.07718906447216156 ) ) ;
#17701 = VERTEX_POINT ( 'NONE', #504 ) ;
#17702 = CARTESIAN_POINT ( 'NONE',  ( 136.1360204305621551, 31.79587985999232558, 24.77266263493161702 ) ) ;
#17703 = DIRECTION ( 'NONE',  ( 1.000000000000000000, 1.836970198721030181E-16, 0.000000000000000000 ) ) ;
#17704 = CIRCLE ( 'NONE', #13872, 5.000000000000004441 ) ;
#17705 = CYLINDRICAL_SURFACE ( 'NONE', #2144, 5.000000000000007994 ) ;
#17706 = CARTESIAN_POINT ( 'NONE',  ( -192.9588430854690273, 10.23066800229588758, -66.79921049721882298 ) ) ;
#17707 = CARTESIAN_POINT ( 'NONE',  ( -99.21568817060988010, 22.67402823373189591, -0.000000000000000000 ) ) ;
#17708 = ORIENTED_EDGE ( 'NONE', *, *, #3969, .F. ) ;
#17709 = DIRECTION ( 'NONE',  ( 0.3301743754003874098, 0.000000000000000000, -0.9439199552022214945 ) ) ;
#17710 = CARTESIAN_POINT ( 'NONE',  ( 199.0159014060021150, -14.06460796087901954, -14.21930665748418576 ) ) ;
#17711 = CARTESIAN_POINT ( 'NONE',  ( -24.51100708734949052, 15.48921386281993051, 37.39427017793874342 ) ) ;
#17712 = VECTOR ( 'NONE', #6631, 1000.000000000000000 ) ;
#17713 = ORIENTED_EDGE ( 'NONE', *, *, #11594, .F. ) ;
#17714 = ORIENTED_EDGE ( 'NONE', *, *, #11104, .F. ) ;
#17715 = CARTESIAN_POINT ( 'NONE',  ( -280.0000000000000568, -20.00000000000006750, -40.00000000000002132 ) ) ;
#17716 = CARTESIAN_POINT ( 'NONE',  ( -194.4222169613648532, -44.35789444895097233, -24.44978956117715541 ) ) ;
#17717 = CARTESIAN_POINT ( 'NONE',  ( 184.8905102610680444, -3.509827109981123710E-14, 19.07866798485558490 ) ) ;
#17718 = PRESENTATION_STYLE_ASSIGNMENT (( #21995 ) ) ;
#17719 = CARTESIAN_POINT ( 'NONE',  ( -105.3755690713226727, 12.89780903124418998, -12.89780903124389155 ) ) ;
#17720 = DIRECTION ( 'NONE',  ( 0.3301743753925353575, 0.9439199552049681863, 0.000000000000000000 ) ) ;
#17721 = CARTESIAN_POINT ( 'NONE',  ( 14.38125909742182529, -40.00000000000021316, 55.17850393974251944 ) ) ;
#17722 = CARTESIAN_POINT ( 'NONE',  ( 199.9999999999999432, -17.61942792365240607, -7.131405496535110800 ) ) ;
#17723 = CARTESIAN_POINT ( 'NONE',  ( 14.38125909742181108, -5.035366881890652543E-14, 15.17850393972633682 ) ) ;
#17724 = FACE_OUTER_BOUND ( 'NONE', #20650, .T. ) ;
#17725 = CARTESIAN_POINT ( 'NONE',  ( 130.8568914410475372, -24.07718906447255947, 24.07718906447199458 ) ) ;
#17726 = CARTESIAN_POINT ( 'NONE',  ( -56.48582580120558561, 6.472252184284607246, -50.09629031063960269 ) ) ;
#17727 = CARTESIAN_POINT ( 'NONE',  ( 98.29820294267314296, 18.47759065023127079, 7.653668647304074923 ) ) ;
#17728 = APPLICATION_CONTEXT ( 'automotive_design' ) ;
#17729 = CARTESIAN_POINT ( 'NONE',  ( 14.38125909742181108, 1.616281842095393922E-13, -15.17850393972633682 ) ) ;
#17730 = CARTESIAN_POINT ( 'NONE',  ( -30.26275506840324425, -1.694272468446265334, 40.00000000000002132 ) ) ;
#17731 = CARTESIAN_POINT ( 'NONE',  ( 19.06497207195980792, -14.19242893257839988, -40.00000000000002132 ) ) ;
#17732 = CARTESIAN_POINT ( 'NONE',  ( 136.1360204305621266, 53.05693388239316022, 3.511608612530967566 ) ) ;
#17733 = CARTESIAN_POINT ( 'NONE',  ( -192.9588430854690273, -54.46834944101725284, -40.00000000000002132 ) ) ;
#17734 = DIRECTION ( 'NONE',  ( 0.000000000000000000, 0.000000000000000000, 1.000000000000000000 ) ) ;
#17735 = CARTESIAN_POINT ( 'NONE',  ( 0.2972598230769957217, 1.502051041545559470E-13, -14.33493731733933352 ) ) ;
#17736 = CARTESIAN_POINT ( 'NONE',  ( 57.59792236341147031, 54.84617931850881689, -1.722363176414946073 ) ) ;
#17737 = CARTESIAN_POINT ( 'NONE',  ( 199.9999999999999432, 19.99999999999996092, 2.449293598294708485E-15 ) ) ;
#17738 = ORIENTED_EDGE ( 'NONE', *, *, #7370, .F. ) ;
#17739 = CARTESIAN_POINT ( 'NONE',  ( 90.68848816910541188, -21.47805809224183449, 8.337973097871099526 ) ) ;
#17740 = CARTESIAN_POINT ( 'NONE',  ( 130.8888609958234497, 12.21841679119692792, 29.49786752803550627 ) ) ;
#17741 = ADVANCED_FACE ( 'NONE', ( #14988 ), #6742, .F. ) ;
#17742 =( BOUNDED_SURFACE ( )  B_SPLINE_SURFACE ( 3, 3, ( 
 ( #21467, #21224, #19341, #18961, #999, #23348, #23472, #13348, #24962, #10981, #1131, #19091, #9235, #871, #742, #14960, #8846, #15218, #7228, #8979, #22954, #15086, #16955, #2739, #25093, #17087, #2997, #11101, #25349, #25219 ),
 ( #23095, #3121, #11225, #1252, #6972, #7106, #4866, #19465, #5243, #6840, #3245, #4998, #9356, #19218, #9102, #6708, #17343, #14822, #17211, #5125, #4732, #25479, #12842, #20958, #13229, #12239, #9617, #10114, #14366, #16091 ),
 ( #20363, #13475, #22230, #5497, #7351, #24492, #18214, #2267, #4276, #14101, #15591, #15464, #24221, #25726, #3368, #8240, #23716, #17721, #5370, #2137, #12365, #23591, #21597, #6253, #20494, #26353, #24358, #13597, #3503, #5994 ),
 ( #11469, #16358, #4006, #1383, #19595, #10247, #8111, #16228, #22497, #11601, #25608, #1510, #18357, #17465, #9484, #7478, #12105, #17588, #4146, #21727, #19724, #25862, #7973, #20230, #2009, #6122, #14230, #22370, #136, #12903 ),
 ( #8375, #10375, #18486, #2530, #24887, #12633, #8509, #14887, #23027, #13037, #18757, #18889, #16626, #4926, #803, #10509, #25154, #4536, #21155, #10647, #20760, #6905, #4802, #23152, #22627, #20623, #267, #21019, #17018, #2802 ),
 ( #8777, #24757, #15022, #16497, #19024, #14496, #10913, #6377, #16890, #4402, #22886, #25022, #14621, #22758, #24622, #539, #14756, #8644, #406, #668, #16753, #8908, #12496, #6642, #4665, #12767, #20894, #2398, #6510, #2671 ),
 ( #18623, #10776, #6775, #9042, #19655, #19406, #17147, #25410, #15152, #9418, #17650, #1441, #5432, #7035, #11038, #933, #2929, #19148, #21407, #17399, #5183, #1058, #7409, #15523, #5555, #11286, #11403, #9164, #23777, #9542 ) ),
 .UNSPECIFIED., .T., .F., .F. ) 
 B_SPLINE_SURFACE_WITH_KNOTS ( ( 4, 3, 4 ),
 ( 4, 2, 2, 2, 2, 2, 2, 2, 2, 2, 2, 2, 2, 2, 4 ),
 ( 0.000000000000000000, 0.5000000000000000000, 1.000000000000000000 ),
 ( 0.000000000000000000, 0.1357259735107005372, 0.1651108541090157700, 0.1944957347073310028, 0.3598804999793158710, 0.3867117631979620773, 0.4135430264166082281, 0.5789277916885930964, 0.6062785021374117456, 0.6336292125862302838, 0.8508620842112317728, 0.8814014469398914198, 0.9119408096685510667, 0.9559704048342755334, 1.000000000000000000 ),
 .UNSPECIFIED. ) 
 GEOMETRIC_REPRESENTATION_ITEM ( )  RATIONAL_B_SPLINE_SURFACE ( (
 ( 1.000000000000000000, 1.000000000000000000, 1.000000000000000000, 1.000000000000000000, 1.000000000000000000, 1.000000000000000000, 1.000000000000000000, 1.000000000000000000, 1.000000000000000000, 1.000000000000000000, 1.000000000000000000, 1.000000000000000000, 1.000000000000000000, 1.000000000000000000, 1.000000000000000000, 1.000000000000000000, 1.000000000000000000, 1.000000000000000000, 1.000000000000000000, 1.000000000000000000, 1.000000000000000000, 1.000000000000000000, 1.000000000000000000, 1.000000000000000000, 1.000000000000000000, 1.000000000000000000, 1.000000000000000000, 1.000000000000000000, 1.000000000000000000, 1.000000000000000000),
 ( 0.3333333333333333703, 0.3333333333333333703, 0.3333333333333333703, 0.3333333333333333703, 0.3333333333333333703, 0.3333333333333333703, 0.3333333333333333703, 0.3333333333333333703, 0.3333333333333333703, 0.3333333333333333703, 0.3333333333333333703, 0.3333333333333333703, 0.3333333333333333703, 0.3333333333333333703, 0.3333333333333333703, 0.3333333333333333703, 0.3333333333333333703, 0.3333333333333333703, 0.3333333333333333703, 0.3333333333333333703, 0.3333333333333333703, 0.3333333333333333703, 0.3333333333333333703, 0.3333333333333333703, 0.3333333333333333703, 0.3333333333333333703, 0.3333333333333333703, 0.3333333333333333703, 0.3333333333333333703, 0.3333333333333333703),
 ( 0.3333333333333333703, 0.3333333333333333703, 0.3333333333333333703, 0.3333333333333333703, 0.3333333333333333703, 0.3333333333333333703, 0.3333333333333333703, 0.3333333333333333703, 0.3333333333333333703, 0.3333333333333333703, 0.3333333333333333703, 0.3333333333333333703, 0.3333333333333333703, 0.3333333333333333703, 0.3333333333333333703, 0.3333333333333333703, 0.3333333333333333703, 0.3333333333333333703, 0.3333333333333333703, 0.3333333333333333703, 0.3333333333333333703, 0.3333333333333333703, 0.3333333333333333703, 0.3333333333333333703, 0.3333333333333333703, 0.3333333333333333703, 0.3333333333333333703, 0.3333333333333333703, 0.3333333333333333703, 0.3333333333333333703),
 ( 1.000000000000000000, 1.000000000000000000, 1.000000000000000000, 1.000000000000000000, 1.000000000000000000, 1.000000000000000000, 1.000000000000000000, 1.000000000000000000, 1.000000000000000000, 1.000000000000000000, 1.000000000000000000, 1.000000000000000000, 1.000000000000000000, 1.000000000000000000, 1.000000000000000000, 1.000000000000000000, 1.000000000000000000, 1.000000000000000000, 1.000000000000000000, 1.000000000000000000, 1.000000000000000000, 1.000000000000000000, 1.000000000000000000, 1.000000000000000000, 1.000000000000000000, 1.000000000000000000, 1.000000000000000000, 1.000000000000000000, 1.000000000000000000, 1.000000000000000000),
 ( 0.3333333333333333703, 0.3333333333333333703, 0.3333333333333333703, 0.3333333333333333703, 0.3333333333333333703, 0.3333333333333333703, 0.3333333333333333703, 0.3333333333333333703, 0.3333333333333333703, 0.3333333333333333703, 0.3333333333333333703, 0.3333333333333333703, 0.3333333333333333703, 0.3333333333333333703, 0.3333333333333333703, 0.3333333333333333703, 0.3333333333333333703, 0.3333333333333333703, 0.3333333333333333703, 0.3333333333333333703, 0.3333333333333333703, 0.3333333333333333703, 0.3333333333333333703, 0.3333333333333333703, 0.3333333333333333703, 0.3333333333333333703, 0.3333333333333333703, 0.3333333333333333703, 0.3333333333333333703, 0.3333333333333333703),
 ( 0.3333333333333333703, 0.3333333333333333703, 0.3333333333333333703, 0.3333333333333333703, 0.3333333333333333703, 0.3333333333333333703, 0.3333333333333333703, 0.3333333333333333703, 0.3333333333333333703, 0.3333333333333333703, 0.3333333333333333703, 0.3333333333333333703, 0.3333333333333333703, 0.3333333333333333703, 0.3333333333333333703, 0.3333333333333333703, 0.3333333333333333703, 0.3333333333333333703, 0.3333333333333333703, 0.3333333333333333703, 0.3333333333333333703, 0.3333333333333333703, 0.3333333333333333703, 0.3333333333333333703, 0.3333333333333333703, 0.3333333333333333703, 0.3333333333333333703, 0.3333333333333333703, 0.3333333333333333703, 0.3333333333333333703),
 ( 1.000000000000000000, 1.000000000000000000, 1.000000000000000000, 1.000000000000000000, 1.000000000000000000, 1.000000000000000000, 1.000000000000000000, 1.000000000000000000, 1.000000000000000000, 1.000000000000000000, 1.000000000000000000, 1.000000000000000000, 1.000000000000000000, 1.000000000000000000, 1.000000000000000000, 1.000000000000000000, 1.000000000000000000, 1.000000000000000000, 1.000000000000000000, 1.000000000000000000, 1.000000000000000000, 1.000000000000000000, 1.000000000000000000, 1.000000000000000000, 1.000000000000000000, 1.000000000000000000, 1.000000000000000000, 1.000000000000000000, 1.000000000000000000, 1.000000000000000000) ) ) 
 REPRESENTATION_ITEM ( '' )  SURFACE ( )  );
#17743 = CARTESIAN_POINT ( 'NONE',  ( -86.96347745069644475, 12.89780903124410472, -43.67073346367977393 ) ) ;
#17744 = CARTESIAN_POINT ( 'NONE',  ( 91.82158438592158234, -6.516925787240506436E-14, 22.79471317813470321 ) ) ;
#17745 = CARTESIAN_POINT ( 'NONE',  ( -100.7734535825088500, 12.25131212657428748, 44.31723036834913643 ) ) ;
#17746 = EDGE_CURVE ( 'NONE', #19647, #16477, #23568, .T. ) ;
#17747 = CARTESIAN_POINT ( 'NONE',  ( -105.3755690713226585, -21.75974354311652448, -40.00000000000002132 ) ) ;
#17748 = CARTESIAN_POINT ( 'NONE',  ( 169.9999999999999716, -22.62041470344880523, -9.369682556672316309 ) ) ;
#17749 = CARTESIAN_POINT ( 'NONE',  ( 200.0000000000000000, 12.97704027674654270, 13.88623514161034045 ) ) ;
#17750 = ADVANCED_FACE ( 'NONE', ( #7382 ), #12319, .T. ) ;
#17751 = ADVANCED_FACE ( 'NONE', ( #5501 ), #20488, .T. ) ;
#17752 = CARTESIAN_POINT ( 'NONE',  ( -86.90968602935149079, -7.324300800229181618, -20.05592747609932758 ) ) ;
#17753 = CARTESIAN_POINT ( 'NONE',  ( 165.3321726438082351, -26.53500608755489054, 0.000000000000000000 ) ) ;
#17754 = CARTESIAN_POINT ( 'NONE',  ( 200.0000000000000000, 14.14213562373142352, -42.42640687119268961 ) ) ;
#17755 = CARTESIAN_POINT ( 'NONE',  ( -105.4741150117381778, 19.77569912954994891, -7.943527260753209696 ) ) ;
#17756 = CARTESIAN_POINT ( 'NONE',  ( -105.3755690713226727, -2.472783935621397949E-13, 21.75974354311649961 ) ) ;
#17757 = CARTESIAN_POINT ( 'NONE',  ( -56.48582580120558561, 6.472252184284607246, -50.09629031063960269 ) ) ;
#17759 = CARTESIAN_POINT ( 'NONE',  ( -198.0356074513804572, 10.87444709761036066, -67.44298959253325165 ) ) ;
#17758 = CARTESIAN_POINT ( 'NONE',  ( -100.7734535825088358, -12.25131212657475643, -12.25131212657495539 ) ) ;
#17760 = CARTESIAN_POINT ( 'NONE',  ( 184.8905102610680444, -14.79361573936330565, -41.77492675556016621 ) ) ;
#17761 = CARTESIAN_POINT ( 'NONE',  ( -198.0356074513804572, -10.87444709759729911, 10.87444709759714812 ) ) ;
#17762 = CARTESIAN_POINT ( 'NONE',  ( -86.86493150571116928, 19.77569912839177846, -7.943527260495974573 ) ) ;
#17764 = CARTESIAN_POINT ( 'NONE',  ( 57.59792236341149163, -40.00000000000014211, 37.56421063658172699 ) ) ;
#17763 = CARTESIAN_POINT ( 'NONE',  ( 200.0000000000000000, 14.14213562373041455, 42.42640687119311593 ) ) ;
#17765 = CARTESIAN_POINT ( 'NONE',  ( 184.8905102610680444, 14.79361573936366092, 41.77492675556006674 ) ) ;
#17766 = FACE_OUTER_BOUND ( 'NONE', #21084, .T. ) ;
#17767 = CARTESIAN_POINT ( 'NONE',  ( -198.0356074513804572, 15.37879056873066830, 40.00000000000002132 ) ) ;
#17768 = ORIENTED_EDGE ( 'NONE', *, *, #23947, .T. ) ;
#17769 = CARTESIAN_POINT ( 'NONE',  ( 14.38125909742180220, 39.01709431150916885, -17.55144818341463164 ) ) ;
#17770 = DIRECTION ( 'NONE',  ( 1.000000000000000000, 1.836970198721030181E-16, 0.000000000000000000 ) ) ;
#17771 = CARTESIAN_POINT ( 'NONE',  ( -16.41532015025260804, -12.95569205545558766, -42.70629200445775098 ) ) ;
#17772 = CARTESIAN_POINT ( 'NONE',  ( -105.3755690713226585, -21.75974354311652448, 40.00000000000002132 ) ) ;
#17773 = EDGE_LOOP ( 'NONE', ( #25333, #3079, #11425, #25168 ) ) ;
#17774 = CARTESIAN_POINT ( 'NONE',  ( -4.039451493210497901, 23.44932283416708074, -43.00522595893983890 ) ) ;
#17775 = CARTESIAN_POINT ( 'NONE',  ( 200.0000000000002274, -16.15590588650048787, 10.03807108387658786 ) ) ;
#17776 = CARTESIAN_POINT ( 'NONE',  ( -3.336279363872675319, -17.94861674415315278, 43.33179396957154950 ) ) ;
#17777 = CARTESIAN_POINT ( 'NONE',  ( 20.16956056504004380, 23.97604322321460657, -43.71646652951380219 ) ) ;
#17778 = CARTESIAN_POINT ( 'NONE',  ( 199.0066757862822726, 19.23093628729661475, -5.478378800400602877 ) ) ;
#17779 = UNCERTAINTY_MEASURE_WITH_UNIT (LENGTH_MEASURE( 1.000000000000000082E-05 ), #18682, 'distance_accuracy_value', 'NONE');
#17780 = B_SPLINE_CURVE_WITH_KNOTS ( 'NONE', 3,
 ( #26259, #11586, #17707, #3753, #16113, #11858 ),
 .UNSPECIFIED., .F., .F.,
 ( 4, 2, 4 ),
 ( 0.3689590070116581799, 0.3867117631979620773, 0.4044645193949217843 ),
 .UNSPECIFIED. ) ;
#17781 = DIRECTION ( 'NONE',  ( -1.000000000000000000, -0.000000000000000000, -0.000000000000000000 ) ) ;
#17782 = CARTESIAN_POINT ( 'NONE',  ( -238.4067589809705794, -4.716212492215116094E-14, 0.9644942799825824142 ) ) ;
#17783 = CARTESIAN_POINT ( 'NONE',  ( -190.0000000000000000, 82.50000000000008527, 52.49999999999979394 ) ) ;
#17784 = CARTESIAN_POINT ( 'NONE',  ( -30.26275506840325136, 57.76657404653985139, -1.198031551615314161 ) ) ;
#17785 = CARTESIAN_POINT ( 'NONE',  ( -135.8532207217289738, 9.153146818113548022, 40.00000000000002132 ) ) ;
#17787 = CARTESIAN_POINT ( 'NONE',  ( -362.0709805440841365, -4.857225732735059864E-14, 0.000000000000000000 ) ) ;
#17786 = CARTESIAN_POINT ( 'NONE',  ( 83.06440094993928369, -10.91839312090031378, -23.65491511364134070 ) ) ;
#17788 = CARTESIAN_POINT ( 'NONE',  ( 151.7948205124836250, 33.23291073765556547, 0.000000000000000000 ) ) ;
#17789 = CARTESIAN_POINT ( 'NONE',  ( 136.1360204305621266, 35.03383547441298163, -40.00000000000002132 ) ) ;
#17790 = CARTESIAN_POINT ( 'NONE',  ( 146.6084372240433993, -34.62501878078303008, 0.000000000000000000 ) ) ;
#17791 = CARTESIAN_POINT ( 'NONE',  ( -100.7734535825088358, 1.654174317907124744E-13, -17.32597176626811120 ) ) ;
#17792 = DIRECTION ( 'NONE',  ( 0.000000000000000000, 0.000000000000000000, 1.000000000000000000 ) ) ;
#17793 = CARTESIAN_POINT ( 'NONE',  ( -56.48582580120559982, 34.75652343174628101, -21.81201906317743067 ) ) ;
#17794 = VERTEX_POINT ( 'NONE', #3837 ) ;
#17795 = DIRECTION ( 'NONE',  ( 1.000000000000000000, 1.836970198721030181E-16, -0.000000000000000000 ) ) ;
#17796 = DIRECTION ( 'NONE',  ( 0.000000000000000000, -1.000000000000000000, 0.000000000000000000 ) ) ;
#17797 = CARTESIAN_POINT ( 'NONE',  ( 136.1360204305621266, -24.77266263493151044, 24.77266263493093135 ) ) ;
#17798 = CARTESIAN_POINT ( 'NONE',  ( -196.0240758340695777, 48.96019759410240368, -14.12332442061102356 ) ) ;
#17799 = CONTEXT_DEPENDENT_SHAPE_REPRESENTATION ( #12060, #13993 ) ;
#17800 = EDGE_LOOP ( 'NONE', ( #1241, #15012, #16379, #21140 ) ) ;
#17801 = ORIENTED_EDGE ( 'NONE', *, *, #1926, .T. ) ;
#17802 = CARTESIAN_POINT ( 'NONE',  ( -30.26275506840324070, -29.48230279907780016, -27.08623969584605362 ) ) ;
#17803 = CARTESIAN_POINT ( 'NONE',  ( 23.30336656375561688, -42.87878279885800481, -23.35569295765272457 ) ) ;
#17804 = ORIENTED_EDGE ( 'NONE', *, *, #2567, .F. ) ;
#17805 = CARTESIAN_POINT ( 'NONE',  ( -86.96347745069644475, -21.75974354311652093, -40.00000000000002132 ) ) ;
#17806 = CARTESIAN_POINT ( 'NONE',  ( -89.91646883261441303, -20.29783361052119872, 8.407637968115118099 ) ) ;
#17807 = ORIENTED_EDGE ( 'NONE', *, *, #8591, .T. ) ;
#17808 = CARTESIAN_POINT ( 'NONE',  ( 199.9999999999996305, 13.20330696038688068, 13.67115712520468840 ) ) ;
#17809 = CARTESIAN_POINT ( 'NONE',  ( -200.0000000000000284, -82.49999999999990052, 52.49999999999977973 ) ) ;
#17810 = CARTESIAN_POINT ( 'NONE',  ( -105.3755690713226727, 12.89780903124400879, 12.89780903124407452 ) ) ;
#17811 = CARTESIAN_POINT ( 'NONE',  ( -105.4741150117390021, -7.943527260764932763, -19.77569912954469800 ) ) ;
#17812 = CARTESIAN_POINT ( 'NONE',  ( 151.7948205124836250, 1.439163438361279259E-13, -33.23291073765553705 ) ) ;
#17813 = CARTESIAN_POINT ( 'NONE',  ( 4.995406935893288214, 15.24977328854832770, 40.00000000000002132 ) ) ;
#17814 = CARTESIAN_POINT ( 'NONE',  ( 14.38125909742181108, 39.01709431150961649, -39.01709431150867147 ) ) ;
#17815 = FACE_OUTER_BOUND ( 'NONE', #23138, .T. ) ;
#17816 = CARTESIAN_POINT ( 'NONE',  ( -213.1075012329537230, -8.703598725189323045E-14, 13.71589010951911902 ) ) ;
#17817 = CARTESIAN_POINT ( 'NONE',  ( -102.2610585947572872, -15.74993999358175678, 15.74993999358135710 ) ) ;
#17818 = CARTESIAN_POINT ( 'NONE',  ( 146.6084372240433709, -39.99999999999993605, -5.374981219217395356 ) ) ;
#17819 = EDGE_CURVE ( 'NONE', #8765, #17548, #18475, .T. ) ;
#17820 = CARTESIAN_POINT ( 'NONE',  ( -135.8532207217289738, -50.09629031063965243, -6.472252184284438492 ) ) ;
#17821 = CARTESIAN_POINT ( 'NONE',  ( 91.82158438592158234, 17.20528682183301683, 0.000000000000000000 ) ) ;
#17822 = CARTESIAN_POINT ( 'NONE',  ( -30.26275506840324070, -29.48230279907780016, -27.08623969584605362 ) ) ;
#17823 = CARTESIAN_POINT ( 'NONE',  ( -280.0000000000000000, 9.999999999999948486, 1.224646799147346354E-15 ) ) ;
#17824 = AXIS2_PLACEMENT_3D ( 'NONE', #21842, #25593, #23704 ) ;
#17825 = CYLINDRICAL_SURFACE ( 'NONE', #17864, 28.79780246617542616 ) ;
#17826 = CARTESIAN_POINT ( 'NONE',  ( 146.6084372240433993, 24.48358557860307272, 24.48358557860347418 ) ) ;
#17827 = CARTESIAN_POINT ( 'NONE',  ( 130.8568914410475372, 1.429239637432775288E-13, -34.05028731879788495 ) ) ;
#17828 = CARTESIAN_POINT ( 'NONE',  ( 57.59792236341147031, -1.722363176415123043, 54.84617931850879557 ) ) ;
#17829 = CARTESIAN_POINT ( 'NONE',  ( 151.7948205124836250, 23.49921654116328540, 23.49921654116366554 ) ) ;
#17830 = CARTESIAN_POINT ( 'NONE',  ( -188.3120606736147806, -23.45204117844517810, -43.00889065703323411 ) ) ;
#17831 = CARTESIAN_POINT ( 'NONE',  ( 0.2972598230769976091, -10.13633138497479180, 10.13633138497468522 ) ) ;
#17832 = ORIENTED_EDGE ( 'NONE', *, *, #19523, .F. ) ;
#17833 = CARTESIAN_POINT ( 'NONE',  ( -135.8532207217289738, 21.81201906317798134, -21.81201906317747685 ) ) ;
#17834 = DIRECTION ( 'NONE',  ( 0.000000000000000000, 0.000000000000000000, -1.000000000000000000 ) ) ;
#17835 = CARTESIAN_POINT ( 'NONE',  ( -56.48582580120559982, 9.153146818113574668, -40.00000000000002132 ) ) ;
#17836 = FILL_AREA_STYLE ('',( #3893 ) ) ;
#17837 = CARTESIAN_POINT ( 'NONE',  ( 57.59792236341147031, -30.00663442387662627, -26.56190807104723461 ) ) ;
#17838 = CARTESIAN_POINT ( 'NONE',  ( -87.13361725324189422, 0.6800178180866376376, 21.49321519332665176 ) ) ;
#17839 = EDGE_LOOP ( 'NONE', ( #13020, #22817 ) ) ;
#17840 = CARTESIAN_POINT ( 'NONE',  ( 184.8905102610680444, -1.851754852062639767E-13, 20.92133201514444352 ) ) ;
#17841 = CARTESIAN_POINT ( 'NONE',  ( 200.0000000000000000, 69.99999999999998579, 8.572527594031466682E-15 ) ) ;
#17842 = CARTESIAN_POINT ( 'NONE',  ( -4.112199523541912427, 23.43514144949416078, 42.98379141459026442 ) ) ;
#17843 = ORIENTED_EDGE ( 'NONE', *, *, #13075, .T. ) ;
#17844 = VERTEX_POINT ( 'NONE', #9421 ) ;
#17845 = CARTESIAN_POINT ( 'NONE',  ( 151.7948205124836534, 6.767089262349062828, -40.00000000000002132 ) ) ;
#17846 = CARTESIAN_POINT ( 'NONE',  ( 163.1118516004056573, 19.27778845538780317, -19.27778845538757224 ) ) ;
#17847 = CARTESIAN_POINT ( 'NONE',  ( 170.2234770963711128, 40.00000000000000000, 15.44714144992830462 ) ) ;
#17848 = CARTESIAN_POINT ( 'NONE',  ( 35.93675038278705358, 12.87543821110860520, -42.26938935684505338 ) ) ;
#17849 = PRESENTATION_LAYER_ASSIGNMENT (  '', '', ( #18274 ) ) ;
#17850 = CARTESIAN_POINT ( 'NONE',  ( -213.1075012329537230, 37.98287015391280619, -37.98287015391192512 ) ) ;
#17851 = CARTESIAN_POINT ( 'NONE',  ( 98.29820294267312875, 7.653668647304333383, -18.47759065023115355 ) ) ;
#17852 = CARTESIAN_POINT ( 'NONE',  ( 98.29820294267312875, 7.653668647304333383, -18.47759065023115355 ) ) ;
#17853 = CARTESIAN_POINT ( 'NONE',  ( 199.0142490642952566, 16.24935999037262846, 11.66321269349018941 ) ) ;
#17854 = CARTESIAN_POINT ( 'NONE',  ( -129.2920181229026753, 10.46331487454523845, 25.26067667728931809 ) ) ;
#17855 = CARTESIAN_POINT ( 'NONE',  ( 6.615221834201326701, -24.79576599683120008, -44.82734842560605415 ) ) ;
#17856 = CARTESIAN_POINT ( 'NONE',  ( 0.2972598230770100991, -38.42060263243632079, -38.42060263243699580 ) ) ;
#17857 = CARTESIAN_POINT ( 'NONE',  ( 107.5473083967383445, -16.96446921415050113, 16.96446921415010678 ) ) ;
#17858 = CARTESIAN_POINT ( 'NONE',  ( 184.8905102610680444, -41.77492675555986779, -14.79361573936407304 ) ) ;
#17859 = CARTESIAN_POINT ( 'NONE',  ( -238.4067589809705794, -3.369206980223063916E-14, -0.9644942799825824142 ) ) ;
#17860 = CARTESIAN_POINT ( 'NONE',  ( -716.9846540392142060, 66.50000000000009948, 61.50000000000005684 ) ) ;
#17861 = PLANE ( 'NONE',  #6669 ) ;
#17862 = CARTESIAN_POINT ( 'NONE',  ( 163.1118516004056573, -12.73709011382472234, -2.449293598294708485E-15 ) ) ;
#17863 = CARTESIAN_POINT ( 'NONE',  ( 146.6084372240433709, 52.76785682606519146, 3.800685668858932775 ) ) ;
#17864 = AXIS2_PLACEMENT_3D ( 'NONE', #5344, #23953, #11203 ) ;
#17865 = CARTESIAN_POINT ( 'NONE',  ( 19.06497207195982924, -54.19242893257843008, 40.00000000000002132 ) ) ;
#17866 = CARTESIAN_POINT ( 'NONE',  ( 199.9999999999999432, -14.14213562373115884, 14.14213562373085153 ) ) ;
#17867 = CARTESIAN_POINT ( 'NONE',  ( -114.4712152604451347, 20.46962080079592994, 7.710842095506693639 ) ) ;
#17868 = CARTESIAN_POINT ( 'NONE',  ( 170.2234770963711128, -17.36149277826995885, 39.20704971665388427 ) ) ;
#17869 = CARTESIAN_POINT ( 'NONE',  ( 200.0000000000000000, -20.00000000000006750, -40.00000000000002132 ) ) ;
#17870 = ORIENTED_EDGE ( 'NONE', *, *, #14818, .F. ) ;
#17871 = DIRECTION ( 'NONE',  ( 0.000000000000000000, 0.000000000000000000, 1.000000000000000000 ) ) ;
#17872 = CARTESIAN_POINT ( 'NONE',  ( -16.41654234047147654, -12.95560590355978725, 42.70586891282371056 ) ) ;
#17873 = CARTESIAN_POINT ( 'NONE',  ( 184.8905102610680444, 13.49065550809817715, -43.07788698682574591 ) ) ;
#17874 = CARTESIAN_POINT ( 'NONE',  ( 14.38125909742182529, -40.00000000000021316, 55.17850393974251944 ) ) ;
#17875 = CIRCLE ( 'NONE', #24268, 5.000000000000011546 ) ;
#17876 = CARTESIAN_POINT ( 'NONE',  ( 19.06497207195979726, 38.31983398719604139, 18.24870850772803976 ) ) ;
#17877 = LINE ( 'NONE', #22430, #1981 ) ;
#17878 = VECTOR ( 'NONE', #6419, 1000.000000000000000 ) ;
#17879 = CARTESIAN_POINT ( 'NONE',  ( 184.8905102610680444, 19.07866798485562398, -40.00000000000002132 ) ) ;
#17880 = PLANE ( 'NONE',  #13415 ) ;
#17881 = CARTESIAN_POINT ( 'NONE',  ( 199.9999999999996021, 18.99368777275013898, 0.6330478706754758544 ) ) ;
#17882 = CARTESIAN_POINT ( 'NONE',  ( 199.9999999999999147, -9.234286251058666295, -16.61017430452723787 ) ) ;
#17883 = CARTESIAN_POINT ( 'NONE',  ( -162.0762913951021176, 57.76657433523994456, -1.198031840315424867 ) ) ;
#17884 = CARTESIAN_POINT ( 'NONE',  ( -100.7734535825088500, 16.03295912088740494, -40.53558337403661938 ) ) ;
#17885 = CARTESIAN_POINT ( 'NONE',  ( 192.4448373802100889, 14.14213562375893574, -14.14213562375874922 ) ) ;
#17886 = CARTESIAN_POINT ( 'NONE',  ( -87.12812962367802072, 14.21201470107229881, -16.13326835689685623 ) ) ;
#17887 = CARTESIAN_POINT ( 'NONE',  ( 130.8568914410475088, 24.07718906446937623, -32.49135343045455215 ) ) ;
#17889 = CARTESIAN_POINT ( 'NONE',  ( -28.75808802591302538, 12.03522322449776638, 38.33175228464047990 ) ) ;
#17888 = CARTESIAN_POINT ( 'NONE',  ( 136.1360204305621551, 24.77266263493153176, -31.79587985999237887 ) ) ;
#17890 = CARTESIAN_POINT ( 'NONE',  ( 146.6084372240433709, -52.76785682606510619, -3.800685668859292043 ) ) ;
#17891 = CARTESIAN_POINT ( 'NONE',  ( 192.4448373802100889, -20.00000000003938538, 0.000000000000000000 ) ) ;
#17892 = CARTESIAN_POINT ( 'NONE',  ( 160.7895100360958622, 28.48799984206444336, 0.000000000000000000 ) ) ;
#17893 = ADVANCED_FACE ( 'NONE', ( #25541 ), #3434, .T. ) ;
#17895 = CARTESIAN_POINT ( 'NONE',  ( -86.96347745069643054, -39.99999999999995737, -21.75974354311664527 ) ) ;
#17894 = CARTESIAN_POINT ( 'NONE',  ( 146.6084372240433709, 3.800685668858042821, 52.76785682606522698 ) ) ;
#17896 = CARTESIAN_POINT ( 'NONE',  ( -238.4067589809705794, 27.60227080167040370, 28.96627169325338613 ) ) ;
#17897 = CARTESIAN_POINT ( 'NONE',  ( -259.2033419157646676, 21.55415060305790931, 35.01439189186571355 ) ) ;
#17898 = CONICAL_SURFACE ( 'NONE', #5585, 21.53474504356810115, 0.7853981633974378429 ) ;
#17899 = CARTESIAN_POINT ( 'NONE',  ( -91.56559293963834989, 17.32597176626808988, 40.00000000000002132 ) ) ;
#17900 = ORIENTED_EDGE ( 'NONE', *, *, #6239, .T. ) ;
#17901 = CARTESIAN_POINT ( 'NONE',  ( -162.0762913951020892, 57.76657433537918251, 1.198031840455469066 ) ) ;
#17902 = EDGE_CURVE ( 'NONE', #993, #17327, #4961, .T. ) ;
#17903 =( BOUNDED_SURFACE ( )  B_SPLINE_SURFACE ( 3, 2, ( 
 ( #16192, #6090, #9812 ),
 ( #6218, #13926, #21924 ),
 ( #7798, #15913, #20326 ),
 ( #26332, #24182, #2103 ),
 ( #18317, #3973, #22062 ),
 ( #100, #22462, #14330 ),
 ( #20460, #4242, #12332 ),
 ( #24046, #5823, #2234 ),
 ( #20063, #14065, #1839 ),
 ( #10342, #7938, #12070 ),
 ( #16056, #20188, #10077 ),
 ( #10746, #12461, #16463 ),
 ( #14591, #25123, #12600 ),
 ( #18451, #24992, #22857 ),
 ( #13005, #4497, #4633 ),
 ( #8471, #6342, #6743 ),
 ( #2902, #18720, #12735 ),
 ( #2770, #14725, #14856 ),
 ( #16590, #8877, #6874 ),
 ( #4896, #18857, #771 ),
 ( #505, #16860, #22991 ),
 ( #20856, #2637, #8342 ),
 ( #22720, #22594, #228 ),
 ( #8611, #20730, #4371 ),
 ( #2498, #10477, #21126 ),
 ( #10608, #16721, #24585 ),
 ( #14463, #4767, #637 ),
 ( #14989, #24853, #8742 ),
 ( #18591, #16987, #6605 ),
 ( #12871, #20988, #10879 ),
 ( #18994, #23123, #20588 ),
 ( #2363, #369, #24722 ),
 ( #6478, #21253, #11010 ),
 ( #13135, #19119, #7000 ) ),
 .UNSPECIFIED., .F., .F., .F. ) 
 B_SPLINE_SURFACE_WITH_KNOTS ( ( 4, 2, 2, 2, 2, 2, 2, 2, 2, 2, 2, 2, 2, 2, 2, 2, 4 ),
 ( 3, 3 ),
 ( 0.005135431517079875642, 0.02907016617529989064, 0.05300490083351990650, 0.07693963549173991889, 0.08292331915629491679, 0.08441924007243367667, 0.08446598760106301118, 0.08448936136537768538, 0.08451273512969234569, 0.08460623018695101472, 0.08479322030146836664, 0.08516720053050305661, 0.08591516098857242267, 0.08890700282084992856, 0.09189884465312743445, 0.09489068648540494033, 0.1008743701499599382 ),
 ( 0.000000000000000000, 1.000000000000000000 ),
 .UNSPECIFIED. ) 
 GEOMETRIC_REPRESENTATION_ITEM ( )  RATIONAL_B_SPLINE_SURFACE ( (
 ( 1.000000000000000000, 0.9997813423552078804, 1.000000000000000000),
 ( 1.000000000000000000, 0.9991063894442812066, 1.000000000000000000),
 ( 1.000000000000000000, 0.9968824679670513778, 1.000000000000000000),
 ( 1.000000000000000000, 0.9891556708430853107, 1.000000000000000000),
 ( 1.000000000000000000, 0.9836552227706821805, 1.000000000000000000),
 ( 1.000000000000000000, 0.9690804699595866323, 1.000000000000000000),
 ( 1.000000000000000000, 0.9600093828092017834, 1.000000000000000000),
 ( 1.000000000000000000, 0.9461484455228768020, 1.000000000000000000),
 ( 1.000000000000000000, 0.9432496483672407894, 1.000000000000000000),
 ( 1.000000000000000000, 0.9394619383806346313, 1.000000000000000000),
 ( 1.000000000000000000, 0.9386961831920884736, 1.000000000000000000),
 ( 1.000000000000000000, 0.9378979462694522207, 1.000000000000000000),
 ( 1.000000000000000000, 0.9378737491732492826, 1.000000000000000000),
 ( 1.000000000000000000, 0.9378374413774239748, 1.000000000000000000),
 ( 1.000000000000000000, 0.9378252326299131303, 1.000000000000000000),
 ( 1.000000000000000000, 0.9378013115143170042, 1.000000000000000000),
 ( 1.000000000000000000, 0.9377893564346097000, 1.000000000000000000),
 ( 1.000000000000000000, 0.9377296084626357553, 1.000000000000000000),
 ( 1.000000000000000000, 0.9376818978498919765, 1.000000000000000000),
 ( 1.000000000000000000, 0.9375390306864408441, 1.000000000000000000),
 ( 1.000000000000000000, 0.9374441388112029205, 1.000000000000000000),
 ( 1.000000000000000000, 0.9371605328928167555, 1.000000000000000000),
 ( 1.000000000000000000, 0.9369728885717006905, 1.000000000000000000),
 ( 1.000000000000000000, 0.9364143219789186068, 1.000000000000000000),
 ( 1.000000000000000000, 0.9360477663173443208, 1.000000000000000000),
 ( 1.000000000000000000, 0.9342452504721948658, 1.000000000000000000),
 ( 1.000000000000000000, 0.9329001521055332313, 1.000000000000000000),
 ( 1.000000000000000000, 0.9304320728630449677, 1.000000000000000000),
 ( 1.000000000000000000, 0.9293115496651194185, 1.000000000000000000),
 ( 1.000000000000000000, 0.9273349178229508549, 1.000000000000000000),
 ( 1.000000000000000000, 0.9264755994062412459, 1.000000000000000000),
 ( 1.000000000000000000, 0.9243018539388534460, 1.000000000000000000),
 ( 1.000000000000000000, 0.9233922906946859799, 1.000000000000000000),
 ( 1.000000000000000000, 0.9230540990195957862, 1.000000000000000000) ) ) 
 REPRESENTATION_ITEM ( '' )  SURFACE ( )  );
#17904 = DIRECTION ( 'NONE',  ( 0.000000000000000000, 1.000000000000000000, 0.000000000000000000 ) ) ;
#17905 = DIRECTION ( 'NONE',  ( 0.000000000000000000, 0.000000000000000000, -1.000000000000000000 ) ) ;
#17906 = CARTESIAN_POINT ( 'NONE',  ( 0.2972598230769930572, 14.33493731733933352, 0.000000000000000000 ) ) ;
#17907 = ADVANCED_FACE ( 'NONE', ( #9297 ), #1605, .T. ) ;
#17908 = EDGE_CURVE ( 'NONE', #16948, #151, #21094, .T. ) ;
#17909 = ORIENTED_EDGE ( 'NONE', *, *, #10475, .F. ) ;
#17910 = CARTESIAN_POINT ( 'NONE',  ( -188.3120147333550563, -43.00887716025417262, 23.45203116714296598 ) ) ;
#17911 = LINE ( 'NONE', #26054, #25531 ) ;
#17912 = CARTESIAN_POINT ( 'NONE',  ( 6.984886629842144146, -24.81009931999644635, 44.84679502273391449 ) ) ;
#17913 = CARTESIAN_POINT ( 'NONE',  ( 22.01478053667198864, 23.63228119973664931, -43.25192662397402188 ) ) ;
#17914 = CARTESIAN_POINT ( 'NONE',  ( 199.0064300139308102, 18.94043123351016433, -6.416860702434988184 ) ) ;
#17915 = CIRCLE ( 'NONE', #26022, 29.99999999999999289 ) ;
#17916 = CARTESIAN_POINT ( 'NONE',  ( 118.9130007099546305, -25.80693111732297496, 10.68958087202318374 ) ) ;
#17917 = CARTESIAN_POINT ( 'NONE',  ( -200.0000000000000000, -74.99999999999995737, 0.000000000000000000 ) ) ;
#17918 = CARTESIAN_POINT ( 'NONE',  ( -162.0762913951020892, 29.48230308784799902, -29.48230308784730980 ) ) ;
#17919 = CARTESIAN_POINT ( 'NONE',  ( 184.8905102610680444, -19.07866798485554938, 40.00000000000002132 ) ) ;
#17921 = CARTESIAN_POINT ( 'NONE',  ( -613.0749189761168054, 29.88886548687010247, -26.58473085348082776 ) ) ;
#17920 = CARTESIAN_POINT ( 'NONE',  ( -114.4388184736417173, 8.352332320002227917, -20.16431396440712831 ) ) ;
#17922 = CARTESIAN_POINT ( 'NONE',  ( -370.0000000000001137, -4.617994102837407382E-14, 19.53474504356807273 ) ) ;
#17923 = CARTESIAN_POINT ( 'NONE',  ( -162.0762913951020892, -41.69427287672991866, -40.00000000000002132 ) ) ;
#17924 = CARTESIAN_POINT ( 'NONE',  ( 163.1118516004056573, -27.26290988616869626, 40.00000000000002132 ) ) ;
#17925 = CARTESIAN_POINT ( 'NONE',  ( -86.96347745069644475, 1.775309070576523494E-13, -18.24025645688352881 ) ) ;
#17926 = CARTESIAN_POINT ( 'NONE',  ( 98.29820294267359770, -8.858778887854322548, 17.94316440882988317 ) ) ;
#17927 = CARTESIAN_POINT ( 'NONE',  ( 14.38125909742180752, 17.55144818341503665, -39.01709431150898411 ) ) ;
#17928 = VERTEX_POINT ( 'NONE', #4503 ) ;
#17929 = CARTESIAN_POINT ( 'NONE',  ( 98.29820294267312875, 7.653668647304333383, -18.47759065023115355 ) ) ;
#17930 = CARTESIAN_POINT ( 'NONE',  ( -105.3755690713226727, -15.38646221621786481, -15.38646221621789856 ) ) ;
#17931 = DIRECTION ( 'NONE',  ( -1.000000000000000000, -0.000000000000000000, -0.000000000000000000 ) ) ;
#17932 = PRODUCT_CONTEXT ( 'NONE', #17997, 'mechanical' ) ;
#17933 = ORIENTED_EDGE ( 'NONE', *, *, #20627, .F. ) ;
#17934 = VERTEX_POINT ( 'NONE', #18726 ) ;
#17935 = CARTESIAN_POINT ( 'NONE',  ( -208.1127848780264742, -38.89260858015728672, -17.67593391476669851 ) ) ;
#17936 = CARTESIAN_POINT ( 'NONE',  ( 23.35928221536256899, -42.86167611819477230, -23.34300348377128742 ) ) ;
#17937 = EDGE_CURVE ( 'NONE', #2955, #5450, #776, .T. ) ;
#17938 = ORIENTED_EDGE ( 'NONE', *, *, #6860, .T. ) ;
#17939 = CARTESIAN_POINT ( 'NONE',  ( 170.2234770963711128, 15.44714144992819627, -40.00000000000002132 ) ) ;
#17940 = CARTESIAN_POINT ( 'NONE',  ( -102.4309680865952146, -20.17061239838023923, 8.733065090080391002 ) ) ;
#17941 = EDGE_LOOP ( 'NONE', ( #23175, #15135, #20377, #2286 ) ) ;
#17942 = CARTESIAN_POINT ( 'NONE',  ( 200.0000000000000568, 16.12943746570313053, 10.05448153537135347 ) ) ;
#17943 = CARTESIAN_POINT ( 'NONE',  ( -105.3175672232813724, 20.76674186929500365, -5.407869933822353481 ) ) ;
#17944 = CARTESIAN_POINT ( 'NONE',  ( -162.0762913951020892, 57.76657433537918251, 1.198031840455469066 ) ) ;
#17945 = CARTESIAN_POINT ( 'NONE',  ( -187.3037411062139483, -42.71163782367793260, -23.25513534570746899 ) ) ;
#17946 = CARTESIAN_POINT ( 'NONE',  ( 184.8905102610680444, -40.00000000000005684, 19.07866798485543569 ) ) ;
#17947 = CARTESIAN_POINT ( 'NONE',  ( -259.2033419157646676, 30.48217210827734647, 40.00000000000002132 ) ) ;
#17948 = CARTESIAN_POINT ( 'NONE',  ( 130.8568914410475372, 4.207082182992923691, -4.207082182992794017 ) ) ;
#17949 = FACE_OUTER_BOUND ( 'NONE', #25947, .T. ) ;
#17950 = CARTESIAN_POINT ( 'NONE',  ( -100.7734535825088500, -39.99999999999995737, -22.67402823373205578 ) ) ;
#17951 = CARTESIAN_POINT ( 'NONE',  ( -238.4067589809705794, -40.00000000000005684, -0.9644942799830014124 ) ) ;
#17952 = CARTESIAN_POINT ( 'NONE',  ( 169.9999999999999716, -9.369682556672181306, -22.62041470344887273 ) ) ;
#17953 = CARTESIAN_POINT ( 'NONE',  ( -208.1127848780264742, -10.60833733268345469, 67.17687982760682530 ) ) ;
#17954 = CARTESIAN_POINT ( 'NONE',  ( -280.0000000000000568, -20.00000000000006395, -40.00000000000002132 ) ) ;
#17955 = CARTESIAN_POINT ( 'NONE',  ( -280.0000000000000000, -14.14213562373108779, 14.14213562373088529 ) ) ;
#17956 = CARTESIAN_POINT ( 'NONE',  ( -190.0000000000000000, 71.50000000000009948, -66.50000000000005684 ) ) ;
#17957 = DIRECTION ( 'NONE',  ( -1.000000000000000000, 0.000000000000000000, 0.000000000000000000 ) ) ;
#17958 = CARTESIAN_POINT ( 'NONE',  ( -200.0000000000000000, 61.50000000000009948, 66.50000000000005684 ) ) ;
#17959 = CARTESIAN_POINT ( 'NONE',  ( 136.1360204305621551, -39.99999999999987921, -35.03383547441310242 ) ) ;
#17960 = CARTESIAN_POINT ( 'NONE',  ( 184.8905102610680444, 41.77492675556005253, -14.79361573936377461 ) ) ;
#17961 = CARTESIAN_POINT ( 'NONE',  ( 130.8568914410475372, 24.07718906447210472, 24.07718906447249907 ) ) ;
#17962 = CARTESIAN_POINT ( 'NONE',  ( -188.9524938556051552, -13.86227398172975533, -47.22059665005807716 ) ) ;
#17963 = CARTESIAN_POINT ( 'NONE',  ( -162.0762913951021176, -29.48230308784755493, -27.08623940707632372 ) ) ;
#17964 = ORIENTED_EDGE ( 'NONE', *, *, #23136, .T. ) ;
#17965 = CARTESIAN_POINT ( 'NONE',  ( -56.48582580120559271, -6.472252184284276844, 6.472252184284108978 ) ) ;
#17966 = CARTESIAN_POINT ( 'NONE',  ( 151.7948205124835681, 51.78348778862537927, 4.785054706298732086 ) ) ;
#17967 = CARTESIAN_POINT ( 'NONE',  ( 57.59792236341147031, 2.435789363418171760, 0.000000000000000000 ) ) ;
#17968 = CARTESIAN_POINT ( 'NONE',  ( 98.29820294272414571, 7.653668647302724892, 18.47759065022804137 ) ) ;
#17969 = CARTESIAN_POINT ( 'NONE',  ( -100.7734535825088500, -16.03295912088659492, -40.53558337403696044 ) ) ;
#17970 = DIRECTION ( 'NONE',  ( -1.000000000000000000, -1.836970198721030181E-16, -0.000000000000000000 ) ) ;
#17971 = CARTESIAN_POINT ( 'NONE',  ( -200.0000000000000000, -60.00000000000009948, 7.347880794884132555E-15 ) ) ;
#17972 = VERTEX_POINT ( 'NONE', #16865 ) ;
#17973 = CARTESIAN_POINT ( 'NONE',  ( 200.0000000000000000, 18.50924455979920324, -4.296878913645367781 ) ) ;
#17974 = CARTESIAN_POINT ( 'NONE',  ( -265.6482238768269326, 0.000000000000000000, -39.99999999999997158 ) ) ;
#17975 = CARTESIAN_POINT ( 'NONE',  ( -7.233308327734865983, 17.51119053153846394, 42.27575367454018362 ) ) ;
#17976 = ORIENTED_EDGE ( 'NONE', *, *, #4443, .T. ) ;
#17977 = EDGE_LOOP ( 'NONE', ( #16516, #6701, #4857, #17583 ) ) ;
#17978 = CARTESIAN_POINT ( 'NONE',  ( 4.995406935893288214, 15.24977328854832770, 0.000000000000000000 ) ) ;
#17979 = CARTESIAN_POINT ( 'NONE',  ( 199.0079861221352360, 1.294590733001960592, -19.95474696286750671 ) ) ;
#17980 = CARTESIAN_POINT ( 'NONE',  ( -110.0574646603687512, -6.254026121474651312, -19.22569902442541334 ) ) ;
#17981 = CARTESIAN_POINT ( 'NONE',  ( 7.340276910564531576, 44.87059041559415817, -24.82763627182861299 ) ) ;
#17982 = CARTESIAN_POINT ( 'NONE',  ( -91.56559293963834989, -2.543181659092656077E-13, 22.67402823373191723 ) ) ;
#17983 = DIRECTION ( 'NONE',  ( 5.098616525425841937E-32, -2.775557561562890858E-16, -1.000000000000000000 ) ) ;
#17984 = CARTESIAN_POINT ( 'NONE',  ( -82.26522454411171736, -19.58755215917935288, -5.034236609581555832 ) ) ;
#17985 = CARTESIAN_POINT ( 'NONE',  ( 200.0000000000000000, 63.70262460423112572, -57.69613583541415380 ) ) ;
#17986 = CARTESIAN_POINT ( 'NONE',  ( 199.0135736376541615, 16.97384353125803003, 10.58053792802146020 ) ) ;
#17987 = ADVANCED_FACE ( 'NONE', ( #13011 ), #14026, .T. ) ;
#17988 = CARTESIAN_POINT ( 'NONE',  ( -187.8979312699049729, 42.13932507928217319, 17.45467995708709452 ) ) ;
#17989 = CARTESIAN_POINT ( 'NONE',  ( 9.006212071485066417, -14.17897189022234450, -49.32687279761056942 ) ) ;
#17990 = CARTESIAN_POINT ( 'NONE',  ( -208.1127848780264742, -67.17687982760682530, -10.60833733268364298 ) ) ;
#17991 = PRODUCT_DEFINITION ( 'UNKNOWN', '', #11277, #19339 ) ;
#17992 = DIRECTION ( 'NONE',  ( -0.000000000000000000, -1.321694076934715579E-16, -1.000000000000000000 ) ) ;
#17993 = CARTESIAN_POINT ( 'NONE',  ( -56.48582580120558561, -21.81201906317785699, 21.81201906317761896 ) ) ;
#17994 = CARTESIAN_POINT ( 'NONE',  ( 57.59792236341147031, -1.493297263419786540E-14, 2.435789363418160658 ) ) ;
#17995 = CARTESIAN_POINT ( 'NONE',  ( -280.0000000000000000, -14.14213562373118549, 14.14213562373078936 ) ) ;
#17996 = CARTESIAN_POINT ( 'NONE',  ( -198.0356074513804572, 17.40982414986501325, -39.15871834505897198 ) ) ;
#17997 = APPLICATION_CONTEXT ( 'automotive_design' ) ;
#17998 = CARTESIAN_POINT ( 'NONE',  ( 0.2972598230770129857, -54.33493731733938148, 40.00000000000002132 ) ) ;
#17999 = DIRECTION ( 'NONE',  ( -1.836970198721030181E-16, 1.000000000000000000, 0.000000000000000000 ) ) ;
#18000 = CARTESIAN_POINT ( 'NONE',  ( 199.9999999999999432, -19.99999999999988987, -2.449293598294708485E-15 ) ) ;
#18001 = CARTESIAN_POINT ( 'NONE',  ( -105.2243945160626026, 13.27818848189948575, 16.94163139060719203 ) ) ;
#18002 = CARTESIAN_POINT ( 'NONE',  ( 57.59792236341146321, 40.00000000000000711, 2.435789363418579434 ) ) ;
#18003 = CARTESIAN_POINT ( 'NONE',  ( 170.2234770963711128, 10.92277846919210660, -45.64576402573182889 ) ) ;
#18004 = EDGE_CURVE ( 'NONE', #25674, #10228, #15909, .T. ) ;
#18005 = CARTESIAN_POINT ( 'NONE',  ( -56.48582580120559982, -9.153146818113595984, -40.00000000000002132 ) ) ;
#18006 = ORIENTED_EDGE ( 'NONE', *, *, #2639, .T. ) ;
#18007 = EDGE_CURVE ( 'NONE', #17934, #916, #18905, .T. ) ;
#18008 = CARTESIAN_POINT ( 'NONE',  ( 60.14720761603590660, -31.22869220290919756, 15.75494750878411665 ) ) ;
#18009 = CARTESIAN_POINT ( 'NONE',  ( 127.8236149080041173, 11.91256696755823086, 28.75948073575764141 ) ) ;
#18010 = CARTESIAN_POINT ( 'NONE',  ( 130.8568914410475088, 32.49135343045483637, -24.07718906446901030 ) ) ;
#18011 = CARTESIAN_POINT ( 'NONE',  ( 0.2972598230770103767, -40.00000000000021316, 54.33493731733921805 ) ) ;
#18012 = CARTESIAN_POINT ( 'NONE',  ( 136.1360204305621266, -24.77266263493151044, 24.77266263493093135 ) ) ;
#18013 = CARTESIAN_POINT ( 'NONE',  ( 146.6084372240433993, -3.357462877844280890E-13, 34.62501878078305850 ) ) ;
#18014 = CARTESIAN_POINT ( 'NONE',  ( -135.8532207217289738, -9.153146818113595984, 0.000000000000000000 ) ) ;
#18015 = LINE ( 'NONE', #25760, #10444 ) ;
#18016 = CARTESIAN_POINT ( 'NONE',  ( 199.9999999999998579, 13.86282612285610938, 13.00154682524819805 ) ) ;
#18017 = CARTESIAN_POINT ( 'NONE',  ( 199.9999999999999716, -16.91202053066619371, 8.687169125204889042 ) ) ;
#18018 = CARTESIAN_POINT ( 'NONE',  ( 57.59792236341147031, 54.84617931850878136, 1.722363176415705910 ) ) ;
#18019 = CARTESIAN_POINT ( 'NONE',  ( 14.38125909742182529, -39.01709431150879936, -39.01709431150948859 ) ) ;
#18020 = CARTESIAN_POINT ( 'NONE',  ( -110.0368417077424965, 18.74474319002781897, -7.441767003009320369 ) ) ;
#18021 = CARTESIAN_POINT ( 'NONE',  ( -82.26674357280032268, 17.37244534975081933, -10.27857254523484798 ) ) ;
#18022 = CARTESIAN_POINT ( 'NONE',  ( -162.0762913951021176, -29.48230308784793152, 27.08623940707591515 ) ) ;
#18024 = DIRECTION ( 'NONE',  ( 0.000000000000000000, 1.000000000000000000, 0.000000000000000000 ) ) ;
#18023 = CARTESIAN_POINT ( 'NONE',  ( 136.1360204305621266, -3.511608612530630058, -3.511608612530719764 ) ) ;
#18025 = CARTESIAN_POINT ( 'NONE',  ( -259.2033419157646676, -35.01439189186523748, -21.55415060305881170 ) ) ;
#18026 = CARTESIAN_POINT ( 'NONE',  ( -114.4364955367327497, -8.064892380842218600, -20.29001642038850406 ) ) ;
#18027 = CARTESIAN_POINT ( 'NONE',  ( 199.0263771133097350, -13.25980953972711340, 15.03167181779690331 ) ) ;
#18029 = CARTESIAN_POINT ( 'NONE',  ( -91.56559293963834989, -40.00000000000009948, 17.32597176626796553 ) ) ;
#18028 = CARTESIAN_POINT ( 'NONE',  ( -208.1127848780265026, 38.89260858015777700, -38.89260858015687461 ) ) ;
#18030 = CARTESIAN_POINT ( 'NONE',  ( 151.7948205124835681, 51.78348778862537927, 4.785054706298732086 ) ) ;
#18031 = CARTESIAN_POINT ( 'NONE',  ( 130.8568914410475372, -24.07718906447255947, 24.07718906447199458 ) ) ;
#18032 = CARTESIAN_POINT ( 'NONE',  ( 5.823571940252923795, 49.16771748719391155, -14.15488761396722239 ) ) ;
#18033 = CARTESIAN_POINT ( 'NONE',  ( 192.4448373802101173, -20.00000000003938538, 40.00000000000002132 ) ) ;
#18034 = ORIENTED_EDGE ( 'NONE', *, *, #21663, .F. ) ;
#18035 = CARTESIAN_POINT ( 'NONE',  ( 23.37394308801977871, -23.33966569535037294, -42.85717664514612579 ) ) ;
#18036 = CARTESIAN_POINT ( 'NONE',  ( -10.17115291714076619, 40.74322563957075971, 16.87639663473746410 ) ) ;
#18037 = CARTESIAN_POINT ( 'NONE',  ( 200.0000000000000284, -82.49999999999990052, 52.49999999999977973 ) ) ;
#18038 = DIRECTION ( 'NONE',  ( 0.000000000000000000, 1.000000000000000000, 0.000000000000000000 ) ) ;
#18039 = ORIENTED_EDGE ( 'NONE', *, *, #7502, .T. ) ;
#18040 = CARTESIAN_POINT ( 'NONE',  ( -188.4701769959780790, -43.05504096897843880, 23.48627020870801374 ) ) ;
#18041 = CARTESIAN_POINT ( 'NONE',  ( 199.9999999999998579, -17.68075590865577951, 6.990562776172230208 ) ) ;
#18042 = CARTESIAN_POINT ( 'NONE',  ( 20.91285618074430275, -13.92631245144835539, 47.65039156503490148 ) ) ;
#18043 = EDGE_CURVE ( 'NONE', #22478, #12165, #12445, .T. ) ;
#18044 = AXIS2_PLACEMENT_3D ( 'NONE', #21550, #7427, #23300 ) ;
#18045 = CARTESIAN_POINT ( 'NONE',  ( 23.36927571439206375, 23.34061495561077137, -42.85861222363617884 ) ) ;
#18046 = CARTESIAN_POINT ( 'NONE',  ( 199.0191706476670959, -17.79509468669765226, -9.138050845474172235 ) ) ;
#18047 = EDGE_CURVE ( 'NONE', #2455, #19714, #18113, .T. ) ;
#18048 = CARTESIAN_POINT ( 'NONE',  ( 158.3379117892986585, -26.51167085133963397, 10.98149362779608396 ) ) ;
#18049 = CARTESIAN_POINT ( 'NONE',  ( -109.1264249741462748, 13.72187187126471386, -33.12752917268139896 ) ) ;
#18050 = CARTESIAN_POINT ( 'NONE',  ( -100.7734535825088500, 40.53558337403654832, 16.03295912088756481 ) ) ;
#18051 = CARTESIAN_POINT ( 'NONE',  ( 192.4448373802101173, -19.99999999996057554, 40.00000000000002132 ) ) ;
#18052 = VECTOR ( 'NONE', #7898, 1000.000000000000000 ) ;
#18053 = CIRCLE ( 'NONE', #1934, 5.000000000000004441 ) ;
#18055 = CARTESIAN_POINT ( 'NONE',  ( 14.38125909742180220, 39.01709431150892016, 17.55144818341517166 ) ) ;
#18054 = CARTESIAN_POINT ( 'NONE',  ( -188.9524938556052689, 13.86227398173258329, -47.22059665005700424 ) ) ;
#18056 = CARTESIAN_POINT ( 'NONE',  ( 98.29820294267527458, 2.689882573189819553E-13, -20.00000000000500222 ) ) ;
#18057 = CARTESIAN_POINT ( 'NONE',  ( -208.1127848780264742, -15.00245453012673202, -40.00000000000002132 ) ) ;
#18058 = CARTESIAN_POINT ( 'NONE',  ( -238.4067589809705794, 0.9644942799825385604, 40.00000000000002132 ) ) ;
#18059 = CARTESIAN_POINT ( 'NONE',  ( -238.4067589809705794, -39.99999999999963762, -40.96449428006383187 ) ) ;
#18060 = CARTESIAN_POINT ( 'NONE',  ( 130.8568914410475088, -24.07718906446910623, 32.49135343045471558 ) ) ;
#18061 = CARTESIAN_POINT ( 'NONE',  ( 98.29820294267423719, -14.14213562374330024, 14.14213562372619926 ) ) ;
#18062 = CARTESIAN_POINT ( 'NONE',  ( 98.38705101653206953, -18.51031735812086865, -7.667224493555860221 ) ) ;
#18063 = ORIENTED_EDGE ( 'NONE', *, *, #21741, .T. ) ;
#18064 = CARTESIAN_POINT ( 'NONE',  ( 91.82158438592158234, -12.16597498397761967, -12.16597498397768007 ) ) ;
#18065 = CARTESIAN_POINT ( 'NONE',  ( 91.82158438592158234, 17.20528682183301683, 0.000000000000000000 ) ) ;
#18066 = CARTESIAN_POINT ( 'NONE',  ( -210.0000000000000284, 0.000000000000000000, 0.000000000000000000 ) ) ;
#18067 = ITEM_DEFINED_TRANSFORMATION ( 'NONE', 'NONE', #16793,  #21058 ) ;
#18068 = EDGE_LOOP ( 'NONE', ( #5455, #21425 ) ) ;
#18069 = ORIENTED_EDGE ( 'NONE', *, *, #20361, .T. ) ;
#18070 = CARTESIAN_POINT ( 'NONE',  ( -30.26275506840322294, -57.76657404653985139, 1.198031551615709844 ) ) ;
#18071 = CARTESIAN_POINT ( 'NONE',  ( 22.95085416411756540, -43.12496437194769783, -17.86294511971837551 ) ) ;
#18072 = VERTEX_POINT ( 'NONE', #13177 ) ;
#18073 = CARTESIAN_POINT ( 'NONE',  ( -135.8532207217289738, 30.84685318188643777, -40.00000000000002132 ) ) ;
#18074 = CARTESIAN_POINT ( 'NONE',  ( 200.0000000000000000, 71.50000000000009948, -66.50000000000005684 ) ) ;
#18075 = ORIENTED_EDGE ( 'NONE', *, *, #3001, .T. ) ;
#18076 = CARTESIAN_POINT ( 'NONE',  ( 200.0000000000000568, 7.542793502284206753, 17.44923311141863920 ) ) ;
#18077 = AXIS2_PLACEMENT_3D ( 'NONE', #21156, #4803, #12905 ) ;
#18078 = DIRECTION ( 'NONE',  ( -0.3301743753981520868, 0.9439199552030034246, 0.000000000000000000 ) ) ;
#18079 = CARTESIAN_POINT ( 'NONE',  ( -30.26275506840325136, 29.48230279907798135, -27.08623969584585112 ) ) ;
#18080 = CARTESIAN_POINT ( 'NONE',  ( -188.2871287166307184, -46.98614659774644053, -13.82723289751385387 ) ) ;
#18081 = ADVANCED_FACE ( 'NONE', ( #21298 ), #3073, .F. ) ;
#18082 = CARTESIAN_POINT ( 'NONE',  ( 4.995406935893305089, -40.00000000000021316, 55.24977328853194791 ) ) ;
#18083 = CARTESIAN_POINT ( 'NONE',  ( 57.59792236341147031, -2.435789363418150000, 40.00000000000002132 ) ) ;
#18084 = CARTESIAN_POINT ( 'NONE',  ( -91.56559293963834989, -16.03295912088659492, -40.53558337403696044 ) ) ;
#18085 = CARTESIAN_POINT ( 'NONE',  ( 199.0231121918538975, 0.6363371645724309467, 19.99606429142543362 ) ) ;
#18086 = AXIS2_PLACEMENT_3D ( 'NONE', #440, #2709, #8544 ) ;
#18087 = CARTESIAN_POINT ( 'NONE',  ( -198.0356074513804572, -9.007331120208026888E-14, 15.37879056873070560 ) ) ;
#18088 = CARTESIAN_POINT ( 'NONE',  ( 200.0000000000000000, -40.00000000000019185, 19.99999999999968381 ) ) ;
#18089 = CARTESIAN_POINT ( 'NONE',  ( -114.4364955367315559, -8.644468109196942862, 20.04994829328090589 ) ) ;
#18090 = CARTESIAN_POINT ( 'NONE',  ( 146.6084372240433709, -32.08495691632041513, -24.48358557860343154 ) ) ;
#18091 = EDGE_CURVE ( 'NONE', #15298, #2818, #21747, .T. ) ;
#18092 = CARTESIAN_POINT ( 'NONE',  ( -56.48582580120559271, 9.153146818113576444, -0.000000000000000000 ) ) ;
#18093 = EDGE_CURVE ( 'NONE', #4362, #20612, #21966, .T. ) ;
#18094 = CARTESIAN_POINT ( 'NONE',  ( 151.7948205124835681, -4.785054706298153882, -51.78348778862540058 ) ) ;
#18095 = DIRECTION ( 'NONE',  ( -1.000000000000000000, 1.836970198721030181E-16, 0.000000000000000000 ) ) ;
#18096 = CARTESIAN_POINT ( 'NONE',  ( 0.4289713102705806080, -48.32239598606154374, 14.02712011273581894 ) ) ;
#18097 = CARTESIAN_POINT ( 'NONE',  ( -192.9588430854690273, 40.00000000000014211, -14.46834944099927966 ) ) ;
#18098 = CARTESIAN_POINT ( 'NONE',  ( 170.2234770963711128, 1.169953928977015745E-13, -24.55285855007187124 ) ) ;
#18099 = CARTESIAN_POINT ( 'NONE',  ( 4.995406935893283773, 39.06748935135195211, -17.50105314357185193 ) ) ;
#18100 = CARTESIAN_POINT ( 'NONE',  ( -30.26275506840324070, -1.198031551616016266, -1.198031551616031587 ) ) ;
#18101 = CARTESIAN_POINT ( 'NONE',  ( -187.7699188115114737, -23.34606611632339579, -42.84915433765043957 ) ) ;
#18102 = ORIENTED_EDGE ( 'NONE', *, *, #6961, .F. ) ;
#18103 = CARTESIAN_POINT ( 'NONE',  ( 163.1118516004056573, -19.27778845539181063, -37.29075403953176959 ) ) ;
#18104 = LINE ( 'NONE', #24375, #6343 ) ;
#18105 = CARTESIAN_POINT ( 'NONE',  ( 4.995406935893293543, -15.24977328854832592, 0.000000000000000000 ) ) ;
#18106 = SURFACE_STYLE_FILL_AREA ( #17836 ) ;
#18107 = CARTESIAN_POINT ( 'NONE',  ( 163.1118516004056573, -47.56205970284945295, -9.006482792074823607 ) ) ;
#18108 = CARTESIAN_POINT ( 'NONE',  ( -626.9846540392142060, 75.00000000000000000, -60.00000000000000000 ) ) ;
#18109 = VERTEX_POINT ( 'NONE', #5573 ) ;
#18110 = CARTESIAN_POINT ( 'NONE',  ( 199.9999999999999432, 18.69211761857796361, 3.422848245100247766 ) ) ;
#18111 = CARTESIAN_POINT ( 'NONE',  ( 200.0000000000000000, -59.99999999999992895, 0.000000000000000000 ) ) ;
#18112 = CARTESIAN_POINT ( 'NONE',  ( -8.720657192108735245, 22.53512351407145431, 41.62108041046444384 ) ) ;
#18113 = CIRCLE ( 'NONE', #6639, 21.53474504356805852 ) ;
#18114 = ORIENTED_EDGE ( 'NONE', *, *, #3781, .F. ) ;
#18115 = ORIENTED_EDGE ( 'NONE', *, *, #6472, .F. ) ;
#18116 = CARTESIAN_POINT ( 'NONE',  ( 57.59792236341147031, -2.435789363418150444, 0.000000000000000000 ) ) ;
#18117 = CARTESIAN_POINT ( 'NONE',  ( 199.0097193260481561, -3.097360908056462137, -19.75623422735097989 ) ) ;
#18118 = CARTESIAN_POINT ( 'NONE',  ( -114.7826396786541778, -1.385196341758722305, -22.13135001983572536 ) ) ;
#18119 = CARTESIAN_POINT ( 'NONE',  ( -280.0000000000000000, -14.14213562373098831, -14.14213562373098654 ) ) ;
#18120 = CARTESIAN_POINT ( 'NONE',  ( -93.01854144617588815, -8.553566904151914230, -20.65013722626880366 ) ) ;
#18121 = CARTESIAN_POINT ( 'NONE',  ( -208.1127848780264742, 40.00000000000014211, -15.00245453012627728 ) ) ;
#18122 = FACE_OUTER_BOUND ( 'NONE', #23919, .T. ) ;
#18123 = LINE ( 'NONE', #1910, #12167 ) ;
#18124 = DIRECTION ( 'NONE',  ( 1.000000000000000000, -1.836970198721030181E-16, -0.000000000000000000 ) ) ;
#18125 = CARTESIAN_POINT ( 'NONE',  ( 199.0163148259956358, 13.65645126726637670, 14.61284818176725331 ) ) ;
#18126 = CARTESIAN_POINT ( 'NONE',  ( -179.7979154981486545, 40.14328926550173549, 16.62789485202968365 ) ) ;
#18127 = B_SPLINE_CURVE_WITH_KNOTS ( 'NONE', 3,
 ( #15729, #23854, #5632, #7235, #13739, #21865, #3252, #13237 ),
 .UNSPECIFIED., .F., .F.,
 ( 4, 2, 2, 4 ),
 ( 0.0002291728420353419319, 0.002290361214525118462, 0.004351549587014895588, 0.008473926331994447239 ),
 .UNSPECIFIED. ) ;
#18128 = CARTESIAN_POINT ( 'NONE',  ( -3.439026802539704164, -17.93765581402000109, -43.30533194338906355 ) ) ;
#18129 = CARTESIAN_POINT ( 'NONE',  ( 151.7948205124836534, -33.06932595376376582, 23.49921654115996006 ) ) ;
#18130 = CIRCLE ( 'NONE', #24076, 14.99999999999999822 ) ;
#18131 = CARTESIAN_POINT ( 'NONE',  ( -110.0961830519565012, 2.516413774691878658, -20.07657871247701209 ) ) ;
#18132 = CARTESIAN_POINT ( 'NONE',  ( -162.0762913951020892, -57.76657433524000851, 1.198031840315820329 ) ) ;
#18133 = CARTESIAN_POINT ( 'NONE',  ( 0.2972598230769957217, 1.502051041545559470E-13, -14.33493731733933352 ) ) ;
#18134 = DIRECTION ( 'NONE',  ( 0.000000000000000000, 0.000000000000000000, 1.000000000000000000 ) ) ;
#18135 = CARTESIAN_POINT ( 'NONE',  ( -238.4067589809705510, -40.96449427998265946, -2.449293598294708485E-15 ) ) ;
#18136 = CARTESIAN_POINT ( 'NONE',  ( 146.6084372240433993, 24.48358557860341733, -24.48358557860313311 ) ) ;
#18137 = AXIS2_PLACEMENT_3D ( 'NONE', #13154, #25145, #15269 ) ;
#18138 = CARTESIAN_POINT ( 'NONE',  ( -86.96347745069644475, -18.24025645688354302, -2.449293598294708485E-15 ) ) ;
#18139 = CARTESIAN_POINT ( 'NONE',  ( -110.0799678180788135, 10.89276344593376500, 16.99803934748214118 ) ) ;
#18140 = CARTESIAN_POINT ( 'NONE',  ( -208.1127848780264742, 40.00000000000014211, -15.00245453012627728 ) ) ;
#18141 = CARTESIAN_POINT ( 'NONE',  ( 136.1360204305621266, -24.77266263493116583, -24.77266263493127951 ) ) ;
#18142 = CARTESIAN_POINT ( 'NONE',  ( 91.82158438592158234, -17.20528682183298486, -40.00000000000002132 ) ) ;
#18143 = ORIENTED_EDGE ( 'NONE', *, *, #9630, .T. ) ;
#18144 = ORIENTED_EDGE ( 'NONE', *, *, #3151, .F. ) ;
#18145 = CARTESIAN_POINT ( 'NONE',  ( -192.9588430854689989, 14.46834944099965981, 0.000000000000000000 ) ) ;
#18146 = CARTESIAN_POINT ( 'NONE',  ( -30.26275506840323359, -40.00000000000017053, 41.69427246844613677 ) ) ;
#18147 = CARTESIAN_POINT ( 'NONE',  ( 19.06497207195980792, 10.03556273973447155, -10.03556273973422286 ) ) ;
#18148 = CYLINDRICAL_SURFACE ( 'NONE', #21115, 74.99999999999995737 ) ;
#18149 = B_SPLINE_CURVE_WITH_KNOTS ( 'NONE', 3,
 ( #13562, #3334, #23936, #7191, #9706, #17811 ),
 .UNSPECIFIED., .F., .F.,
 ( 4, 2, 4 ),
 ( 0.000000000000000000, 0.004090195167846852331, 0.008180390335693704662 ),
 .UNSPECIFIED. ) ;
#18150 = CARTESIAN_POINT ( 'NONE',  ( -126.6834156230570443, -9.107266674891850045, -24.89646324314895409 ) ) ;
#18151 = FACE_OUTER_BOUND ( 'NONE', #21047, .T. ) ;
#18152 = CARTESIAN_POINT ( 'NONE',  ( 200.0000000000000284, 17.23849352212496910, 7.999418879479941680 ) ) ;
#18153 = B_SPLINE_CURVE_WITH_KNOTS ( 'NONE', 3,
 ( #14671, #12953, #2855, #8559, #10963, #8827, #2444, #10556, #16541, #16674, #22937, #23200, #18808, #588 ),
 .UNSPECIFIED., .F., .F.,
 ( 4, 2, 2, 2, 2, 2, 4 ),
 ( 1.040834085586084257E-17, 0.002941681445496942097, 0.004412522168245415315, 0.005883362890993887664, 0.008825044336490834099, 0.01029588505923930211, 0.01176672578198776839 ),
 .UNSPECIFIED. ) ;
#18154 = CARTESIAN_POINT ( 'NONE',  ( 199.9999999999999147, -18.75789134796499624, 3.098008012732793137 ) ) ;
#18155 = CARTESIAN_POINT ( 'NONE',  ( 192.4448373802101173, 42.42640687116487896, 14.14213562375934075 ) ) ;
#18156 = CARTESIAN_POINT ( 'NONE',  ( -162.0762913951020607, -57.76657433537922515, -1.198031840455874963 ) ) ;
#18157 = EDGE_CURVE ( 'NONE', #21974, #24779, #11951, .T. ) ;
#18158 = CARTESIAN_POINT ( 'NONE',  ( -105.5018569248037323, 19.60236078713514729, 8.316028620552629036 ) ) ;
#18159 = CARTESIAN_POINT ( 'NONE',  ( -162.0762913951020892, -1.202636532414034422E-14, -1.694272876828323948 ) ) ;
#18160 = CARTESIAN_POINT ( 'NONE',  ( 0.2972598230770027716, -38.42060263243681817, 18.14793986248684377 ) ) ;
#18161 = CARTESIAN_POINT ( 'NONE',  ( -162.0762913951020892, 1.198031840385732849, -1.198031840385733515 ) ) ;
#18162 = CARTESIAN_POINT ( 'NONE',  ( 151.7948205124836534, -23.49921654115981084, -33.06932595376387951 ) ) ;
#18163 = CARTESIAN_POINT ( 'NONE',  ( -86.96347745069644475, 15.38646221621793586, -15.38646221621778842 ) ) ;
#18164 = CARTESIAN_POINT ( 'NONE',  ( 199.0255398360378365, -7.415439759742569414, 18.57980843913382429 ) ) ;
#18166 = CARTESIAN_POINT ( 'NONE',  ( -91.56559293963836410, 39.99999999999994316, 17.32597176626825330 ) ) ;
#18165 = CARTESIAN_POINT ( 'NONE',  ( -192.9588430854689989, 38.51493924976983152, -38.51493924976893624 ) ) ;
#18167 = CARTESIAN_POINT ( 'NONE',  ( -105.3755690713226727, -15.38646221621807619, 15.38646221621768362 ) ) ;
#18168 = CARTESIAN_POINT ( 'NONE',  ( 21.80824205441142638, 43.30754100652377758, -23.67346680102637890 ) ) ;
#18169 = CARTESIAN_POINT ( 'NONE',  ( -162.0762913951020892, 41.69427287692678163, -40.00000000000002132 ) ) ;
#18170 = ORIENTED_EDGE ( 'NONE', *, *, #24602, .F. ) ;
#18171 = CARTESIAN_POINT ( 'NONE',  ( 136.1360204305621266, -24.77266263493116583, -24.77266263493127951 ) ) ;
#18172 = CARTESIAN_POINT ( 'NONE',  ( -6.342283169553549982, -42.32555349774968789, 23.00001740814397877 ) ) ;
#18173 = CARTESIAN_POINT ( 'NONE',  ( -198.0356074513804572, 15.37879056873066830, 40.00000000000002132 ) ) ;
#18174 = VERTEX_POINT ( 'NONE', #13545 ) ;
#18175 = CARTESIAN_POINT ( 'NONE',  ( -192.1963514251026481, -48.17613439256447094, 14.00508311691324259 ) ) ;
#18176 = CARTESIAN_POINT ( 'NONE',  ( 199.9999999999999716, -17.31617203886849410, 7.850475485701642775 ) ) ;
#18177 = CARTESIAN_POINT ( 'NONE',  ( -3.696864809820544995, -13.84627154338493682, 47.11278487914830038 ) ) ;
#18178 = EDGE_CURVE ( 'NONE', #7956, #17450, #20935, .T. ) ;
#18179 = CARTESIAN_POINT ( 'NONE',  ( 22.81400246987433178, 17.87890238636472517, -43.16348862150605470 ) ) ;
#18180 = CARTESIAN_POINT ( 'NONE',  ( 199.0138211924391385, -10.98290011267725141, -16.71408225681557980 ) ) ;
#18181 = CARTESIAN_POINT ( 'NONE',  ( 155.1206158682455509, -27.79897307351034286, 11.51471166709224825 ) ) ;
#18182 = DIRECTION ( 'NONE',  ( 0.7071067811865476838, 0.7071067811865474617, 0.000000000000000000 ) ) ;
#18183 = CARTESIAN_POINT ( 'NONE',  ( 130.8568914410475372, 4.207082182992923691, -4.207082182992794017 ) ) ;
#18184 = CARTESIAN_POINT ( 'NONE',  ( -56.48582580120559271, 9.153146818113576444, -0.000000000000000000 ) ) ;
#18185 = CARTESIAN_POINT ( 'NONE',  ( -192.6563370915689575, 18.27409561807029093, -44.11756948121943367 ) ) ;
#18186 = DIRECTION ( 'NONE',  ( -3.936061032557131542E-17, 0.2142691827715860198, 0.9767746502210203907 ) ) ;
#18187 = CARTESIAN_POINT ( 'NONE',  ( -198.0356074513804572, -55.37879056871328487, -40.00000000000002132 ) ) ;
#18188 = CARTESIAN_POINT ( 'NONE',  ( 0.2972598230769930017, 54.33493731733936016, 40.00000000000002132 ) ) ;
#18189 = CARTESIAN_POINT ( 'NONE',  ( 184.8905102610680444, 40.00000000000025580, -19.07866798485515503 ) ) ;
#18190 = CARTESIAN_POINT ( 'NONE',  ( -91.56559293963834989, 40.53558337403677569, -16.03295912088699993 ) ) ;
#18191 = DIRECTION ( 'NONE',  ( -1.000000000000000000, 1.836970198721030181E-16, 0.000000000000000000 ) ) ;
#18192 = DIRECTION ( 'NONE',  ( 1.000000000000000000, 1.836970198721030181E-16, 0.000000000000000000 ) ) ;
#18193 = ORIENTED_EDGE ( 'NONE', *, *, #1482, .F. ) ;
#18194 = CARTESIAN_POINT ( 'NONE',  ( -192.9588430854690273, -18.05360324515454096, 38.51493924976936967 ) ) ;
#18195 = CARTESIAN_POINT ( 'NONE',  ( -102.4309680866550849, -8.733065090091864491, 20.17061239836789355 ) ) ;
#18196 = ORIENTED_EDGE ( 'NONE', *, *, #20013, .T. ) ;
#18197 = EDGE_LOOP ( 'NONE', ( #14609, #24917 ) ) ;
#18198 = CARTESIAN_POINT ( 'NONE',  ( 192.4448373802101173, -14.14213562370283128, -42.42640687122081999 ) ) ;
#18199 = CARTESIAN_POINT ( 'NONE',  ( 22.70429368897839595, -43.19357487035075849, -17.89136451867676314 ) ) ;
#18200 = ORIENTED_EDGE ( 'NONE', *, *, #17112, .F. ) ;
#18201 = CARTESIAN_POINT ( 'NONE',  ( -213.1075012329537230, 13.71589010951907994, 0.000000000000000000 ) ) ;
#18202 = CARTESIAN_POINT ( 'NONE',  ( -99.31364972218746345, -20.48028939129060078, 8.933506367463246889 ) ) ;
#18203 = CIRCLE ( 'NONE', #19484, 10.00000000000000888 ) ;
#18204 = EDGE_LOOP ( 'NONE', ( #21342, #12487, #17801, #24282 ) ) ;
#18205 = CARTESIAN_POINT ( 'NONE',  ( 200.0000000000002558, 14.28373528157942829, 12.54030857537068755 ) ) ;
#18206 = CYLINDRICAL_SURFACE ( 'NONE', #1340, 9.999999999999998224 ) ;
#18207 = CARTESIAN_POINT ( 'NONE',  ( 57.59792236341147031, 26.56190807104693619, -30.00663442387692115 ) ) ;
#18208 = CARTESIAN_POINT ( 'NONE',  ( -151.4802930571904085, -33.96623840872754130, -11.09498731354133660 ) ) ;
#18209 = CARTESIAN_POINT ( 'NONE',  ( 136.1360204305621551, -39.99999999999987921, -35.03383547441310242 ) ) ;
#18210 = CARTESIAN_POINT ( 'NONE',  ( -280.0000000000000568, -20.00000000000006750, 40.00000000000002132 ) ) ;
#18211 = CARTESIAN_POINT ( 'NONE',  ( 192.4448373802101173, -14.14213562375826605, -42.42640687116518450 ) ) ;
#18212 = CARTESIAN_POINT ( 'NONE',  ( 199.0260893535204048, -10.43036187021208860, 17.07141274968551059 ) ) ;
#18213 = CARTESIAN_POINT ( 'NONE',  ( 0.2972598230770030492, -40.00000000000007816, 14.33493731733919496 ) ) ;
#18214 = CARTESIAN_POINT ( 'NONE',  ( -192.9588430854690273, -40.00000000000024158, 54.46834944101708231 ) ) ;
#18215 = CARTESIAN_POINT ( 'NONE',  ( -30.26275506840324070, -40.00000000000001421, -1.694272468446678559 ) ) ;
#18216 = CARTESIAN_POINT ( 'NONE',  ( -162.0762913951020892, -3.568845385355699554E-14, 1.694272876828323948 ) ) ;
#18217 = CARTESIAN_POINT ( 'NONE',  ( 192.4448373802100889, 20.00000000003945644, 0.000000000000000000 ) ) ;
#18218 = CARTESIAN_POINT ( 'NONE',  ( -238.4067589809705794, -28.96627169325343942, 28.96627169325309126 ) ) ;
#18219 = CARTESIAN_POINT ( 'NONE',  ( -162.0762913951021176, -1.694272876828353702, -40.00000000000002132 ) ) ;
#18220 = CARTESIAN_POINT ( 'NONE',  ( -100.7734535825088500, -40.53558337403669753, -16.03295912088728770 ) ) ;
#18221 = FACE_BOUND ( 'NONE', #21874, .T. ) ;
#18222 = CARTESIAN_POINT ( 'NONE',  ( 23.23834162556334348, -46.85950693572758041, 13.80856396598941593 ) ) ;
#18223 = CARTESIAN_POINT ( 'NONE',  ( -162.0762913951020892, -1.202636532414034422E-14, -1.694272876828323948 ) ) ;
#18224 = CARTESIAN_POINT ( 'NONE',  ( -105.3755690713226727, -8.549198663894545631E-14, 18.24025645688352881 ) ) ;
#18225 = CARTESIAN_POINT ( 'NONE',  ( -91.56559293963834989, 40.53558337403677569, -16.03295912088699993 ) ) ;
#18226 = PLANE ( 'NONE',  #21533 ) ;
#18227 = CARTESIAN_POINT ( 'NONE',  ( -189.6939645179852789, -18.01965094556722136, -43.50328570201967437 ) ) ;
#18228 = CARTESIAN_POINT ( 'NONE',  ( -208.1127848780264742, -38.89260858015728672, -17.67593391476669851 ) ) ;
#18229 = EDGE_LOOP ( 'NONE', ( #25236, #15542, #18772, #15712 ) ) ;
#18230 = AXIS2_PLACEMENT_3D ( 'NONE', #16061, #12075, #10217 ) ;
#18231 = CARTESIAN_POINT ( 'NONE',  ( 130.8568914410475372, -24.07718906447255947, 24.07718906447199458 ) ) ;
#18232 = DIRECTION ( 'NONE',  ( 0.000000000000000000, -1.000000000000000000, 0.000000000000000000 ) ) ;
#18233 = DIRECTION ( 'NONE',  ( 0.000000000000000000, -1.000000000000000000, 0.000000000000000000 ) ) ;
#18234 = ADVANCED_FACE ( 'NONE', ( #5311, #25675 ), #15536, .F. ) ;
#18235 = DIRECTION ( 'NONE',  ( 0.000000000000000000, 1.000000000000000000, 0.000000000000000000 ) ) ;
#18236 = CARTESIAN_POINT ( 'NONE',  ( -162.0762913951021176, -27.08623940707584055, -29.48230308784799547 ) ) ;
#18237 = SHAPE_REPRESENTATION_RELATIONSHIP ( 'NONE' , 'NONE' ,  #15720, #21994 ) ;
#18238 = CARTESIAN_POINT ( 'NONE',  ( -77.61595200903278169, 3.459815247513496228, 21.80829238165218698 ) ) ;
#18239 = ORIENTED_EDGE ( 'NONE', *, *, #13997, .T. ) ;
#18240 = CARTESIAN_POINT ( 'NONE',  ( 199.9999999999998863, 18.97030179798468907, 1.258860953597385590 ) ) ;
#18241 = DIRECTION ( 'NONE',  ( -1.000000000000000000, -1.836970198721030181E-16, 0.000000000000000000 ) ) ;
#18242 = CARTESIAN_POINT ( 'NONE',  ( -1.087763065929284290, 24.03018639663618927, 43.78960619332443116 ) ) ;
#18243 = EDGE_CURVE ( 'NONE', #1858, #2889, #12113, .T. ) ;
#18244 = EDGE_LOOP ( 'NONE', ( #15338, #13714, #23088, #21488 ) ) ;
#18245 = ORIENTED_EDGE ( 'NONE', *, *, #20785, .F. ) ;
#18246 = CARTESIAN_POINT ( 'NONE',  ( -351.0000000000000568, -4.857225732735059864E-14, 0.000000000000000000 ) ) ;
#18247 = CARTESIAN_POINT ( 'NONE',  ( 199.0140770886559949, -11.39180206020552788, -16.43826011434489587 ) ) ;
#18248 = DIRECTION ( 'NONE',  ( -1.000000000000000000, 1.836970198721030181E-16, 0.000000000000000000 ) ) ;
#18249 = EDGE_CURVE ( 'NONE', #19453, #19106, #17915, .T. ) ;
#18250 = ADVANCED_FACE ( 'NONE', ( #1203 ), #3319, .F. ) ;
#18251 = CARTESIAN_POINT ( 'NONE',  ( -91.56559293963834989, -16.03295912088706388, -16.03295912088710651 ) ) ;
#18252 = CARTESIAN_POINT ( 'NONE',  ( -97.73860346107333896, -8.987542150753291992, -20.56359266933904451 ) ) ;
#18253 = CIRCLE ( 'NONE', #21652, 15.00000000000000178 ) ;
#18254 = CARTESIAN_POINT ( 'NONE',  ( 14.38125909742180220, 40.00000000000017764, -15.17850393972591760 ) ) ;
#18255 = CARTESIAN_POINT ( 'NONE',  ( 199.9999999999996589, -18.76526504493254777, 3.099636891498418478 ) ) ;
#18256 = CARTESIAN_POINT ( 'NONE',  ( -188.2995950289364089, 46.99046209955525200, -13.82811170417133617 ) ) ;
#18257 = CARTESIAN_POINT ( 'NONE',  ( -105.4741150117389168, 7.943527260764259523, 19.77569912954497866 ) ) ;
#18258 = CARTESIAN_POINT ( 'NONE',  ( 199.0227319893622848, 1.617020328492027259, 19.94056979940310015 ) ) ;
#18259 = CARTESIAN_POINT ( 'NONE',  ( -199.0572111222995488, 43.66164585888754601, 18.08524587028139052 ) ) ;
#18260 = CARTESIAN_POINT ( 'NONE',  ( 11.38508063392463043, -14.17561098846331191, -49.30460303390994170 ) ) ;
#18261 = CARTESIAN_POINT ( 'NONE',  ( -192.9588430854689705, -38.51493924976909966, -38.51493924976973915 ) ) ;
#18262 = CARTESIAN_POINT ( 'NONE',  ( -96.93773665438781961, 20.58457565566406799, -9.001171854902132452 ) ) ;
#18263 = CARTESIAN_POINT ( 'NONE',  ( 130.8568914410475088, -32.49135343045460900, -24.07718906446924478 ) ) ;
#18264 = CARTESIAN_POINT ( 'NONE',  ( -210.0000000000000284, -1.836970198721030378E-15, 0.000000000000000000 ) ) ;
#18265 = FACE_BOUND ( 'NONE', #8431, .T. ) ;
#18266 = CARTESIAN_POINT ( 'NONE',  ( 184.8905102610680444, -19.07866798485555293, -2.449293598294708485E-15 ) ) ;
#18267 = DIRECTION ( 'NONE',  ( 0.000000000000000000, -0.000000000000000000, 1.000000000000000000 ) ) ;
#18268 = CARTESIAN_POINT ( 'NONE',  ( -238.4067589809705510, -40.96449427998265946, -2.449293598294708485E-15 ) ) ;
#18269 = DIRECTION ( 'NONE',  ( 0.000000000000000000, 1.000000000000000000, 0.000000000000000000 ) ) ;
#18270 = CARTESIAN_POINT ( 'NONE',  ( -238.4067589809705794, 40.00000000000040501, -40.96449427990138759 ) ) ;
#18271 = CARTESIAN_POINT ( 'NONE',  ( -91.56559293963834989, -16.03295912088706388, -16.03295912088710651 ) ) ;
#18272 = CARTESIAN_POINT ( 'NONE',  ( 146.6084372240433993, -34.62501878078303008, 0.000000000000000000 ) ) ;
#18273 = ORIENTED_EDGE ( 'NONE', *, *, #18926, .F. ) ;
#18274=STYLED_ITEM('',(#26374),#25811);
#18275 = ORIENTED_EDGE ( 'NONE', *, *, #17291, .T. ) ;
#18276 = ORIENTED_EDGE ( 'NONE', *, *, #5393, .T. ) ;
#18277 = CARTESIAN_POINT ( 'NONE',  ( 91.82158438592158234, -17.20528682183298486, 40.00000000000002132 ) ) ;
#18278 = CARTESIAN_POINT ( 'NONE',  ( -89.92902785008678279, -8.088236460649998349, -20.44110050034134929 ) ) ;
#18279 = CARTESIAN_POINT ( 'NONE',  ( -192.9588430854689989, -2.280704836619014309E-13, 54.46834944099972375 ) ) ;
#18280 = CARTESIAN_POINT ( 'NONE',  ( 163.1118516004056573, 37.29075403953132906, 19.27778845539275565 ) ) ;
#18281 = CARTESIAN_POINT ( 'NONE',  ( -105.3755690713226727, -21.75974354311652093, 0.000000000000000000 ) ) ;
#18282 = CYLINDRICAL_SURFACE ( 'NONE', #8747, 5.000000000000004441 ) ;
#18283 = CARTESIAN_POINT ( 'NONE',  ( -362.0709805440841365, -4.857225732735059864E-14, 28.79780246617542616 ) ) ;
#18284 = CARTESIAN_POINT ( 'NONE',  ( 200.0000000000000000, 15.44098642598172866, 11.08330662512073950 ) ) ;
#18285 = CARTESIAN_POINT ( 'NONE',  ( 199.9999999999999147, -15.72534676981639201, 10.68315640806297040 ) ) ;
#18286 = CARTESIAN_POINT ( 'NONE',  ( 151.7948205124836534, 33.06932595376333239, 23.49921654116065284 ) ) ;
#18287 = CARTESIAN_POINT ( 'NONE',  ( -105.3755690713226585, -12.89780903124444578, 43.67073346367968156 ) ) ;
#18288 = CARTESIAN_POINT ( 'NONE',  ( 200.0000000000000000, -61.50000000000001421, -66.50000000000005684 ) ) ;
#18289 = CARTESIAN_POINT ( 'NONE',  ( -87.11138134861613480, 17.02212146152260885, -13.16760794720424776 ) ) ;
#18290 = CARTESIAN_POINT ( 'NONE',  ( -135.8532207217289738, -21.81201906317806305, 34.75652343174590442 ) ) ;
#18291 = CARTESIAN_POINT ( 'NONE',  ( -86.95488169845621940, 9.644899311048764190, -19.11867441905801357 ) ) ;
#18292 = CARTESIAN_POINT ( 'NONE',  ( -259.2033419157646676, -35.01439189186554302, 21.55415060305832498 ) ) ;
#18293 = CARTESIAN_POINT ( 'NONE',  ( -213.1075012329537230, -37.98287015391232302, -18.58567234101164800 ) ) ;
#18294 = CARTESIAN_POINT ( 'NONE',  ( 199.0196953583521520, 8.175823868318582655, 18.25500783319687415 ) ) ;
#18296 = CARTESIAN_POINT ( 'NONE',  ( 4.995406935893298872, -1.944352046434030652E-13, 55.24977328854835434 ) ) ;
#18295 = CARTESIAN_POINT ( 'NONE',  ( 91.82158438592158234, 44.40256751092319121, 12.16597498400105515 ) ) ;
#18297 = CARTESIAN_POINT ( 'NONE',  ( -30.26275506840325136, 57.76657404653985139, -1.198031551615314161 ) ) ;
#18298 = CARTESIAN_POINT ( 'NONE',  ( 23.37583784646131235, 42.85659535397685005, -23.33923448557672131 ) ) ;
#18299 = CARTESIAN_POINT ( 'NONE',  ( -100.7734535825088500, 17.32597176626809699, -40.00000000000002132 ) ) ;
#18300 = ORIENTED_EDGE ( 'NONE', *, *, #23402, .F. ) ;
#18301 = CARTESIAN_POINT ( 'NONE',  ( -135.8532207217289738, -9.153146818113595984, 0.000000000000000000 ) ) ;
#18302 = CARTESIAN_POINT ( 'NONE',  ( -4.915070467873723814, -42.74707758271747338, 23.27857837409242947 ) ) ;
#18303 = CIRCLE ( 'NONE', #7671, 5.000000000000011546 ) ;
#18304 = CARTESIAN_POINT ( 'NONE',  ( -198.0356074513804572, 55.37879056873070027, 2.449293598294708485E-15 ) ) ;
#18305 = ORIENTED_EDGE ( 'NONE', *, *, #11113, .F. ) ;
#18306 = CARTESIAN_POINT ( 'NONE',  ( -1.255560987024282094, 23.98612781107801695, -43.73013506549182949 ) ) ;
#18307 = CIRCLE ( 'NONE', #24273, 14.99999999999999645 ) ;
#18308 = VECTOR ( 'NONE', #2578, 1000.000000000000000 ) ;
#18309 = CIRCLE ( 'NONE', #19589, 31.79780246617542616 ) ;
#18310 = AXIS2_PLACEMENT_3D ( 'NONE', #22494, #404, #16495 ) ;
#18311 = CARTESIAN_POINT ( 'NONE',  ( 199.9999999999998863, -16.91159699891635171, 8.687942971654136315 ) ) ;
#18312 = CARTESIAN_POINT ( 'NONE',  ( -3.786831587087432727, -23.50387725152155838, 43.07879808621821383 ) ) ;
#18313 = CARTESIAN_POINT ( 'NONE',  ( -3.443169733045677194, 17.93724492941721493, -43.30433998020576780 ) ) ;
#18314 = CARTESIAN_POINT ( 'NONE',  ( 199.0078712948245823, 1.622169390422157242, -19.93073376281416031 ) ) ;
#18315 = CARTESIAN_POINT ( 'NONE',  ( 57.59792236341147031, -1.493297263419786540E-14, 2.435789363418160658 ) ) ;
#18316 = CARTESIAN_POINT ( 'NONE',  ( 155.4809970915717372, -27.66446758342042500, 11.45899766888341986 ) ) ;
#18317 = CARTESIAN_POINT ( 'NONE',  ( -151.4802930564399901, -16.17241674337392254, 31.86309827659608018 ) ) ;
#18318 = CARTESIAN_POINT ( 'NONE',  ( 57.59792236341147031, 26.56190807104720975, -26.56190807104655249 ) ) ;
#18319 = CARTESIAN_POINT ( 'NONE',  ( -105.2054292635175017, 14.23158570600623385, -16.16441072139837232 ) ) ;
#18320 = AXIS2_PLACEMENT_3D ( 'NONE', #11032, #14614, #13029 ) ;
#18322 = CARTESIAN_POINT ( 'NONE',  ( -208.1127848780264742, 38.89260858015707356, 17.67593391476696141 ) ) ;
#18321 = CARTESIAN_POINT ( 'NONE',  ( -188.6013942376037278, 13.84412886956844169, -47.09843442133356461 ) ) ;
#18323 = CARTESIAN_POINT ( 'NONE',  ( -208.1127848780264742, 67.17687982763172272, -10.60833733270698254 ) ) ;
#18324 = EDGE_CURVE ( 'NONE', #1209, #25810, #530, .T. ) ;
#18325 = CARTESIAN_POINT ( 'NONE',  ( -208.1127848780264742, -55.00245453010926866, 40.00000000000002132 ) ) ;
#18326 = CARTESIAN_POINT ( 'NONE',  ( -213.1075012329537230, 53.71589010950162191, -40.00000000000002132 ) ) ;
#18327 = CARTESIAN_POINT ( 'NONE',  ( -86.96347745069644475, -2.438961472018186339E-13, 21.75974354311649961 ) ) ;
#18328 = CARTESIAN_POINT ( 'NONE',  ( 57.59792236341147031, -1.722363176415123043, 54.84617931850879557 ) ) ;
#18329 = CARTESIAN_POINT ( 'NONE',  ( -105.4741150117379647, 19.77569912955136999, -7.943527260750081531 ) ) ;
#18330 = CARTESIAN_POINT ( 'NONE',  ( 192.4448373802100889, -14.14213562370293431, -14.14213562370322030 ) ) ;
#18331 = EDGE_CURVE ( 'NONE', #22608, #20012, #18347, .T. ) ;
#18332 = ORIENTED_EDGE ( 'NONE', *, *, #869, .F. ) ;
#18333 = CARTESIAN_POINT ( 'NONE',  ( 130.8568914410475372, -24.07718906447222551, -24.07718906447233209 ) ) ;
#18334 = B_SPLINE_CURVE_WITH_KNOTS ( 'NONE', 3,
 ( #21884, #25891, #7508, #12037, #24148, #17615 ),
 .UNSPECIFIED., .F., .F.,
 ( 4, 2, 4 ),
 ( -6.000000003830536561E-08, 0.03937727993095203882, 0.07875461986190411545 ),
 .UNSPECIFIED. ) ;
#18335 = CARTESIAN_POINT ( 'NONE',  ( -99.31364972220134746, 8.933506367370242174, 20.48028939132513315 ) ) ;
#18336 = ORIENTED_EDGE ( 'NONE', *, *, #14853, .T. ) ;
#18337 = VERTEX_POINT ( 'NONE', #21673 ) ;
#18338 = CARTESIAN_POINT ( 'NONE',  ( -105.3755690713226585, -12.89780903124383471, -43.67073346367985920 ) ) ;
#18339 = CARTESIAN_POINT ( 'NONE',  ( 22.01478053669594814, -43.25192662396801069, -23.63228119971946839 ) ) ;
#18340 = EDGE_CURVE ( 'NONE', #17033, #25214, #9019, .T. ) ;
#18341 = VERTEX_POINT ( 'NONE', #19667 ) ;
#18342 = CARTESIAN_POINT ( 'NONE',  ( 23.37394308801978582, -46.80823611210187352, -13.80096434448294396 ) ) ;
#18343 = CARTESIAN_POINT ( 'NONE',  ( -105.3844866140388206, -9.640326247891781719, -19.12039797534664132 ) ) ;
#18345 = ORIENTED_EDGE ( 'NONE', *, *, #13952, .T. ) ;
#18344 = EDGE_CURVE ( 'NONE', #20782, #16811, #24470, .T. ) ;
#18346 = CARTESIAN_POINT ( 'NONE',  ( 199.9999999999998579, 17.43084440603007224, 7.570815656493459223 ) ) ;
#18347 = CIRCLE ( 'NONE', #1381, 10.00000000000004796 ) ;
#18348 = DIRECTION ( 'NONE',  ( 0.000000000000000000, 0.9767746502210202797, -0.2142691827715865471 ) ) ;
#18349 = CARTESIAN_POINT ( 'NONE',  ( -56.48582580120559982, 21.81201906317778594, -34.75652343174606074 ) ) ;
#18350 = CARTESIAN_POINT ( 'NONE',  ( -189.0115661350367873, -43.33404204260303061, -17.94954792649186004 ) ) ;
#18351 = CARTESIAN_POINT ( 'NONE',  ( -213.1075012329537230, -40.00000000000011369, 13.71589010951897691 ) ) ;
#18352 = CARTESIAN_POINT ( 'NONE',  ( -105.3755690713226727, -21.75974354311652093, 0.000000000000000000 ) ) ;
#18353 = CARTESIAN_POINT ( 'NONE',  ( -198.0356074513804572, 10.87444709761036066, -67.44298959253325165 ) ) ;
#18354 = CARTESIAN_POINT ( 'NONE',  ( 199.0252416244725282, -6.134786337322394090, 19.04345623536530141 ) ) ;
#18355 =( REPRESENTATION_RELATIONSHIP ('NONE','NONE', #23888, #12169 ) REPRESENTATION_RELATIONSHIP_WITH_TRANSFORMATION ( #13804 )SHAPE_REPRESENTATION_RELATIONSHIP( ) );
#18356 = CARTESIAN_POINT ( 'NONE',  ( 151.7948205124836534, -39.99999999999987921, -33.23291073765567916 ) ) ;
#18357 = CARTESIAN_POINT ( 'NONE',  ( -86.96347745069644475, -8.210974027862429531E-14, 18.24025645688352881 ) ) ;
#18358 = CARTESIAN_POINT ( 'NONE',  ( -86.96347745069644475, 5.999880687339585546E-14, -21.75974354311649961 ) ) ;
#18359 = CARTESIAN_POINT ( 'NONE',  ( -56.48582580120559982, 9.153146818113574668, -40.00000000000002132 ) ) ;
#18360 = CARTESIAN_POINT ( 'NONE',  ( 192.4448373802101173, -42.42640687116490028, -14.14213562375904942 ) ) ;
#18361 = CARTESIAN_POINT ( 'NONE',  ( 0.2972598230769983307, -14.33493731733933352, 0.000000000000000000 ) ) ;
#18362 = CARTESIAN_POINT ( 'NONE',  ( 57.59792236341148453, -26.56190807104700369, 26.56190807104673723 ) ) ;
#18363 = DIRECTION ( 'NONE',  ( 0.000000000000000000, -0.6739498806388349861, -0.7387770694782697101 ) ) ;
#18364 = CARTESIAN_POINT ( 'NONE',  ( 20.59573805978979522, -47.74081960064684438, 13.93986955483953594 ) ) ;
#18365 = CARTESIAN_POINT ( 'NONE',  ( -86.96347745069645896, 40.00000000000019895, -18.24025645688310249 ) ) ;
#18366 = CARTESIAN_POINT ( 'NONE',  ( 136.1360204305621551, -40.00000000000001421, 4.966164525586921563 ) ) ;
#18367 = CARTESIAN_POINT ( 'NONE',  ( 192.4448373802101173, 42.42640687116508502, -14.14213562375874567 ) ) ;
#18368 = AXIS2_PLACEMENT_3D ( 'NONE', #7464, #23702, #13582 ) ;
#18369 = CARTESIAN_POINT ( 'NONE',  ( 57.59792236341147031, 1.722363176415040886, 1.722363176415060426 ) ) ;
#18370 = CARTESIAN_POINT ( 'NONE',  ( -188.3611024622301215, -23.46270902204919651, -43.02327292323010255 ) ) ;
#18371 = CARTESIAN_POINT ( 'NONE',  ( 163.1118516004056573, -37.29075403953139300, -19.27778845539249630 ) ) ;
#18372 = ORIENTED_EDGE ( 'NONE', *, *, #20350, .F. ) ;
#18373 = CARTESIAN_POINT ( 'NONE',  ( 0.2972598230769990524, -18.14793986248671231, -38.42060263243687501 ) ) ;
#18374 = CARTESIAN_POINT ( 'NONE',  ( 200.0000000000000000, -52.49999999999970868, 82.49999999999998579 ) ) ;
#18375 = CARTESIAN_POINT ( 'NONE',  ( -86.96347745069645896, 21.75974354311648895, -40.00000000000002132 ) ) ;
#18376 = DIRECTION ( 'NONE',  ( 0.000000000000000000, 1.000000000000000000, 0.000000000000000000 ) ) ;
#18377 = CARTESIAN_POINT ( 'NONE',  ( 130.8568914410475372, -24.07718906447255947, 24.07718906447199458 ) ) ;
#18378 = ORIENTED_EDGE ( 'NONE', *, *, #12576, .T. ) ;
#18379 = ORIENTED_EDGE ( 'NONE', *, *, #23231, .T. ) ;
#18380 = CARTESIAN_POINT ( 'NONE',  ( 199.9999999999999716, 18.60999626737240931, -3.837347524953120370 ) ) ;
#18381 = DIRECTION ( 'NONE',  ( 0.000000000000000000, -1.000000000000000000, 0.000000000000000000 ) ) ;
#18382 = CARTESIAN_POINT ( 'NONE',  ( -4.439300432588719758, 13.79990882516848849, 46.85201324744569717 ) ) ;
#18383 = ORIENTED_EDGE ( 'NONE', *, *, #5649, .F. ) ;
#18384 = ORIENTED_EDGE ( 'NONE', *, *, #18178, .F. ) ;
#18385 = CARTESIAN_POINT ( 'NONE',  ( 199.0059805750804571, 8.391908656364034158, -18.14947886101857932 ) ) ;
#18386 = CARTESIAN_POINT ( 'NONE',  ( -199.9999999999999716, -82.49999999999991473, -52.49999999999977973 ) ) ;
#18387 = FILL_AREA_STYLE ('',( #8541 ) ) ;
#18388 = B_SPLINE_CURVE_WITH_KNOTS ( 'NONE', 3,
 ( #5728, #9723, #21700, #3220, #1230, #1360, #3346, #9459, #17320, #25454, #7205, #15694, #1483, #9588, #7712, #11446 ),
 .UNSPECIFIED., .F., .F.,
 ( 4, 2, 2, 2, 2, 2, 2, 4 ),
 ( 0.0003146141176167394885, 0.002410294611447383068, 0.003458134858362704993, 0.004505975105278026485, 0.008697336092939303778, 0.01079301658676993375, 0.01288869708060056719, 0.01708005806826183581 ),
 .UNSPECIFIED. ) ;
#18389 = EDGE_CURVE ( 'NONE', #6531, #15177, #7022, .T. ) ;
#18390 = CARTESIAN_POINT ( 'NONE',  ( -2.937533998755706310, 43.32931883109341697, -23.68967259528445979 ) ) ;
#18391 = CARTESIAN_POINT ( 'NONE',  ( -192.9588430854690273, 40.00000000000055422, -54.46834944101679810 ) ) ;
#18392 = DIRECTION ( 'NONE',  ( 0.000000000000000000, -1.000000000000000000, 0.000000000000000000 ) ) ;
#18393 = CARTESIAN_POINT ( 'NONE',  ( -640.4792919554359969, 29.69771861375842192, 26.79787511901963271 ) ) ;
#18394 = CYLINDRICAL_SURFACE ( 'NONE', #20875, 31.79780246617542616 ) ;
#18395 = CARTESIAN_POINT ( 'NONE',  ( 199.0188463327468185, 9.707946089746242180, 17.48826952134088941 ) ) ;
#18396 = CARTESIAN_POINT ( 'NONE',  ( -188.3120147333545731, 23.45203116714302638, 43.00887716025393814 ) ) ;
#18397 = CARTESIAN_POINT ( 'NONE',  ( -3.494657986427937679, -17.93150516116801185, -43.29048295385624101 ) ) ;
#18398 = CARTESIAN_POINT ( 'NONE',  ( 57.59792236341148453, -54.84617931850879557, 1.722363176414566155 ) ) ;
#18399 = CARTESIAN_POINT ( 'NONE',  ( -89.92902785008676858, 20.17328762787298402, -8.734793929541176283 ) ) ;
#18400 = CARTESIAN_POINT ( 'NONE',  ( 200.0000000000000000, -42.42640687119269671, -14.14213562373124766 ) ) ;
#18401 = CARTESIAN_POINT ( 'NONE',  ( -77.62168048241881024, 21.77704146685383790, 3.672512281558228509 ) ) ;
#18402 = CARTESIAN_POINT ( 'NONE',  ( -259.2033419157646676, 6.730120644403426944, 6.730120644403592145 ) ) ;
#18403 = CARTESIAN_POINT ( 'NONE',  ( 91.82158438592159655, -22.79471317813468900, 40.00000000000002132 ) ) ;
#18404 = ADVANCED_FACE ( 'NONE', ( #15414 ), #11528, .T. ) ;
#18405 = LINE ( 'NONE', #16008, #16829 ) ;
#18406 = CARTESIAN_POINT ( 'NONE',  ( -198.0356074513804572, -55.37879056874826489, 40.00000000000002132 ) ) ;
#18407 = CARTESIAN_POINT ( 'NONE',  ( -110.0927810291447599, 16.11098205474433342, 12.17528477497603667 ) ) ;
#18408 = CARTESIAN_POINT ( 'NONE',  ( -135.8532207217289738, 40.00000000000031974, -30.84685318188603986 ) ) ;
#18409 = CARTESIAN_POINT ( 'NONE',  ( -86.96347745069644475, 12.89780903124410472, -43.67073346367977393 ) ) ;
#18410 = CARTESIAN_POINT ( 'NONE',  ( 19.06497207195980792, 14.19242893257840876, 0.000000000000000000 ) ) ;
#18411 = ORIENTED_EDGE ( 'NONE', *, *, #15882, .F. ) ;
#18412 = ORIENTED_EDGE ( 'NONE', *, *, #16141, .F. ) ;
#18413 = ORIENTED_EDGE ( 'NONE', *, *, #15552, .T. ) ;
#18414 = CARTESIAN_POINT ( 'NONE',  ( 4.995406935893288214, 15.24977328854832770, 40.00000000000002132 ) ) ;
#18415 = CARTESIAN_POINT ( 'NONE',  ( 156.5537079553357103, 11.28159757857181766, 27.23618587942438651 ) ) ;
#18416 = CARTESIAN_POINT ( 'NONE',  ( -213.1075012329537230, 66.26714140138673770, -9.698598906462034819 ) ) ;
#18417 = CARTESIAN_POINT ( 'NONE',  ( -110.1018001840315748, -20.19553435163851418, 0.6219992248507131283 ) ) ;
#18418 = PRODUCT_RELATED_PRODUCT_CATEGORY ( 'part', '', ( #13756 ) ) ;
#18419 = FACE_OUTER_BOUND ( 'NONE', #21616, .T. ) ;
#18420 = CARTESIAN_POINT ( 'NONE',  ( -370.0000000000001137, -4.857225732735059864E-14, 0.000000000000000000 ) ) ;
#18421 = CARTESIAN_POINT ( 'NONE',  ( 200.0000000000002274, 18.09557305485218848, -5.802546270622393365 ) ) ;
#18422 = CARTESIAN_POINT ( 'NONE',  ( 199.9999999999999716, -17.68120445620925096, 6.989503635265373660 ) ) ;
#18423 = CARTESIAN_POINT ( 'NONE',  ( -86.96347745069644475, 41.18208027870576871, 15.38646221621837107 ) ) ;
#18424 = CARTESIAN_POINT ( 'NONE',  ( 57.59792236341148453, -26.56190807104663421, -26.56190807104710672 ) ) ;
#18425 = B_SPLINE_CURVE_WITH_KNOTS ( 'NONE', 3,
 ( #12185, #18027, #9921, #2216, #16306, #6196, #4350, #1950, #15893, #18164, #10325, #6322, #2083, #22307, #16170, #12048, #209, #13907, #14043, #5800, #24305, #24430, #24567, #22177, #22041, #6072, #26176, #11918, #7917, #3951, #20306, #4084, #8190, #14174, #80, #10190, #20168, #14443, #20040, #10057, #18294, #5936, #2343, #22572, #16034, #12442, #14309, #4221, #12311, #20438, #18433, #24159, #20570, #7778, #24021, #3814, #1818, #14834, #616, #6722, #10726, #23105, #21103, #15097, #20838, #883, #8993, #6456, #4476, #16570, #2750, #2474, #22966, #18837, #17097, #3007, #4746, #12852, #14571, #14970, #24973, #24701, #22701, #10854, #16701, #8722, #25104, #752, #20708, #2613, #4614, #23230, #5008, #8856, #2883, #24833, #18700, #13113, #16840, #14706, #6853, #10991, #16968, #4877 ),
 .UNSPECIFIED., .F., .F.,
 ( 4, 2, 2, 2, 1, 1, 1, 2, 2, 2, 2, 2, 1, 1, 1, 1, 2, 2, 2, 2, 2, 1, 1, 1, 1, 1, 2, 2, 2, 2, 2, 2, 1, 1, 2, 2, 2, 2, 2, 2, 1, 1, 1, 1, 2, 2, 2, 2, 2, 1, 1, 1, 2, 2, 2, 2, 2, 1, 1, 1, 2, 2, 2, 4 ),
 ( 0.000000000000000000, 0.03124629074579460611, 0.06249258149158921222, 0.06298080478449225028, 0.06346902807739529528, 0.06444547466320135753, 0.06639836783481350979, 0.07030415417803781430, 0.07811572686448636782, 0.09373887223738347485, 0.1249851629831776750, 0.1252292746296291837, 0.1254733862760807062, 0.1259616095689837512, 0.1269380561547898412, 0.1288909493264019657, 0.1327967356696262424, 0.1406083083560747959, 0.1562314537289719030, 0.1874777444747661170, 0.1875998002979918367, 0.1877218561212175840, 0.1879659677676691343, 0.1884541910605721793, 0.1894306376463783248, 0.1913835308179905881, 0.1952893171612150591, 0.2031008898476640012, 0.2187240352205620242, 0.2343471805934600194, 0.2499703259663580701, 0.2509467725521641879, 0.2519232191379703334, 0.2538761123095825689, 0.2577818986528070400, 0.2655934713392559821, 0.2812166167121538107, 0.2968397620850516949, 0.3124629074579495791, 0.3127070191044010739, 0.3129511307508526241, 0.3134393540437556136, 0.3144158006295616481, 0.3163686938011737171, 0.3202744801443978551, 0.3280860528308460755, 0.3437091982037425719, 0.3749554889495356758, 0.3754437122424387208, 0.3759319355353417658, 0.3769083821211477447, 0.3788612752927598137, 0.3827670616359840072, 0.3905786343224322832, 0.4062017796953287796, 0.4374480704411218279, 0.4379362937340248729, 0.4384245170269279179, 0.4394009636127340634, 0.4413538567843462990, 0.4452596431275708810, 0.4530712158140199342, 0.4686943611869179849, 0.4999406519327141418 ),
 .UNSPECIFIED. ) ;
#18426 = DIRECTION ( 'NONE',  ( 1.298934084353256076E-16, -0.7071067811865561215, 0.7071067811865389130 ) ) ;
#18427 = CARTESIAN_POINT ( 'NONE',  ( -30.26275506840325136, 40.00000000000003553, -1.694272468445841007 ) ) ;
#18428 = CARTESIAN_POINT ( 'NONE',  ( -100.7734535825088500, -12.25131212657524316, 44.31723036834888774 ) ) ;
#18429 = CARTESIAN_POINT ( 'NONE',  ( 146.6084372240433993, -24.48358557860353457, 24.48358557860296258 ) ) ;
#18430 = CARTESIAN_POINT ( 'NONE',  ( -238.4067589809705794, -27.60227080167069147, 28.96627169325319429 ) ) ;
#18431 = ADVANCED_FACE ( 'NONE', ( #8087 ), #5876, .T. ) ;
#18432 = CARTESIAN_POINT ( 'NONE',  ( 151.7948205124836250, 23.49921654116361225, -23.49921654116333514 ) ) ;
#18433 = CARTESIAN_POINT ( 'NONE',  ( 199.0159127812860049, 14.20410482617004710, 14.07996899236659871 ) ) ;
#18434 = VECTOR ( 'NONE', #11649, 1000.000000000000000 ) ;
#18436 = CARTESIAN_POINT ( 'NONE',  ( -198.0356074513804572, 39.99999999999979394, 55.37879056874835726 ) ) ;
#18435 = CARTESIAN_POINT ( 'NONE',  ( -30.26275506840323715, 29.48230279907829754, -29.48230279907758344 ) ) ;
#18437 = CARTESIAN_POINT ( 'NONE',  ( -238.4067589809705794, 57.25054294065799354, -0.6820004457334954973 ) ) ;
#18438 = CARTESIAN_POINT ( 'NONE',  ( 20.69615274310878306, 47.71500688527101630, -13.93598092275249911 ) ) ;
#18439 = CARTESIAN_POINT ( 'NONE',  ( -162.0762913951021176, 1.694272876828294194, -40.00000000000002132 ) ) ;
#18440 = CARTESIAN_POINT ( 'NONE',  ( 91.82158438592158234, -12.16597498397761967, -12.16597498397768007 ) ) ;
#18441 = CARTESIAN_POINT ( 'NONE',  ( -4.037857402784076122, -43.00569567200361121, 23.44963359339816122 ) ) ;
#18442 = CARTESIAN_POINT ( 'NONE',  ( -86.96347745069644475, 18.24025645688350750, 40.00000000000002132 ) ) ;
#18443 = ORIENTED_EDGE ( 'NONE', *, *, #12092, .F. ) ;
#18444 = CARTESIAN_POINT ( 'NONE',  ( -1.815588850254805431, 23.89016120430211387, -43.60036197523977108 ) ) ;
#18445 = CARTESIAN_POINT ( 'NONE',  ( 136.1360204305621266, -24.77266263493116583, -24.77266263493127951 ) ) ;
#18446 = CARTESIAN_POINT ( 'NONE',  ( -39.81953879987010936, -11.17638696923166286, 34.34246706546223038 ) ) ;
#18447 = CARTESIAN_POINT ( 'NONE',  ( -3.966425590328896078, 13.83202835294368782, -47.01685867532415131 ) ) ;
#18448 = CARTESIAN_POINT ( 'NONE',  ( 199.0102239786929488, -4.226749394367478097, -19.54603893341629473 ) ) ;
#18449 = CARTESIAN_POINT ( 'NONE',  ( -208.1127848780265026, 1.189126717069624012E-13, -15.00245453012669472 ) ) ;
#18450 = FACE_BOUND ( 'NONE', #6278, .T. ) ;
#18451 = CARTESIAN_POINT ( 'NONE',  ( -188.2871287166134096, -23.44689273421206721, 43.00155302796424905 ) ) ;
#18452 =( BOUNDED_CURVE ( )  B_SPLINE_CURVE ( 3, ( #2113, #16335, #14207, #6230 ),
 .UNSPECIFIED., .F., .F. ) 
 B_SPLINE_CURVE_WITH_KNOTS ( ( 4, 4 ),
 ( 0.01576650722537254259, 0.02368120503278678748 ),
 .UNSPECIFIED. ) 
 CURVE ( )  GEOMETRIC_REPRESENTATION_ITEM ( )  RATIONAL_B_SPLINE_CURVE ( ( 0.7232313460858560417, 0.6666666666666658525, 0.6208516971803444973, 0.5857864376268920870 ) ) 
 REPRESENTATION_ITEM ( '' )  );
#18453 = CARTESIAN_POINT ( 'NONE',  ( -208.1127848780264742, -17.67593391476605547, -38.89260858015755673 ) ) ;
#18454 = CARTESIAN_POINT ( 'NONE',  ( 151.7948205124835681, 33.23291073765556547, 40.00000000000002132 ) ) ;
#18456 = CARTESIAN_POINT ( 'NONE',  ( -238.4067589809705794, 0.6820004457912851592, -0.6820004457913123597 ) ) ;
#18455 = CARTESIAN_POINT ( 'NONE',  ( -188.3066136396993784, 13.82848859481245540, -46.99300418776407895 ) ) ;
#18457 = CARTESIAN_POINT ( 'NONE',  ( -198.0356074513804572, 67.44298959250878056, -10.87444709758402261 ) ) ;
#18458 = CARTESIAN_POINT ( 'NONE',  ( -162.0762913951020607, -41.69427287682838568, -2.449293598294708485E-15 ) ) ;
#18459 = CARTESIAN_POINT ( 'NONE',  ( 57.59792236341147031, 37.56421063658187620, 2.449293598294708485E-15 ) ) ;
#18460 = CARTESIAN_POINT ( 'NONE',  ( -30.26275506840324070, 1.218738420030236455E-14, -1.694272468446259783 ) ) ;
#18461 = CARTESIAN_POINT ( 'NONE',  ( 151.7948205124836250, 4.785054706301690608, 4.785054706301682614 ) ) ;
#18462 = CARTESIAN_POINT ( 'NONE',  ( -97.73860346102681262, 20.56359266934609664, -8.987542150742756419 ) ) ;
#18463 = PRODUCT_DEFINITION_SHAPE ( 'NONE', 'NONE',  #26354 ) ;
#18464 = CARTESIAN_POINT ( 'NONE',  ( -213.1075012329537230, -9.698598906462304825, -66.26714140138675191 ) ) ;
#18465 = CARTESIAN_POINT ( 'NONE',  ( 57.59792236341147031, 30.00663442387683588, 26.56190807104703211 ) ) ;
#18466 = ORIENTED_EDGE ( 'NONE', *, *, #15083, .F. ) ;
#18467 = CARTESIAN_POINT ( 'NONE',  ( -198.0356074513804572, 10.87444709759714989, 10.87444709759722450 ) ) ;
#18468 = CARTESIAN_POINT ( 'NONE',  ( -97.73860346102743790, 8.987542150760905457, 20.56359266933915464 ) ) ;
#18469 = CARTESIAN_POINT ( 'NONE',  ( 0.2972598230770048811, -10.13633138497510089, 66.70487387989852834 ) ) ;
#18470 = CARTESIAN_POINT ( 'NONE',  ( -3.921555385250247827, -47.03297225793160408, -13.83441994316416590 ) ) ;
#18471 = ORIENTED_EDGE ( 'NONE', *, *, #24791, .T. ) ;
#18472 = LINE ( 'NONE', #14747, #17712 ) ;
#18473 = FACE_BOUND ( 'NONE', #12590, .T. ) ;
#18474 = ORIENTED_EDGE ( 'NONE', *, *, #389, .T. ) ;
#18475 = B_SPLINE_CURVE_WITH_KNOTS ( 'NONE', 1,
 ( #17528, #13792 ),
 .UNSPECIFIED., .F., .F.,
 ( 2, 2 ),
 ( 0.000000000000000000, 1.000000000000000000 ),
 .UNSPECIFIED. ) ;
#18476 = CARTESIAN_POINT ( 'NONE',  ( 199.9999999999998010, 4.312122466882670757, -18.50761716938983525 ) ) ;
#18477 = DIRECTION ( 'NONE',  ( -1.000000000000000000, 1.836970198721030181E-16, 0.000000000000000000 ) ) ;
#18478 = CARTESIAN_POINT ( 'NONE',  ( -280.0000000000000000, -14.14213562373098831, -14.14213562373098654 ) ) ;
#18479 = CARTESIAN_POINT ( 'NONE',  ( -166.7090905285257918, -37.06261835962623508, -15.35183918168495332 ) ) ;
#18480 = CARTESIAN_POINT ( 'NONE',  ( 192.4448373802101173, -40.00000000000005684, 19.99999999996046185 ) ) ;
#18481 = CARTESIAN_POINT ( 'NONE',  ( 14.38125909742180752, 55.17850393974265444, 40.00000000000002132 ) ) ;
#18482 = CARTESIAN_POINT ( 'NONE',  ( -213.1075012329537230, 9.698598906450543566, -9.698598906450348167 ) ) ;
#18483 = CARTESIAN_POINT ( 'NONE',  ( 199.0255290512018291, -7.361955815226616906, 18.60363316911454845 ) ) ;
#18484 = CIRCLE ( 'NONE', #26158, 14.99999999999999822 ) ;
#18485 = CARTESIAN_POINT ( 'NONE',  ( -198.0356074513804572, -40.00000000000025580, 55.37879056871310013 ) ) ;
#18486 = CARTESIAN_POINT ( 'NONE',  ( -238.4067589809705794, 39.99999999999983658, 40.96449428006354765 ) ) ;
#18487 = CARTESIAN_POINT ( 'NONE',  ( 57.59792236341146321, 40.00000000000004263, -2.435789363418021214 ) ) ;
#18488 = CARTESIAN_POINT ( 'NONE',  ( 130.8568914410475372, 34.05028731879791337, 0.000000000000000000 ) ) ;
#18489 = CARTESIAN_POINT ( 'NONE',  ( 4.995406935893307754, -55.24977328854835434, -2.449293598294708485E-15 ) ) ;
#18490 = CARTESIAN_POINT ( 'NONE',  ( -259.2033419157646676, 6.730120644403214669, 49.83842185052034068 ) ) ;
#18491 = CARTESIAN_POINT ( 'NONE',  ( 164.1122551457363841, -10.10009781492422576, -24.38379312608499205 ) ) ;
#18492 = ADVANCED_FACE ( 'NONE', ( #20048 ), #20314, .F. ) ;
#18493 = FACE_BOUND ( 'NONE', #4526, .T. ) ;
#18494 = CARTESIAN_POINT ( 'NONE',  ( 130.8568914410475372, 8.880724697947696879E-14, -5.949712681206690945 ) ) ;
#18495 = CARTESIAN_POINT ( 'NONE',  ( 170.2234770963711128, -2.511315425431857630E-14, 15.44714144992816074 ) ) ;
#18496 = CARTESIAN_POINT ( 'NONE',  ( -280.0000000000000568, 14.14213562373097943, -42.42640687119285303 ) ) ;
#18497 = DIRECTION ( 'NONE',  ( -1.000000000000000000, -1.836970198721030181E-16, -0.000000000000000000 ) ) ;
#18498 = DIRECTION ( 'NONE',  ( 1.000000000000000000, 1.836970198721030427E-16, -0.000000000000000000 ) ) ;
#18499 = CARTESIAN_POINT ( 'NONE',  ( 184.8905102610680444, -41.77492675555986779, -14.79361573936407304 ) ) ;
#18500 = ORIENTED_EDGE ( 'NONE', *, *, #6380, .T. ) ;
#18501 = CARTESIAN_POINT ( 'NONE',  ( 170.2234770963711128, -45.64576402573167258, -10.92277846919254891 ) ) ;
#18502 = LINE ( 'NONE', #22515, #15693 ) ;
#18503 = CARTESIAN_POINT ( 'NONE',  ( -100.7734535825088500, -17.32597176626812185, -40.00000000000002132 ) ) ;
#18504 = CARTESIAN_POINT ( 'NONE',  ( -114.4364955367335881, -20.04994829326802019, 8.644468109231409514 ) ) ;
#18505 = CARTESIAN_POINT ( 'NONE',  ( -280.0000000000000000, -20.00000000000006750, 0.000000000000000000 ) ) ;
#18506 =( NAMED_UNIT ( * ) SI_UNIT ( $, .STERADIAN. ) SOLID_ANGLE_UNIT ( ) );
#18507 = EDGE_LOOP ( 'NONE', ( #8759, #4134, #6537, #11333, #18979, #21680, #15180, #13306 ) ) ;
#18508 = AXIS2_PLACEMENT_3D ( 'NONE', #1507, #3365, #7349 ) ;
#18509 = ORIENTED_EDGE ( 'NONE', *, *, #12049, .T. ) ;
#18510 = CIRCLE ( 'NONE', #10002, 5.000000000000004441 ) ;
#18511 = CARTESIAN_POINT ( 'NONE',  ( 199.9999999999999716, 10.29099968577115654, 15.98230674020753206 ) ) ;
#18512 = FACE_OUTER_BOUND ( 'NONE', #4488, .T. ) ;
#18513 = CARTESIAN_POINT ( 'NONE',  ( 22.90311673804424331, 13.82691048574062087, 46.98314248933976245 ) ) ;
#18514 = ORIENTED_EDGE ( 'NONE', *, *, #7837, .F. ) ;
#18515 = VERTEX_POINT ( 'NONE', #9929 ) ;
#18516 = CARTESIAN_POINT ( 'NONE',  ( -135.8532207217289738, -6.472252184284190690, -6.472252184284188914 ) ) ;
#18517 = CARTESIAN_POINT ( 'NONE',  ( 199.0058364129993436, 9.132953877242854901, -17.78802470895853816 ) ) ;
#18518 = CARTESIAN_POINT ( 'NONE',  ( -105.3174652557048603, -5.408042926937029371, -20.76738663211824942 ) ) ;
#18519 = AXIS2_PLACEMENT_3D ( 'NONE', #2463, #69, #10179 ) ;
#18520 = CARTESIAN_POINT ( 'NONE',  ( 23.37394308801976450, 46.80823611210215063, -13.80096434448263309 ) ) ;
#18521 = CIRCLE ( 'NONE', #2809, 74.99999999999991473 ) ;
#18522 = CARTESIAN_POINT ( 'NONE',  ( 151.7948205124836534, 33.06932595376365924, -23.49921654116018743 ) ) ;
#18523 = CARTESIAN_POINT ( 'NONE',  ( -726.9846540392142060, -66.50000000000001421, -61.50000000000006395 ) ) ;
#18524 = CARTESIAN_POINT ( 'NONE',  ( -100.0968563617722822, -8.893120081573353986, -20.41799937588055158 ) ) ;
#18525 = CARTESIAN_POINT ( 'NONE',  ( 192.4448373802101173, 39.99999999999985079, 20.00000000003984013 ) ) ;
#18526 = CARTESIAN_POINT ( 'NONE',  ( -105.3755690713226585, 39.99999999999977263, 21.75974354311691883 ) ) ;
#18527 = CARTESIAN_POINT ( 'NONE',  ( -646.7504686163034648, 33.00883640287656107, 22.64711897480060898 ) ) ;
#18528 = CIRCLE ( 'NONE', #15126, 5.000000000000011546 ) ;
#18529 = DIRECTION ( 'NONE',  ( 0.000000000000000000, 1.000000000000000000, 0.000000000000000000 ) ) ;
#18530 = CARTESIAN_POINT ( 'NONE',  ( 199.0053384867209445, 15.04244419640346031, -13.18878631234924192 ) ) ;
#18531 = CARTESIAN_POINT ( 'NONE',  ( -192.1963514250885225, 14.00508311691534047, 48.17613439255790553 ) ) ;
#18532 = CARTESIAN_POINT ( 'NONE',  ( 146.6084372240433709, -3.800685668859084210, 52.76785682606516303 ) ) ;
#18533 = CARTESIAN_POINT ( 'NONE',  ( -199.9999999999998863, 23.83166235904700514, 44.86667451853053734 ) ) ;
#18534 = CARTESIAN_POINT ( 'NONE',  ( 14.38125909742180752, 17.55144818341448953, 39.01709431150923280 ) ) ;
#18535 = CARTESIAN_POINT ( 'NONE',  ( 190.0000000000000000, -35.78896085774753288, 1.496915739050593134E-14 ) ) ;
#18536 = CARTESIAN_POINT ( 'NONE',  ( 4.995406935893287326, 17.50105314357225694, -39.06748935135176026 ) ) ;
#18537 = CARTESIAN_POINT ( 'NONE',  ( -657.0617608586776441, 41.27766484936599056, 18.03718546295864655 ) ) ;
#18538 = CARTESIAN_POINT ( 'NONE',  ( -30.26275506840324425, -1.694272468446265334, 40.00000000000002132 ) ) ;
#18539=STYLED_ITEM('',(#26409),#17642);
#18540 = CARTESIAN_POINT ( 'NONE',  ( 136.1360204305621266, 24.77266263493138965, -24.77266263493110188 ) ) ;
#18541 = CARTESIAN_POINT ( 'NONE',  ( 19.06497207195980792, -14.19242893257839988, 40.00000000000002132 ) ) ;
#18542 = CARTESIAN_POINT ( 'NONE',  ( -114.7719828131935600, 16.76092671198274076, 14.45533796058303899 ) ) ;
#18543 = CARTESIAN_POINT ( 'NONE',  ( -100.7734535825088500, 39.99999999999976552, 22.67402823373233645 ) ) ;
#18544 = CARTESIAN_POINT ( 'NONE',  ( 14.38125909742180752, 10.73282306404720465, 10.73282306404724018 ) ) ;
#18545 = CARTESIAN_POINT ( 'NONE',  ( -726.9846540392142060, -66.50000000000001421, -71.50000000000005684 ) ) ;
#18546 = ORIENTED_EDGE ( 'NONE', *, *, #9075, .T. ) ;
#18547 = VERTEX_POINT ( 'NONE', #10331 ) ;
#18548 = VERTEX_POINT ( 'NONE', #20577 ) ;
#18549 = CARTESIAN_POINT ( 'NONE',  ( -30.26275506840324425, 1.694272468446254232, 40.00000000000002132 ) ) ;
#18550 = CIRCLE ( 'NONE', #8769, 5.000000000000039080 ) ;
#18551 = CARTESIAN_POINT ( 'NONE',  ( 144.9504669809064978, 12.48392651407807108, 30.13886470195712164 ) ) ;
#18552 = CARTESIAN_POINT ( 'NONE',  ( -192.9588430854689989, 38.51493924976983152, -38.51493924976893624 ) ) ;
#18553 = CARTESIAN_POINT ( 'NONE',  ( -351.0000000000000568, -4.605747634845933236E-14, 20.53474504356812247 ) ) ;
#18554 = VECTOR ( 'NONE', #15317, 1000.000000000000000 ) ;
#18555 = AXIS2_PLACEMENT_3D ( 'NONE', #7711, #14236, #7 ) ;
#18556 = CARTESIAN_POINT ( 'NONE',  ( 192.4448373802100889, -20.00000000003938538, 0.000000000000000000 ) ) ;
#18557 = CARTESIAN_POINT ( 'NONE',  ( -87.10563802237732034, 2.725721811608155853, -21.31096006044499802 ) ) ;
#18558 = CARTESIAN_POINT ( 'NONE',  ( 200.0000000000002558, 2.008769787671115026, -18.89534854373681938 ) ) ;
#18559 = CARTESIAN_POINT ( 'NONE',  ( 199.9999999999999432, 6.970163742134758422, -17.67854661859792031 ) ) ;
#18560 = CARTESIAN_POINT ( 'NONE',  ( -238.4067589809705794, 0.6820004458491113475, -57.25054294077229144 ) ) ;
#18561 = CARTESIAN_POINT ( 'NONE',  ( -86.96347745069643054, -41.18208027870611687, 15.38646221621750954 ) ) ;
#18562 = CARTESIAN_POINT ( 'NONE',  ( -210.0000000000000284, 9.184850993605148733E-15, 75.00000000000000000 ) ) ;
#18563 = CARTESIAN_POINT ( 'NONE',  ( -135.8532207217289738, 39.99999999999990763, 9.153146818113990335 ) ) ;
#18564 = CARTESIAN_POINT ( 'NONE',  ( 57.59792236341148453, -54.84617931850879557, 1.722363176414566155 ) ) ;
#18565 = CARTESIAN_POINT ( 'NONE',  ( 4.995406935893293543, -15.24977328854832592, 0.000000000000000000 ) ) ;
#18566 = CARTESIAN_POINT ( 'NONE',  ( -135.8532207217289738, -6.472252184284190690, -6.472252184284188914 ) ) ;
#18567 = CARTESIAN_POINT ( 'NONE',  ( 200.0000000000000000, -14.14213562373062949, -42.42640687119301646 ) ) ;
#18568 = DIRECTION ( 'NONE',  ( 0.000000000000000000, 1.000000000000000000, 0.000000000000000000 ) ) ;
#18570 = CARTESIAN_POINT ( 'NONE',  ( -198.0356074513804572, -2.321818583541004323E-13, 55.37879056873073580 ) ) ;
#18569 = CARTESIAN_POINT ( 'NONE',  ( 163.1118516004056573, 37.29075403953132906, 19.27778845539275565 ) ) ;
#18571 = CARTESIAN_POINT ( 'NONE',  ( 200.0000000000000000, 14.14213562373041455, 42.42640687119311593 ) ) ;
#18572 = CARTESIAN_POINT ( 'NONE',  ( 27.55177309528054863, 41.56868263114863282, -22.48880744266877940 ) ) ;
#18573 = CARTESIAN_POINT ( 'NONE',  ( 19.06497207195980792, 54.19242893257844429, -40.00000000000002132 ) ) ;
#18574 = CARTESIAN_POINT ( 'NONE',  ( 170.2234770963711128, 24.55285855007190321, 0.000000000000000000 ) ) ;
#18575 = VECTOR ( 'NONE', #2072, 1000.000000000000000 ) ;
#18576 = EDGE_CURVE ( 'NONE', #10807, #24743, #19687, .T. ) ;
#18577 = CARTESIAN_POINT ( 'NONE',  ( -4.260882601032464301, -46.91379881627281634, 13.81249720866922281 ) ) ;
#18578 = CARTESIAN_POINT ( 'NONE',  ( 57.59792236341147031, 37.56421063658187620, 40.00000000000002132 ) ) ;
#18579 = ADVANCED_FACE ( 'NONE', ( #16042 ), #7037, .T. ) ;
#18580 = VERTEX_POINT ( 'NONE', #18545 ) ;
#18581 = DIRECTION ( 'NONE',  ( 0.000000000000000000, 1.000000000000000000, 0.000000000000000000 ) ) ;
#18582 = VECTOR ( 'NONE', #20319, 1000.000000000000000 ) ;
#18583 = CARTESIAN_POINT ( 'NONE',  ( -77.71213746886081708, 19.08763273111125258, 11.02205165069162973 ) ) ;
#18584 = FACE_OUTER_BOUND ( 'NONE', #6889, .T. ) ;
#18585 = EDGE_CURVE ( 'NONE', #14740, #23424, #8970, .T. ) ;
#18586 = EDGE_CURVE ( 'NONE', #22454, #12932, #20952, .T. ) ;
#18587 = CARTESIAN_POINT ( 'NONE',  ( -4.151555265633122715, 13.82020782288901728, -46.95165237383025669 ) ) ;
#18588 = CARTESIAN_POINT ( 'NONE',  ( 199.0140770886559949, -11.39180206020552788, -16.43826011434489587 ) ) ;
#18589 = CARTESIAN_POINT ( 'NONE',  ( -87.12809909135488340, -21.45715697399372957, 1.359879344826744774 ) ) ;
#18590 = CARTESIAN_POINT ( 'NONE',  ( -86.95493927446865712, 6.698173996907309302, 20.33927854521555290 ) ) ;
#18591 = CARTESIAN_POINT ( 'NONE',  ( -192.9370379451644055, -24.26711011076518787, 44.11033005022603959 ) ) ;
#18592 = CARTESIAN_POINT ( 'NONE',  ( -162.0762913951021176, -27.08623940707584055, -29.48230308784799547 ) ) ;
#18593 = CARTESIAN_POINT ( 'NONE',  ( -105.3220005116024112, 10.86457728909803144, -18.46446237098378518 ) ) ;
#18595 = CARTESIAN_POINT ( 'NONE',  ( 91.82158438592158234, 16.11829626348378142, 40.45024623143977749 ) ) ;
#18594 = CARTESIAN_POINT ( 'NONE',  ( -188.8842637254077488, 17.93596642850458522, -43.30125340596324435 ) ) ;
#18596 = CARTESIAN_POINT ( 'NONE',  ( 192.4448373802101173, 14.14213562370261279, 42.42640687122091236 ) ) ;
#18597 = CARTESIAN_POINT ( 'NONE',  ( -259.2033419157646676, -30.48217210827744239, -2.449293598294708485E-15 ) ) ;
#18598 = CARTESIAN_POINT ( 'NONE',  ( 130.8568914410475372, 5.949712681206715814, 2.449293598294708485E-15 ) ) ;
#18599 = CARTESIAN_POINT ( 'NONE',  ( -91.56559293963834989, -40.00000000000027711, 22.67402823373149801 ) ) ;
#18600 = CARTESIAN_POINT ( 'NONE',  ( -30.26275506840323715, 29.48230279907789253, 29.48230279907799556 ) ) ;
#18601 = CARTESIAN_POINT ( 'NONE',  ( -93.01854144614533482, 20.65013722618569147, -8.553566904202646981 ) ) ;
#18602 = CARTESIAN_POINT ( 'NONE',  ( 91.82158438592159655, 12.16597498400091304, -44.40256751092321963 ) ) ;
#18603 = CARTESIAN_POINT ( 'NONE',  ( 4.995406935893293543, -10.78321810389005364, 10.78321810388994173 ) ) ;
#18604 = ORIENTED_EDGE ( 'NONE', *, *, #1492, .F. ) ;
#18605 = CARTESIAN_POINT ( 'NONE',  ( -135.8532207217289738, -34.75652343174615311, 21.81201906317767936 ) ) ;
#18606 = CARTESIAN_POINT ( 'NONE',  ( -105.4741150117390021, 8.366608964593581277, 19.60045294982720776 ) ) ;
#18607 = CARTESIAN_POINT ( 'NONE',  ( -259.2033419157646676, 6.730120644403214669, 49.83842185052034068 ) ) ;
#18608 = CARTESIAN_POINT ( 'NONE',  ( 9.349823541315933184, -44.88994471603697178, -18.59402391556391620 ) ) ;
#18609 = ORIENTED_EDGE ( 'NONE', *, *, #4597, .F. ) ;
#18610 = CARTESIAN_POINT ( 'NONE',  ( 0.2972598230769930572, 14.33493731733933352, 0.000000000000000000 ) ) ;
#18611 = CARTESIAN_POINT ( 'NONE',  ( -87.11181986219450835, -13.17798114315252889, -17.01574595262779610 ) ) ;
#18612 = EDGE_LOOP ( 'NONE', ( #12380, #11959, #17807, #16214 ) ) ;
#18613 = CARTESIAN_POINT ( 'NONE',  ( 200.0000000000000853, 3.093441846007485285, -18.74813587279223981 ) ) ;
#18614 = FACE_OUTER_BOUND ( 'NONE', #19038, .T. ) ;
#18615 = CARTESIAN_POINT ( 'NONE',  ( -190.7346372394673608, -43.65255821758116639, -23.92885340725679555 ) ) ;
#18616 = B_SPLINE_CURVE_WITH_KNOTS ( 'NONE', 3,
 ( #11895, #1663, #23736, #22154, #19744, #9772, #1534, #18009, #10038, #9638, #17740, #7374, #5781, #13887, #20017, #1800, #26154, #16425, #18551, #22290, #14687, #22820, #14158, #6439, #14556, #24284, #20823, #6307, #18415, #22556, #24682, #22687, #8435, #26294 ),
 .UNSPECIFIED., .F., .F.,
 ( 4, 2, 2, 2, 2, 2, 2, 2, 2, 2, 2, 2, 2, 2, 2, 2, 4 ),
 ( -5.298243351207459470E-05, 0.01887868273877534031, 0.02834451532491906456, 0.03071097347145497133, 0.03307743161799088505, 0.03544388976452679529, 0.03781034791106270554, 0.04254326420413452603, 0.04727618049720634652, 0.04964263864374224983, 0.05200909679027816701, 0.05674201308334989730, 0.05910847122988576591, 0.06029170030315365858, 0.06147492937642155819, 0.06620784566949312888, 0.07567367825563638128 ),
 .UNSPECIFIED. ) ;
#18617 =( BOUNDED_SURFACE ( )  B_SPLINE_SURFACE ( 3, 3, ( 
 ( #1714, #5694, #5569, #15925, #13799, #11673, #14208, #17661, #21934, #19665, #3845, #19797, #5834, #26071, #25802, #8085, #9552, #15662, #13675, #24195, #9953, #26213, #16205, #3709, #21797, #11811, #22209, #24337, #20203, #19931 ),
 ( #24058, #3984, #5967, #3570, #9824, #1584, #15792, #9687, #7949, #6101, #22342, #12082, #4119, #17793, #13937, #1983, #25938, #17927, #7809, #22073, #11949, #7680, #20074, #16067, #14078, #20337, #16602, #241, #2652, #12343 ),
 ( #24465, #25004, #10758, #18464, #10489, #8218, #14473, #6757, #18735, #6231, #2510, #20869, #8354, #10223, #2376, #4253, #16336, #518, #20741, #4511, #18602, #12613, #4382, #10624, #8485, #16475, #16734, #8623, #8757, #24866 ),
 ( #24599, #18869, #20472, #650, #6354, #14869, #12474, #22605, #16872, #6620, #23003, #14344, #22474, #20601, #381, #2246, #10353, #24735, #14738, #6491, #22869, #111, #14603, #22732, #12749, #12215, #4646, #2114, #18330, #11267 ),
 ( #9026, #25647, #17130, #9142, #25262, #21138, #3037, #2782, #2913, #21392, #1041, #19261, #5040, #11146, #17257, #1173, #11021, #19131, #913, #13018, #12884, #8889, #25394, #7012, #21000, #11386, #23390, #19386, #25135, #4781 ),
 ( #7145, #19007, #15133, #17000, #15505, #23264, #13146, #21265, #6887, #15261, #5164, #23135, #7393, #10894, #13270, #784, #3165, #4907, #9275, #17383, #15002, #21516, #25522, #7269, #15387, #23510, #5284, #13390, #1293, #3289 ),
 ( #19508, #9400, #17507, #12052, #9925, #21771, #24164, #25908, #3954, #13911, #14047, #3544, #23892, #11514, #7921, #10061, #21640, #1423, #20171, #26314, #15898, #3819, #11644, #9662, #21902, #19767, #20044, #17631, #1954, #1557 ) ),
 .UNSPECIFIED., .T., .F., .F. ) 
 B_SPLINE_SURFACE_WITH_KNOTS ( ( 4, 3, 4 ),
 ( 4, 2, 2, 2, 2, 2, 2, 2, 2, 2, 2, 2, 2, 2, 4 ),
 ( 0.000000000000000000, 0.5000000000000000000, 1.000000000000000000 ),
 ( 0.000000000000000000, 0.1357259735107005372, 0.1651108541090157700, 0.1944957347073310028, 0.3598804999793158710, 0.3867117631979620773, 0.4135430264166082281, 0.5789277916885930964, 0.6062785021374117456, 0.6336292125862302838, 0.8508620842112317728, 0.8814014469398914198, 0.9119408096685510667, 0.9559704048342755334, 1.000000000000000000 ),
 .UNSPECIFIED. ) 
 GEOMETRIC_REPRESENTATION_ITEM ( )  RATIONAL_B_SPLINE_SURFACE ( (
 ( 1.000000000000000000, 1.000000000000000000, 1.000000000000000000, 1.000000000000000000, 1.000000000000000000, 1.000000000000000000, 1.000000000000000000, 1.000000000000000000, 1.000000000000000000, 1.000000000000000000, 1.000000000000000000, 1.000000000000000000, 1.000000000000000000, 1.000000000000000000, 1.000000000000000000, 1.000000000000000000, 1.000000000000000000, 1.000000000000000000, 1.000000000000000000, 1.000000000000000000, 1.000000000000000000, 1.000000000000000000, 1.000000000000000000, 1.000000000000000000, 1.000000000000000000, 1.000000000000000000, 1.000000000000000000, 1.000000000000000000, 1.000000000000000000, 1.000000000000000000),
 ( 0.3333333333333333703, 0.3333333333333333703, 0.3333333333333333703, 0.3333333333333333703, 0.3333333333333333703, 0.3333333333333333703, 0.3333333333333333703, 0.3333333333333333703, 0.3333333333333333703, 0.3333333333333333703, 0.3333333333333333703, 0.3333333333333333703, 0.3333333333333333703, 0.3333333333333333703, 0.3333333333333333703, 0.3333333333333333703, 0.3333333333333333703, 0.3333333333333333703, 0.3333333333333333703, 0.3333333333333333703, 0.3333333333333333703, 0.3333333333333333703, 0.3333333333333333703, 0.3333333333333333703, 0.3333333333333333703, 0.3333333333333333703, 0.3333333333333333703, 0.3333333333333333703, 0.3333333333333333703, 0.3333333333333333703),
 ( 0.3333333333333333703, 0.3333333333333333703, 0.3333333333333333703, 0.3333333333333333703, 0.3333333333333333703, 0.3333333333333333703, 0.3333333333333333703, 0.3333333333333333703, 0.3333333333333333703, 0.3333333333333333703, 0.3333333333333333703, 0.3333333333333333703, 0.3333333333333333703, 0.3333333333333333703, 0.3333333333333333703, 0.3333333333333333703, 0.3333333333333333703, 0.3333333333333333703, 0.3333333333333333703, 0.3333333333333333703, 0.3333333333333333703, 0.3333333333333333703, 0.3333333333333333703, 0.3333333333333333703, 0.3333333333333333703, 0.3333333333333333703, 0.3333333333333333703, 0.3333333333333333703, 0.3333333333333333703, 0.3333333333333333703),
 ( 1.000000000000000000, 1.000000000000000000, 1.000000000000000000, 1.000000000000000000, 1.000000000000000000, 1.000000000000000000, 1.000000000000000000, 1.000000000000000000, 1.000000000000000000, 1.000000000000000000, 1.000000000000000000, 1.000000000000000000, 1.000000000000000000, 1.000000000000000000, 1.000000000000000000, 1.000000000000000000, 1.000000000000000000, 1.000000000000000000, 1.000000000000000000, 1.000000000000000000, 1.000000000000000000, 1.000000000000000000, 1.000000000000000000, 1.000000000000000000, 1.000000000000000000, 1.000000000000000000, 1.000000000000000000, 1.000000000000000000, 1.000000000000000000, 1.000000000000000000),
 ( 0.3333333333333333703, 0.3333333333333333703, 0.3333333333333333703, 0.3333333333333333703, 0.3333333333333333703, 0.3333333333333333703, 0.3333333333333333703, 0.3333333333333333703, 0.3333333333333333703, 0.3333333333333333703, 0.3333333333333333703, 0.3333333333333333703, 0.3333333333333333703, 0.3333333333333333703, 0.3333333333333333703, 0.3333333333333333703, 0.3333333333333333703, 0.3333333333333333703, 0.3333333333333333703, 0.3333333333333333703, 0.3333333333333333703, 0.3333333333333333703, 0.3333333333333333703, 0.3333333333333333703, 0.3333333333333333703, 0.3333333333333333703, 0.3333333333333333703, 0.3333333333333333703, 0.3333333333333333703, 0.3333333333333333703),
 ( 0.3333333333333333703, 0.3333333333333333703, 0.3333333333333333703, 0.3333333333333333703, 0.3333333333333333703, 0.3333333333333333703, 0.3333333333333333703, 0.3333333333333333703, 0.3333333333333333703, 0.3333333333333333703, 0.3333333333333333703, 0.3333333333333333703, 0.3333333333333333703, 0.3333333333333333703, 0.3333333333333333703, 0.3333333333333333703, 0.3333333333333333703, 0.3333333333333333703, 0.3333333333333333703, 0.3333333333333333703, 0.3333333333333333703, 0.3333333333333333703, 0.3333333333333333703, 0.3333333333333333703, 0.3333333333333333703, 0.3333333333333333703, 0.3333333333333333703, 0.3333333333333333703, 0.3333333333333333703, 0.3333333333333333703),
 ( 1.000000000000000000, 1.000000000000000000, 1.000000000000000000, 1.000000000000000000, 1.000000000000000000, 1.000000000000000000, 1.000000000000000000, 1.000000000000000000, 1.000000000000000000, 1.000000000000000000, 1.000000000000000000, 1.000000000000000000, 1.000000000000000000, 1.000000000000000000, 1.000000000000000000, 1.000000000000000000, 1.000000000000000000, 1.000000000000000000, 1.000000000000000000, 1.000000000000000000, 1.000000000000000000, 1.000000000000000000, 1.000000000000000000, 1.000000000000000000, 1.000000000000000000, 1.000000000000000000, 1.000000000000000000, 1.000000000000000000, 1.000000000000000000, 1.000000000000000000) ) ) 
 REPRESENTATION_ITEM ( '' )  SURFACE ( )  );
#18618 = CARTESIAN_POINT ( 'NONE',  ( 14.38125909742181818, -1.924622159709266762E-13, 55.17850393972636880 ) ) ;
#18619 = CARTESIAN_POINT ( 'NONE',  ( -198.0356074513804572, 55.37879056874818673, -40.00000000000002132 ) ) ;
#18620 = CARTESIAN_POINT ( 'NONE',  ( -30.26275506840324070, -27.08623969584554558, -29.48230279907826912 ) ) ;
#18621 = CARTESIAN_POINT ( 'NONE',  ( 199.0248237628271113, -4.554872532684343334, 19.47958378538321611 ) ) ;
#18622 = CARTESIAN_POINT ( 'NONE',  ( 130.8568914410475088, -40.00000000000001421, 5.949712681206549725 ) ) ;
#18623 = CARTESIAN_POINT ( 'NONE',  ( -280.0000000000000000, 1.839446121267387017E-14, -20.00000000000001421 ) ) ;
#18624 = CARTESIAN_POINT ( 'NONE',  ( -200.0000000000000000, 1.308061781956697717E-29, 0.000000000000000000 ) ) ;
#18625 = CARTESIAN_POINT ( 'NONE',  ( -280.0000000000000568, 19.99999999999996092, -40.00000000000002132 ) ) ;
#18626 = CARTESIAN_POINT ( 'NONE',  ( -91.56559293963834989, -17.32597176626812185, -40.00000000000002132 ) ) ;
#18627 = CARTESIAN_POINT ( 'NONE',  ( -162.0762913951021176, 27.08623940707598265, 29.48230308784781428 ) ) ;
#18628 = CARTESIAN_POINT ( 'NONE',  ( 14.38125909742181108, 1.616281842095393922E-13, -15.17850393972633682 ) ) ;
#18629 = CARTESIAN_POINT ( 'NONE',  ( -138.9613193423056146, -13.65853114841830696, 27.95779829447857523 ) ) ;
#18630 = CARTESIAN_POINT ( 'NONE',  ( 151.7948205124836534, 40.00000000000012079, -6.767089262348609857 ) ) ;
#18631 = CARTESIAN_POINT ( 'NONE',  ( 163.1118516004056573, -40.00000000000003553, 12.73709011382460687 ) ) ;
#18632 = CARTESIAN_POINT ( 'NONE',  ( 170.2234770963711128, 10.92277846919210660, -45.64576402573182889 ) ) ;
#18633 = FACE_OUTER_BOUND ( 'NONE', #2287, .T. ) ;
#18634 = CARTESIAN_POINT ( 'NONE',  ( -114.7537493279955214, -13.57142477595643371, 17.50316801954799928 ) ) ;
#18635 = CARTESIAN_POINT ( 'NONE',  ( -192.9588430854689705, -38.51493924976963967, 38.51493924976919914 ) ) ;
#18636 = ORIENTED_EDGE ( 'NONE', *, *, #19706, .F. ) ;
#18637 = CARTESIAN_POINT ( 'NONE',  ( -4.915070467873956517, 42.74707758271757285, -23.27857837409175801 ) ) ;
#18638 = DIRECTION ( 'NONE',  ( 0.000000000000000000, 0.000000000000000000, 1.000000000000000000 ) ) ;
#18639 = CARTESIAN_POINT ( 'NONE',  ( 19.06497207195982924, -54.19242893257843008, -40.00000000000002132 ) ) ;
#18640 = CARTESIAN_POINT ( 'NONE',  ( -87.02160967420090287, -20.76757794971305060, -5.405368517529804073 ) ) ;
#18641 = CARTESIAN_POINT ( 'NONE',  ( -208.1127848780265026, 15.00245453012665564, 0.000000000000000000 ) ) ;
#18642 = ORIENTED_EDGE ( 'NONE', *, *, #1194, .F. ) ;
#18643 = VERTEX_POINT ( 'NONE', #8838 ) ;
#18644 = CARTESIAN_POINT ( 'NONE',  ( 199.9999999999999147, -12.54556961440541585, 14.29646200777123788 ) ) ;
#18645 = CARTESIAN_POINT ( 'NONE',  ( -97.73860346106548036, 8.185503821063067065, -20.89580782303987050 ) ) ;
#18646 = CARTESIAN_POINT ( 'NONE',  ( 12.77879914714818632, 18.55776024549972547, 44.80239647188651020 ) ) ;
#18647 = EDGE_LOOP ( 'NONE', ( #1797, #16047, #419, #15931 ) ) ;
#18648 = ORIENTED_EDGE ( 'NONE', *, *, #5971, .T. ) ;
#18649 = CARTESIAN_POINT ( 'NONE',  ( -192.9588430854690273, 10.23066800231970319, 66.79921049724369198 ) ) ;
#18650 = CARTESIAN_POINT ( 'NONE',  ( 199.0203632001705216, -18.77805633539013996, -6.891912269405206182 ) ) ;
#18651 = LINE ( 'NONE', #8808, #26003 ) ;
#18652 = CARTESIAN_POINT ( 'NONE',  ( -105.3755690713226727, -15.38646221621786481, -15.38646221621789856 ) ) ;
#18653 = EDGE_CURVE ( 'NONE', #6362, #16256, #9858, .T. ) ;
#18654 = DIRECTION ( 'NONE',  ( 1.000000000000000000, 0.000000000000000000, 0.000000000000000000 ) ) ;
#18655 = CARTESIAN_POINT ( 'NONE',  ( 190.0000000000000000, -66.50000000000001421, 66.50000000000005684 ) ) ;
#18656 = CARTESIAN_POINT ( 'NONE',  ( 136.1360204305621551, 40.00000000000009948, -4.966164525586641787 ) ) ;
#18657 = CARTESIAN_POINT ( 'NONE',  ( -259.2033419157646676, 40.00000000000029843, -30.48217210827696988 ) ) ;
#18658 = CARTESIAN_POINT ( 'NONE',  ( -642.9707190394884719, 30.90505122157533435, 25.40327220459336388 ) ) ;
#18659 = DIRECTION ( 'NONE',  ( 1.000000000000000000, -0.000000000000000000, -0.000000000000000000 ) ) ;
#18660 = CARTESIAN_POINT ( 'NONE',  ( 199.0076515966382260, 19.86999350167783263, -2.263549309587763680 ) ) ;
#18661 = CIRCLE ( 'NONE', #22128, 5.000000000000007994 ) ;
#18662 = CARTESIAN_POINT ( 'NONE',  ( -188.9478457324750877, 17.94276812689866674, 43.31767415847477309 ) ) ;
#18663 = CARTESIAN_POINT ( 'NONE',  ( -238.4067589809705794, -28.96627169325352469, 27.60227080167035041 ) ) ;
#18664 = CARTESIAN_POINT ( 'NONE',  ( -86.86493150571116928, 8.366608963953661160, 19.60045294882771572 ) ) ;
#18665 = CARTESIAN_POINT ( 'NONE',  ( 91.82158438592159655, -16.11829626346147393, 16.11829626346132116 ) ) ;
#18666 = DIRECTION ( 'NONE',  ( 1.000000000000000000, 1.836970198721030427E-16, -0.000000000000000000 ) ) ;
#18667 = CARTESIAN_POINT ( 'NONE',  ( 151.7948205124836534, 23.49921654116056047, -33.06932595376338213 ) ) ;
#18668 = CARTESIAN_POINT ( 'NONE',  ( -635.2810310689012567, 29.45439800747776715, 34.02319262537031364 ) ) ;
#18669 = CARTESIAN_POINT ( 'NONE',  ( 146.6084372240433993, 34.62501878078308692, 0.000000000000000000 ) ) ;
#18670 = ADVANCED_FACE ( 'NONE', ( #6962 ), #16945, .T. ) ;
#18671 = CARTESIAN_POINT ( 'NONE',  ( -198.0356074513804572, 67.44298959250878056, -10.87444709758402261 ) ) ;
#18672 = CARTESIAN_POINT ( 'NONE',  ( 4.995406935893293543, -15.24977328854832592, 0.000000000000000000 ) ) ;
#18673 = CARTESIAN_POINT ( 'NONE',  ( -592.5938969088034582, 44.52772298657927763, 6.529736744792614900 ) ) ;
#18674 = CARTESIAN_POINT ( 'NONE',  ( -198.0356074513804572, -39.99999999999948130, -55.37879056874863437 ) ) ;
#18675 = CARTESIAN_POINT ( 'NONE',  ( 199.0148543684761080, -12.57771741307266744, -15.55405153308071320 ) ) ;
#18676 = EDGE_CURVE ( 'NONE', #25051, #3040, #23844, .T. ) ;
#18677 = DIRECTION ( 'NONE',  ( 1.000000000000000000, 0.000000000000000000, 0.000000000000000000 ) ) ;
#18678 = B_SPLINE_CURVE_WITH_KNOTS ( 'NONE', 3,
 ( #24898, #16901, #22637, #6264, #24767, #278 ),
 .UNSPECIFIED., .F., .F.,
 ( 4, 2, 4 ),
 ( 1.971482511941758420E-15, 0.03937685683732546071, 0.07875371367464895078 ),
 .UNSPECIFIED. ) ;
#18679 = ORIENTED_EDGE ( 'NONE', *, *, #18722, .T. ) ;
#18680 = VERTEX_POINT ( 'NONE', #2730 ) ;
#18681 = CARTESIAN_POINT ( 'NONE',  ( 19.06497207195980792, 14.19242893257840876, 0.000000000000000000 ) ) ;
#18682 =( LENGTH_UNIT ( ) NAMED_UNIT ( * ) SI_UNIT ( .MILLI., .METRE. ) );
#18683 = EDGE_CURVE ( 'NONE', #3723, #20976, #16665, .T. ) ;
#18684 = CARTESIAN_POINT ( 'NONE',  ( 130.8568914410475372, 4.207082182992923691, -4.207082182992794017 ) ) ;
#18685 = CARTESIAN_POINT ( 'NONE',  ( 90.68848423409737336, 21.28058941648435720, -8.814708753004696362 ) ) ;
#18686 = DIRECTION ( 'NONE',  ( -1.000000000000000000, 0.000000000000000000, 0.000000000000000000 ) ) ;
#18687 = PRODUCT_DEFINITION_SHAPE ( 'NONE', 'NONE',  #26356 ) ;
#18688 = FACE_OUTER_BOUND ( 'NONE', #22915, .T. ) ;
#18689 = CARTESIAN_POINT ( 'NONE',  ( 200.0000000000000284, 8.678546691382686973, -16.90316441639222944 ) ) ;
#18690 = CARTESIAN_POINT ( 'NONE',  ( 199.9999999999999716, 6.098650052811386502, -17.99789284726596961 ) ) ;
#18691 = CARTESIAN_POINT ( 'NONE',  ( 192.4448373802101173, -42.42640687122053578, -14.14213562370360577 ) ) ;
#18692 = CARTESIAN_POINT ( 'NONE',  ( -105.3755690713226727, 15.38646221621771737, 15.38646221621800514 ) ) ;
#18694 = CIRCLE ( 'NONE', #21615, 10.00000000000000000 ) ;
#18693 = CARTESIAN_POINT ( 'NONE',  ( -114.5171371270916296, 20.71058515352653018, 7.156716672343439001 ) ) ;
#18695 = CARTESIAN_POINT ( 'NONE',  ( 14.38125909742180930, 40.00000000000060396, -55.17850393974224232 ) ) ;
#18696 = CARTESIAN_POINT ( 'NONE',  ( -192.9588430854689989, -10.23066800230742501, -10.23066800230756712 ) ) ;
#18697 = CARTESIAN_POINT ( 'NONE',  ( -100.7734535825088500, 22.67402823373189591, -0.000000000000000000 ) ) ;
#18698 = CARTESIAN_POINT ( 'NONE',  ( 146.6084372240433993, -24.48358557860353457, 24.48358557860296258 ) ) ;
#18699 = CARTESIAN_POINT ( 'NONE',  ( -135.8532207217289738, -21.81201906317758343, -34.75652343174620995 ) ) ;
#18700 = CARTESIAN_POINT ( 'NONE',  ( 199.0059807619071535, 18.14866951045441112, -8.393696149220648550 ) ) ;
#18701 = AXIS2_PLACEMENT_3D ( 'NONE', #7465, #9221, #15580 ) ;
#18703 = CARTESIAN_POINT ( 'NONE',  ( -213.1075012329537230, -2.291445344039133686E-13, 53.71589010951915100 ) ) ;
#18702 = CARTESIAN_POINT ( 'NONE',  ( 4.995406935893294431, -17.50105314357144337, -39.06748935135212264 ) ) ;
#18704 = CARTESIAN_POINT ( 'NONE',  ( -91.56559293963834989, 12.25131212657428748, 44.31723036834913643 ) ) ;
#18705 = CARTESIAN_POINT ( 'NONE',  ( 23.36462152323055363, 46.81175967489679834, -13.80148662728979581 ) ) ;
#18706 = CARTESIAN_POINT ( 'NONE',  ( -91.56559293963834989, -22.67402823373193499, -40.00000000000002132 ) ) ;
#18707 = CARTESIAN_POINT ( 'NONE',  ( 192.4448373802100889, -14.14213562375876698, -14.14213562375885047 ) ) ;
#18708 = CARTESIAN_POINT ( 'NONE',  ( -213.1075012329537230, 13.71589010951907817, 40.00000000000002132 ) ) ;
#18709 = CARTESIAN_POINT ( 'NONE',  ( -62.72988123315177944, -25.36777511011030484, 10.50767649784149427 ) ) ;
#18710 = CARTESIAN_POINT ( 'NONE',  ( 184.8905102610680444, 19.07866798485561333, 40.00000000000002132 ) ) ;
#18711 = ORIENTED_EDGE ( 'NONE', *, *, #5910, .F. ) ;
#18712 = CARTESIAN_POINT ( 'NONE',  ( -196.0240701931631691, -48.96019555158521541, -14.12332411430270440 ) ) ;
#18713 = CARTESIAN_POINT ( 'NONE',  ( -3.488770945845345750, -17.93216134257419014, 43.29206711590394008 ) ) ;
#18714 = AXIS2_PLACEMENT_3D ( 'NONE', #2959, #16659, #18792 ) ;
#18715 = CARTESIAN_POINT ( 'NONE',  ( -4.081455915265743251, 17.86600351371890127, -43.13234798823334160 ) ) ;
#18716 = CARTESIAN_POINT ( 'NONE',  ( 199.0250768083106436, -19.24006491846622069, 5.486913247009519878 ) ) ;
#18717 = CARTESIAN_POINT ( 'NONE',  ( 14.38125909742180752, 10.73282306404735387, -10.73282306404708919 ) ) ;
#18718 = CARTESIAN_POINT ( 'NONE',  ( -77.56353172720405098, -22.09247646619704497, 1.385506815421064353 ) ) ;
#18719 = CARTESIAN_POINT ( 'NONE',  ( -4.039451493210478361, -43.00522595893993838, -23.44932283416681429 ) ) ;
#18720 = CARTESIAN_POINT ( 'NONE',  ( -188.9001659262686132, -17.93767091109507916, 43.30536839095043433 ) ) ;
#18721 = CARTESIAN_POINT ( 'NONE',  ( -100.7734535825088500, 16.03295912088691821, 16.03295912088721309 ) ) ;
#18722 = EDGE_CURVE ( 'NONE', #18548, #15169, #19633, .T. ) ;
#18723 = CARTESIAN_POINT ( 'NONE',  ( -135.8532207217289738, -34.75652343174584757, -21.81201906317816253 ) ) ;
#18724 = FACE_OUTER_BOUND ( 'NONE', #19210, .T. ) ;
#18725 =( BOUNDED_SURFACE ( )  B_SPLINE_SURFACE ( 3, 3, ( 
 ( #11138, #21385, #4771, #16992, #906, #508, #22860, #12876, #25386, #1034, #13139, #642, #4637, #9018, #17249, #19254, #17123, #7005, #20992, #12739, #18861, #10750, #16725, #15125, #20859, #6749, #7138, #2642, #21258, #16864 ),
 ( #24996, #24856, #15253, #14861, #23383, #23256, #23128, #5157, #22995, #6608, #13262, #13009, #14993, #21131, #2906, #7386, #15888, #21761, #9393, #23503, #1547, #13636, #9652, #1416, #3535, #3668, #23882, #19632, #23748, #21630 ),
 ( #1165, #9517, #11379, #17623, #3406, #15497, #11635, #23627, #5277, #5406, #19758, #24016, #13507, #17757, #1285, #11507, #5530, #25767, #13902, #25640, #15380, #17887, #9268, #11777, #25898, #1680, #7517, #15625, #7639, #5794 ),
 ( #19895, #15754, #5659, #13382, #11259, #21892, #22035, #13765, #9785, #26036, #19377, #7262, #7773, #17376, #25515, #21509, #19500, #3281, #17499, #12438, #14438, #4080, #2212, #205, #9916, #16166, #22303, #24155, #14170, #12181 ),
 ( #22439, #7912, #20302, #8049, #16030, #76, #8185, #10451, #4216, #20035, #14567, #1813, #12306, #12044, #20164, #2079, #24300, #20566, #24426, #18564, #5932, #343, #26306, #8447, #14305, #1946, #14038, #20433, #6192, #10321 ),
 ( #16302, #22173, #6068, #16566, #3947, #10186, #22567, #18022, #18290, #10053, #18428, #8314, #16437, #24563, #6318, #18160, #4346, #2337, #24696, #6451, #3808, #11913, #26171, #8853, #24969, #25358, #10722, #480, #3004, #20704 ),
 ( #12706, #12849, #16836, #20965, #9109, #17094, #18696, #5005, #10850, #18831, #8585, #22697, #6979, #7113, #8718, #22962, #14967, #4472, #16696, #6716, #11110, #13110, #25226, #4610, #24829, #23102, #21231, #15093, #4742, #21100 ) ),
 .UNSPECIFIED., .T., .F., .T. ) 
 B_SPLINE_SURFACE_WITH_KNOTS ( ( 4, 3, 4 ),
 ( 4, 2, 2, 2, 2, 2, 2, 2, 2, 2, 2, 2, 2, 2, 4 ),
 ( 0.000000000000000000, 0.5000000000000000000, 1.000000000000000000 ),
 ( 0.000000000000000000, 0.1357259735107005372, 0.1651108541090157700, 0.1944957347073310028, 0.3598804999793158710, 0.3867117631979620773, 0.4135430264166082281, 0.5789277916885930964, 0.6062785021374117456, 0.6336292125862302838, 0.8508620842112317728, 0.8814014469398914198, 0.9119408096685510667, 0.9559704048342755334, 1.000000000000000000 ),
 .UNSPECIFIED. ) 
 GEOMETRIC_REPRESENTATION_ITEM ( )  RATIONAL_B_SPLINE_SURFACE ( (
 ( 1.000000000000000000, 1.000000000000000000, 1.000000000000000000, 1.000000000000000000, 1.000000000000000000, 1.000000000000000000, 1.000000000000000000, 1.000000000000000000, 1.000000000000000000, 1.000000000000000000, 1.000000000000000000, 1.000000000000000000, 1.000000000000000000, 1.000000000000000000, 1.000000000000000000, 1.000000000000000000, 1.000000000000000000, 1.000000000000000000, 1.000000000000000000, 1.000000000000000000, 1.000000000000000000, 1.000000000000000000, 1.000000000000000000, 1.000000000000000000, 1.000000000000000000, 1.000000000000000000, 1.000000000000000000, 1.000000000000000000, 1.000000000000000000, 1.000000000000000000),
 ( 0.3333333333333333703, 0.3333333333333333703, 0.3333333333333333703, 0.3333333333333333703, 0.3333333333333333703, 0.3333333333333333703, 0.3333333333333333703, 0.3333333333333333703, 0.3333333333333333703, 0.3333333333333333703, 0.3333333333333333703, 0.3333333333333333703, 0.3333333333333333703, 0.3333333333333333703, 0.3333333333333333703, 0.3333333333333333703, 0.3333333333333333703, 0.3333333333333333703, 0.3333333333333333703, 0.3333333333333333703, 0.3333333333333333703, 0.3333333333333333703, 0.3333333333333333703, 0.3333333333333333703, 0.3333333333333333703, 0.3333333333333333703, 0.3333333333333333703, 0.3333333333333333703, 0.3333333333333333703, 0.3333333333333333703),
 ( 0.3333333333333333703, 0.3333333333333333703, 0.3333333333333333703, 0.3333333333333333703, 0.3333333333333333703, 0.3333333333333333703, 0.3333333333333333703, 0.3333333333333333703, 0.3333333333333333703, 0.3333333333333333703, 0.3333333333333333703, 0.3333333333333333703, 0.3333333333333333703, 0.3333333333333333703, 0.3333333333333333703, 0.3333333333333333703, 0.3333333333333333703, 0.3333333333333333703, 0.3333333333333333703, 0.3333333333333333703, 0.3333333333333333703, 0.3333333333333333703, 0.3333333333333333703, 0.3333333333333333703, 0.3333333333333333703, 0.3333333333333333703, 0.3333333333333333703, 0.3333333333333333703, 0.3333333333333333703, 0.3333333333333333703),
 ( 1.000000000000000000, 1.000000000000000000, 1.000000000000000000, 1.000000000000000000, 1.000000000000000000, 1.000000000000000000, 1.000000000000000000, 1.000000000000000000, 1.000000000000000000, 1.000000000000000000, 1.000000000000000000, 1.000000000000000000, 1.000000000000000000, 1.000000000000000000, 1.000000000000000000, 1.000000000000000000, 1.000000000000000000, 1.000000000000000000, 1.000000000000000000, 1.000000000000000000, 1.000000000000000000, 1.000000000000000000, 1.000000000000000000, 1.000000000000000000, 1.000000000000000000, 1.000000000000000000, 1.000000000000000000, 1.000000000000000000, 1.000000000000000000, 1.000000000000000000),
 ( 0.3333333333333333703, 0.3333333333333333703, 0.3333333333333333703, 0.3333333333333333703, 0.3333333333333333703, 0.3333333333333333703, 0.3333333333333333703, 0.3333333333333333703, 0.3333333333333333703, 0.3333333333333333703, 0.3333333333333333703, 0.3333333333333333703, 0.3333333333333333703, 0.3333333333333333703, 0.3333333333333333703, 0.3333333333333333703, 0.3333333333333333703, 0.3333333333333333703, 0.3333333333333333703, 0.3333333333333333703, 0.3333333333333333703, 0.3333333333333333703, 0.3333333333333333703, 0.3333333333333333703, 0.3333333333333333703, 0.3333333333333333703, 0.3333333333333333703, 0.3333333333333333703, 0.3333333333333333703, 0.3333333333333333703),
 ( 0.3333333333333333703, 0.3333333333333333703, 0.3333333333333333703, 0.3333333333333333703, 0.3333333333333333703, 0.3333333333333333703, 0.3333333333333333703, 0.3333333333333333703, 0.3333333333333333703, 0.3333333333333333703, 0.3333333333333333703, 0.3333333333333333703, 0.3333333333333333703, 0.3333333333333333703, 0.3333333333333333703, 0.3333333333333333703, 0.3333333333333333703, 0.3333333333333333703, 0.3333333333333333703, 0.3333333333333333703, 0.3333333333333333703, 0.3333333333333333703, 0.3333333333333333703, 0.3333333333333333703, 0.3333333333333333703, 0.3333333333333333703, 0.3333333333333333703, 0.3333333333333333703, 0.3333333333333333703, 0.3333333333333333703),
 ( 1.000000000000000000, 1.000000000000000000, 1.000000000000000000, 1.000000000000000000, 1.000000000000000000, 1.000000000000000000, 1.000000000000000000, 1.000000000000000000, 1.000000000000000000, 1.000000000000000000, 1.000000000000000000, 1.000000000000000000, 1.000000000000000000, 1.000000000000000000, 1.000000000000000000, 1.000000000000000000, 1.000000000000000000, 1.000000000000000000, 1.000000000000000000, 1.000000000000000000, 1.000000000000000000, 1.000000000000000000, 1.000000000000000000, 1.000000000000000000, 1.000000000000000000, 1.000000000000000000, 1.000000000000000000, 1.000000000000000000, 1.000000000000000000, 1.000000000000000000) ) ) 
 REPRESENTATION_ITEM ( '' )  SURFACE ( )  );
#18727 = CARTESIAN_POINT ( 'NONE',  ( 0.2972598230769907257, 66.70487387989869887, -10.13633138497392494 ) ) ;
#18726 = CARTESIAN_POINT ( 'NONE',  ( -210.0000000000000284, 75.52305771588336825, -68.47933392563552957 ) ) ;
#18728 = CARTESIAN_POINT ( 'NONE',  ( 57.59792236341147031, -1.722363176415055985, 1.722363176415024677 ) ) ;
#18729 = CARTESIAN_POINT ( 'NONE',  ( -30.26275506840323004, -41.69427246844627888, -40.00000000000002132 ) ) ;
#18730 = CARTESIAN_POINT ( 'NONE',  ( -91.56559293963834989, 17.32597176626808988, 40.00000000000002132 ) ) ;
#18731 = EDGE_CURVE ( 'NONE', #12661, #5675, #20484, .T. ) ;
#18732 = CARTESIAN_POINT ( 'NONE',  ( -198.0356074513804572, -39.99999999999990052, -15.37879056873112482 ) ) ;
#18733 = CARTESIAN_POINT ( 'NONE',  ( 146.6084372240433709, 3.800685668858776900, -52.76785682606518435 ) ) ;
#18734 = CARTESIAN_POINT ( 'NONE',  ( -626.9846540392142060, 75.00000000000000000, 0.000000000000000000 ) ) ;
#18735 = CARTESIAN_POINT ( 'NONE',  ( -135.8532207217289738, 6.472252184284583265, -50.09629031063960980 ) ) ;
#18736 = EDGE_CURVE ( 'NONE', #21682, #5885, #6564, .T. ) ;
#18737 = CARTESIAN_POINT ( 'NONE',  ( -210.0000000000000284, -61.50000000000002132, -66.50000000000005684 ) ) ;
#18738 = ORIENTED_EDGE ( 'NONE', *, *, #6146, .T. ) ;
#18739 = CARTESIAN_POINT ( 'NONE',  ( 184.8905102610680444, 13.49065550809807945, 13.49065550809809544 ) ) ;
#18740 = CIRCLE ( 'NONE', #1321, 74.99999999999995737 ) ;
#18741 = DIRECTION ( 'NONE',  ( 0.000000000000000000, -1.000000000000000000, 0.000000000000000000 ) ) ;
#18742 = CARTESIAN_POINT ( 'NONE',  ( 57.59792236341148453, 1.722363176414758668, 54.84617931850880268 ) ) ;
#18743 = CARTESIAN_POINT ( 'NONE',  ( 8.602182264136155609, -44.88373884392252933, -18.59145335915702901 ) ) ;
#18744 = ORIENTED_EDGE ( 'NONE', *, *, #22984, .F. ) ;
#18745 = CARTESIAN_POINT ( 'NONE',  ( 17.76569288431005234, -48.46476365406682163, -14.04863394049459302 ) ) ;
#18746 = CARTESIAN_POINT ( 'NONE',  ( -102.2610585947573298, -15.74993999358153829, -15.74993999358157204 ) ) ;
#18747 = ORIENTED_EDGE ( 'NONE', *, *, #3782, .F. ) ;
#18748 = CARTESIAN_POINT ( 'NONE',  ( 199.9999999999999147, 19.00141375156598045, 0.3223421948013435179 ) ) ;
#18749 = CARTESIAN_POINT ( 'NONE',  ( -114.6382724355125191, -21.35157561685035787, 5.497872032160216804 ) ) ;
#18750 = CARTESIAN_POINT ( 'NONE',  ( 130.8568914410475088, 5.949712681206712261, 40.00000000000002132 ) ) ;
#18751 = CARTESIAN_POINT ( 'NONE',  ( 91.82158438592158234, -40.45024623143936537, -16.11829626348475131 ) ) ;
#18752 = CARTESIAN_POINT ( 'NONE',  ( 199.0095182511445557, 19.82538855659994681, 2.633105091475395287 ) ) ;
#18753 = AXIS2_PLACEMENT_3D ( 'NONE', #24246, #6019, #2699 ) ;
#18754 = VECTOR ( 'NONE', #16588, 1000.000000000000000 ) ;
#18755 = CARTESIAN_POINT ( 'NONE',  ( -86.96347745069643054, -41.18208027870611687, 15.38646221621750954 ) ) ;
#18756 = CARTESIAN_POINT ( 'NONE',  ( -198.0356074513804572, 39.99999999999979394, 55.37879056874835726 ) ) ;
#18757 = CARTESIAN_POINT ( 'NONE',  ( -100.7734535825088500, 39.99999999999994316, 17.32597176626825686 ) ) ;
#18758 = CARTESIAN_POINT ( 'NONE',  ( -200.0000000000000853, -24.82633483071228753, -44.86878812508721381 ) ) ;
#18759 = CARTESIAN_POINT ( 'NONE',  ( -56.48582580120559271, 9.153146818113576444, -0.000000000000000000 ) ) ;
#18760 = CARTESIAN_POINT ( 'NONE',  ( -597.8386401671281192, 39.36331430824176891, 7.179049609373510776 ) ) ;
#18761 = CARTESIAN_POINT ( 'NONE',  ( -135.8532207217289738, -30.84685318188647685, -2.449293598294708485E-15 ) ) ;
#18762 = CARTESIAN_POINT ( 'NONE',  ( 14.38125909742181996, -10.73282306403606157, 67.30136555895948902 ) ) ;
#18763 = CARTESIAN_POINT ( 'NONE',  ( 147.2817042152898352, -12.35516179550122118, -29.82799917201325002 ) ) ;
#18764 = CARTESIAN_POINT ( 'NONE',  ( -114.5514240058867586, 19.59008466206002197, -9.949107728601523704 ) ) ;
#18765 = CARTESIAN_POINT ( 'NONE',  ( -238.4067589809705794, 3.877349844572403567E-13, -40.96449427998260973 ) ) ;
#18766 = CARTESIAN_POINT ( 'NONE',  ( -100.7734535825088358, -8.145438380286941744E-14, 17.32597176626811120 ) ) ;
#18767 = CARTESIAN_POINT ( 'NONE',  ( 199.0263771353516233, -14.14574067859894413, 14.14574067859863682 ) ) ;
#18768 = CARTESIAN_POINT ( 'NONE',  ( -105.4741150117398263, -19.77569912953930498, 7.943527260776862775 ) ) ;
#18769 = CARTESIAN_POINT ( 'NONE',  ( -114.7252611291636128, -17.87002000140759250, 12.98773421617053714 ) ) ;
#18770 = CARTESIAN_POINT ( 'NONE',  ( -105.3755690713226585, -41.18208027870589660, -15.38646221621809040 ) ) ;
#18771 = ADVANCED_FACE ( 'NONE', ( #21214, #1375 ), #1116, .T. ) ;
#18772 = ORIENTED_EDGE ( 'NONE', *, *, #21363, .T. ) ;
#18773 = CARTESIAN_POINT ( 'NONE',  ( -193.0908841288064650, 24.29092413197486522, -44.14257353178361143 ) ) ;
#18774 = CARTESIAN_POINT ( 'NONE',  ( 210.0000000000000284, 69.29737539576909455, -75.30386416458597409 ) ) ;
#18775 = CARTESIAN_POINT ( 'NONE',  ( 130.8568914410475088, -5.949712681206664300, -40.00000000000002132 ) ) ;
#18776 = CARTESIAN_POINT ( 'NONE',  ( -350.0000000000001137, -4.857225732735059864E-14, 31.79780246617542616 ) ) ;
#18777 = DIRECTION ( 'NONE',  ( -1.000000000000000000, 1.836970198721030181E-16, 0.000000000000000000 ) ) ;
#18778 = ORIENTED_EDGE ( 'NONE', *, *, #11030, .T. ) ;
#18779 = ORIENTED_EDGE ( 'NONE', *, *, #11900, .F. ) ;
#18780 = CIRCLE ( 'NONE', #19597, 5.000000000000004441 ) ;
#18781 = CARTESIAN_POINT ( 'NONE',  ( 199.9999999999999147, 1.227885840012788776, 18.97153672786391709 ) ) ;
#18782 = CARTESIAN_POINT ( 'NONE',  ( 98.29820294267490510, 4.808046699556526995E-12, 20.00000000000513722 ) ) ;
#18783 = CARTESIAN_POINT ( 'NONE',  ( 21.25019396252800519, 18.04326867293863756, 43.56030393974966586 ) ) ;
#18784 = B_SPLINE_CURVE_WITH_KNOTS ( 'NONE', 3,
 ( #23690, #2967, #21697, #3473, #19691, #19192, #1479, #975, #9080, #17186, #15194, #5097, #13202, #21324 ),
 .UNSPECIFIED., .F., .F.,
 ( 4, 2, 2, 2, 2, 2, 4 ),
 ( 8.673617379884035472E-18, 0.002941681445496974190, 0.004412522168245463020, 0.005883362890993952717, 0.008825044336490939917, 0.01029588505923942701, 0.01176672578198791584 ),
 .UNSPECIFIED. ) ;
#18785 = ORIENTED_EDGE ( 'NONE', *, *, #23766, .F. ) ;
#18786 = VERTEX_POINT ( 'NONE', #13096 ) ;
#18787 =( BOUNDED_SURFACE ( )  B_SPLINE_SURFACE ( 3, 3, ( 
 ( #24331, #23783, #6095, #15787, #23914, #5689, #13794, #21929, #4640, #16728, #22863, #24999, #22468, #105, #20862, #12606, #16596, #22600, #2504, #18728, #10482, #10615, #14597, #24592, #14864, #374, #20735, #2370, #6752, #14336 ),
 ( #8212, #4247, #12337, #2777, #16468, #22998, #6485, #20465, #12742, #6613, #8478, #2646, #512, #18864, #6348, #16330, #10753, #14467, #20995, #4376, #12466, #20594, #24729, #2239, #24859, #10347, #4505, #14731, #18596, #22726 ),
 ( #8617, #645, #8751, #16867, #18323, #18457, #4775, #12879, #235, #24459, #8347, #6223, #25389, #1288, #3284, #25643, #5035, #11382, #19503, #7008, #9396, #7265, #11017, #8884, #7141, #1168, #17503, #13510, #17253, #15256 ),
 ( #21134, #23386, #19127, #14996, #909, #19257, #11142, #21633, #3160, #19381, #10889, #19001, #17126, #23630, #7389, #5160, #5280, #23131, #1037, #15384, #15500, #778, #5409, #25518, #16995, #13266, #25130, #21388, #11262, #21512 ),
 ( #6880, #4903, #9137, #2909, #9271, #13013, #23506, #3033, #13385, #17379, #9022, #25257, #15129, #13142, #23259, #21261, #13905, #19898, #11780, #11916, #1551, #24302, #20166, #3538, #18162, #23885, #20038, #17760, #15757, #8051 ),
 ( #24157, #18025, #1683, #5934, #3811, #3949, #9655, #19636, #14040, #25901, #6070, #7642, #5662, #13768, #9788, #25770, #1816, #7520, #15891, #9919, #21895, #3672, #14172, #17890, #7776, #26039, #19761, #22175, #1948, #16168 ),
 ( #13639, #12046, #11638, #10055, #24019, #26308, #3409, #11510, #5798, #1419, #9520, #22039, #17626, #26174, #7914, #15628, #16032, #23751, #5533, #21765, #2339, #10453, #10188, #18698, #14569, #20836, #22699, #14307, #6718, #6584 ) ),
 .UNSPECIFIED., .T., .F., .F. ) 
 B_SPLINE_SURFACE_WITH_KNOTS ( ( 4, 3, 4 ),
 ( 4, 2, 2, 2, 2, 2, 2, 2, 2, 2, 2, 2, 2, 2, 4 ),
 ( 0.000000000000000000, 0.5000000000000000000, 1.000000000000000000 ),
 ( 0.000000000000000000, 0.1357259735107005372, 0.1651108541090157700, 0.1944957347073310028, 0.3598804999793158710, 0.3867117631979620773, 0.4135430264166082281, 0.5789277916885930964, 0.6062785021374117456, 0.6336292125862302838, 0.8508620842112317728, 0.8814014469398914198, 0.9119408096685510667, 0.9559704048342755334, 1.000000000000000000 ),
 .UNSPECIFIED. ) 
 GEOMETRIC_REPRESENTATION_ITEM ( )  RATIONAL_B_SPLINE_SURFACE ( (
 ( 1.000000000000000000, 1.000000000000000000, 1.000000000000000000, 1.000000000000000000, 1.000000000000000000, 1.000000000000000000, 1.000000000000000000, 1.000000000000000000, 1.000000000000000000, 1.000000000000000000, 1.000000000000000000, 1.000000000000000000, 1.000000000000000000, 1.000000000000000000, 1.000000000000000000, 1.000000000000000000, 1.000000000000000000, 1.000000000000000000, 1.000000000000000000, 1.000000000000000000, 1.000000000000000000, 1.000000000000000000, 1.000000000000000000, 1.000000000000000000, 1.000000000000000000, 1.000000000000000000, 1.000000000000000000, 1.000000000000000000, 1.000000000000000000, 1.000000000000000000),
 ( 0.3333333333333333703, 0.3333333333333333703, 0.3333333333333333703, 0.3333333333333333703, 0.3333333333333333703, 0.3333333333333333703, 0.3333333333333333703, 0.3333333333333333703, 0.3333333333333333703, 0.3333333333333333703, 0.3333333333333333703, 0.3333333333333333703, 0.3333333333333333703, 0.3333333333333333703, 0.3333333333333333703, 0.3333333333333333703, 0.3333333333333333703, 0.3333333333333333703, 0.3333333333333333703, 0.3333333333333333703, 0.3333333333333333703, 0.3333333333333333703, 0.3333333333333333703, 0.3333333333333333703, 0.3333333333333333703, 0.3333333333333333703, 0.3333333333333333703, 0.3333333333333333703, 0.3333333333333333703, 0.3333333333333333703),
 ( 0.3333333333333333703, 0.3333333333333333703, 0.3333333333333333703, 0.3333333333333333703, 0.3333333333333333703, 0.3333333333333333703, 0.3333333333333333703, 0.3333333333333333703, 0.3333333333333333703, 0.3333333333333333703, 0.3333333333333333703, 0.3333333333333333703, 0.3333333333333333703, 0.3333333333333333703, 0.3333333333333333703, 0.3333333333333333703, 0.3333333333333333703, 0.3333333333333333703, 0.3333333333333333703, 0.3333333333333333703, 0.3333333333333333703, 0.3333333333333333703, 0.3333333333333333703, 0.3333333333333333703, 0.3333333333333333703, 0.3333333333333333703, 0.3333333333333333703, 0.3333333333333333703, 0.3333333333333333703, 0.3333333333333333703),
 ( 1.000000000000000000, 1.000000000000000000, 1.000000000000000000, 1.000000000000000000, 1.000000000000000000, 1.000000000000000000, 1.000000000000000000, 1.000000000000000000, 1.000000000000000000, 1.000000000000000000, 1.000000000000000000, 1.000000000000000000, 1.000000000000000000, 1.000000000000000000, 1.000000000000000000, 1.000000000000000000, 1.000000000000000000, 1.000000000000000000, 1.000000000000000000, 1.000000000000000000, 1.000000000000000000, 1.000000000000000000, 1.000000000000000000, 1.000000000000000000, 1.000000000000000000, 1.000000000000000000, 1.000000000000000000, 1.000000000000000000, 1.000000000000000000, 1.000000000000000000),
 ( 0.3333333333333333703, 0.3333333333333333703, 0.3333333333333333703, 0.3333333333333333703, 0.3333333333333333703, 0.3333333333333333703, 0.3333333333333333703, 0.3333333333333333703, 0.3333333333333333703, 0.3333333333333333703, 0.3333333333333333703, 0.3333333333333333703, 0.3333333333333333703, 0.3333333333333333703, 0.3333333333333333703, 0.3333333333333333703, 0.3333333333333333703, 0.3333333333333333703, 0.3333333333333333703, 0.3333333333333333703, 0.3333333333333333703, 0.3333333333333333703, 0.3333333333333333703, 0.3333333333333333703, 0.3333333333333333703, 0.3333333333333333703, 0.3333333333333333703, 0.3333333333333333703, 0.3333333333333333703, 0.3333333333333333703),
 ( 0.3333333333333333703, 0.3333333333333333703, 0.3333333333333333703, 0.3333333333333333703, 0.3333333333333333703, 0.3333333333333333703, 0.3333333333333333703, 0.3333333333333333703, 0.3333333333333333703, 0.3333333333333333703, 0.3333333333333333703, 0.3333333333333333703, 0.3333333333333333703, 0.3333333333333333703, 0.3333333333333333703, 0.3333333333333333703, 0.3333333333333333703, 0.3333333333333333703, 0.3333333333333333703, 0.3333333333333333703, 0.3333333333333333703, 0.3333333333333333703, 0.3333333333333333703, 0.3333333333333333703, 0.3333333333333333703, 0.3333333333333333703, 0.3333333333333333703, 0.3333333333333333703, 0.3333333333333333703, 0.3333333333333333703),
 ( 1.000000000000000000, 1.000000000000000000, 1.000000000000000000, 1.000000000000000000, 1.000000000000000000, 1.000000000000000000, 1.000000000000000000, 1.000000000000000000, 1.000000000000000000, 1.000000000000000000, 1.000000000000000000, 1.000000000000000000, 1.000000000000000000, 1.000000000000000000, 1.000000000000000000, 1.000000000000000000, 1.000000000000000000, 1.000000000000000000, 1.000000000000000000, 1.000000000000000000, 1.000000000000000000, 1.000000000000000000, 1.000000000000000000, 1.000000000000000000, 1.000000000000000000, 1.000000000000000000, 1.000000000000000000, 1.000000000000000000, 1.000000000000000000, 1.000000000000000000) ) ) 
 REPRESENTATION_ITEM ( '' )  SURFACE ( )  );
#18788 = CARTESIAN_POINT ( 'NONE',  ( 91.82158438592158234, -40.45024623143958564, 16.11829626348418998 ) ) ;
#18789 = CARTESIAN_POINT ( 'NONE',  ( 199.0143331921596257, -11.79252763263196613, -16.15335214697885391 ) ) ;
#18790 = LINE ( 'NONE', #22657, #15367 ) ;
#18791 = CARTESIAN_POINT ( 'NONE',  ( 4.995406935893297096, 10.78321810387837232, 67.35176059880234334 ) ) ;
#18792 = DIRECTION ( 'NONE',  ( -0.2259624731742164438, 0.000000000000000000, -0.9741360072992845121 ) ) ;
#18793 = CARTESIAN_POINT ( 'NONE',  ( 192.4448373802101173, 40.00000000000012790, -20.00000000003928236 ) ) ;
#18794 = DIRECTION ( 'NONE',  ( 1.303213150798907793E-16, -1.000000000000000000, 2.775557561562890858E-16 ) ) ;
#18795 = CARTESIAN_POINT ( 'NONE',  ( -200.0000000000000000, 82.50000000000008527, -52.49999999999978684 ) ) ;
#18796 = CARTESIAN_POINT ( 'NONE',  ( 163.1118516004056573, 40.00000000000017764, -12.73709011382432976 ) ) ;
#18797 = CARTESIAN_POINT ( 'NONE',  ( -208.1127848780264742, 40.00000000000055422, -55.00245453014380814 ) ) ;
#18798 = CARTESIAN_POINT ( 'NONE',  ( -628.0242092632672666, 26.47293101200708776, 29.98642280378765435 ) ) ;
#18799 = AXIS2_PLACEMENT_3D ( 'NONE', #16441, #22443, #18568 ) ;
#18800 = DIRECTION ( 'NONE',  ( 1.000000000000000000, 1.836970198721030181E-16, -0.000000000000000000 ) ) ;
#18801 = CARTESIAN_POINT ( 'NONE',  ( 199.0069448139248891, 19.47830345430216070, -4.521371627647083891 ) ) ;
#18802 = CARTESIAN_POINT ( 'NONE',  ( -188.6889827002260631, 13.84869468768024703, 47.12918603174951926 ) ) ;
#18803 = CARTESIAN_POINT ( 'NONE',  ( -280.0000000000000000, 14.14213562373078581, 14.14213562373108424 ) ) ;
#18804 = CARTESIAN_POINT ( 'NONE',  ( -192.1166648175283456, -48.16216898722870354, 14.00295691731075109 ) ) ;
#18805 = CARTESIAN_POINT ( 'NONE',  ( -280.0000000000000568, 42.42640687119274645, 14.14213562373118194 ) ) ;
#18806 = CARTESIAN_POINT ( 'NONE',  ( 200.0000000000000000, 71.50000000000009948, 66.50000000000005684 ) ) ;
#18807 = CARTESIAN_POINT ( 'NONE',  ( -135.8532207217289738, -21.81201906317757633, -21.81201906317793515 ) ) ;
#18808 = CARTESIAN_POINT ( 'NONE',  ( -200.0000000000000284, 48.92947633520098805, -14.52307781036565437 ) ) ;
#18809 = CARTESIAN_POINT ( 'NONE',  ( 170.2234770963711128, 24.55285855007190321, 0.000000000000000000 ) ) ;
#18810 = CARTESIAN_POINT ( 'NONE',  ( 192.4448373802100889, -14.14213562375896061, 14.14213562375865330 ) ) ;
#18811 = CARTESIAN_POINT ( 'NONE',  ( -135.8532207217289738, 9.153146818113548022, 40.00000000000002132 ) ) ;
#18812 = CARTESIAN_POINT ( 'NONE',  ( -598.7739420286916356, 39.94555953491243372, 20.74621423265620379 ) ) ;
#18813 = ORIENTED_EDGE ( 'NONE', *, *, #7511, .T. ) ;
#18814 = CARTESIAN_POINT ( 'NONE',  ( -259.2033419157646676, -40.00000000000017053, 9.517827891722212996 ) ) ;
#18815 = CARTESIAN_POINT ( 'NONE',  ( 199.0119081132318115, -7.641483972870305230, -18.48045621412796891 ) ) ;
#18816 = CARTESIAN_POINT ( 'NONE',  ( 147.2817042152898352, -12.35516179550165283, 29.82799917201307238 ) ) ;
#18817 = EDGE_LOOP ( 'NONE', ( #9410, #3720, #5880, #3853 ) ) ;
#18818 = ORIENTED_EDGE ( 'NONE', *, *, #25191, .T. ) ;
#18819 = CARTESIAN_POINT ( 'NONE',  ( -259.2033419157646676, 30.48217210827734647, 2.449293598294708485E-15 ) ) ;
#18820 = CYLINDRICAL_SURFACE ( 'NONE', #7029, 31.79780246617542616 ) ;
#18821 = CARTESIAN_POINT ( 'NONE',  ( -105.3846709045546106, -20.33574920587810908, 6.705972854941914640 ) ) ;
#18822 = EDGE_CURVE ( 'NONE', #6493, #19428, #23868, .T. ) ;
#18823 = LINE ( 'NONE', #20957, #4501 ) ;
#18824 = CARTESIAN_POINT ( 'NONE',  ( -199.9999999999999432, 14.17215463606722636, -49.28189405767596298 ) ) ;
#18825 = CARTESIAN_POINT ( 'NONE',  ( 199.9999999999998010, -4.930716969832944940, -18.35446462305003834 ) ) ;
#18826 = CARTESIAN_POINT ( 'NONE',  ( -105.3174603216990590, 5.405945607584760282, -20.76742684539521022 ) ) ;
#18827 = CARTESIAN_POINT ( 'NONE',  ( -280.0000000000000000, -14.14213562373118549, 14.14213562373078936 ) ) ;
#18828 = CARTESIAN_POINT ( 'NONE',  ( -135.8532207217289738, 6.472252184284096543, 6.472252184284234211 ) ) ;
#18829 = CARTESIAN_POINT ( 'NONE',  ( -94.58238812364415082, 20.73544118676234405, 8.588900961346663365 ) ) ;
#18830 = CARTESIAN_POINT ( 'NONE',  ( 4.995406935893283773, 40.00000000000017764, -15.24977328854790848 ) ) ;
#18831 = CARTESIAN_POINT ( 'NONE',  ( -105.3755690713226727, 15.38646221621771737, 15.38646221621800514 ) ) ;
#18832 = B_SPLINE_CURVE_WITH_KNOTS ( 'NONE', 1,
 ( #25713, #3355 ),
 .UNSPECIFIED., .F., .F.,
 ( 2, 2 ),
 ( 0.000000000000000000, 1.000000000000000000 ),
 .UNSPECIFIED. ) ;
#18833 = CARTESIAN_POINT ( 'NONE',  ( 23.23834162557122696, 13.80856396595914504, 46.85950693575291837 ) ) ;
#18834 = CARTESIAN_POINT ( 'NONE',  ( 91.82158438592158234, -12.16597498397761967, -12.16597498397768007 ) ) ;
#18835 = EDGE_CURVE ( 'NONE', #13885, #9833, #1442, .T. ) ;
#18836 = CARTESIAN_POINT ( 'NONE',  ( -30.26275506840322294, -57.76657404653985139, 1.198031551615709844 ) ) ;
#18837 = CARTESIAN_POINT ( 'NONE',  ( 199.0105800778188723, 19.37561348799876626, 4.995799333890384553 ) ) ;
#18838 = EDGE_CURVE ( 'NONE', #817, #12121, #11774, .T. ) ;
#18840 = CARTESIAN_POINT ( 'NONE',  ( 57.59792236341146321, 40.00000000000004263, -2.435789363418021214 ) ) ;
#18839 = CARTESIAN_POINT ( 'NONE',  ( -56.48582580120559982, -34.75652343174584047, -21.81201906317815187 ) ) ;
#18841 = CARTESIAN_POINT ( 'NONE',  ( 60.14720761588542075, 31.22869220292431081, -15.75494750901078689 ) ) ;
#18842 = CYLINDRICAL_SURFACE ( 'NONE', #24040, 10.00000000000000888 ) ;
#18843 = CARTESIAN_POINT ( 'NONE',  ( 199.9999999999999432, -14.14213562373096345, -14.14213562373104871 ) ) ;
#18844 = CARTESIAN_POINT ( 'NONE',  ( 4.995406935893288214, 15.24977328854832770, 40.00000000000002132 ) ) ;
#18845 = VERTEX_POINT ( 'NONE', #19331 ) ;
#18846 = CARTESIAN_POINT ( 'NONE',  ( 12.96694272564372952, -44.79869582453225263, 24.77464205076265102 ) ) ;
#18847 = CARTESIAN_POINT ( 'NONE',  ( -208.1127848780265026, 55.00245453012668406, 2.449293598294708485E-15 ) ) ;
#18848 = ORIENTED_EDGE ( 'NONE', *, *, #2985, .F. ) ;
#18849 = CARTESIAN_POINT ( 'NONE',  ( -200.0000000000000000, -66.50000000000001421, -66.50000000000005684 ) ) ;
#18850 = CARTESIAN_POINT ( 'NONE',  ( -208.1127848780265026, 10.60833733269537049, 10.60833733269544510 ) ) ;
#18851 = CARTESIAN_POINT ( 'NONE',  ( -8.255580677152480007, -13.52904896325719442, 45.52720393890135853 ) ) ;
#18852 = CARTESIAN_POINT ( 'NONE',  ( 2.332272417553664212, 14.08759251168236126, -48.72342300851929053 ) ) ;
#18853 = CARTESIAN_POINT ( 'NONE',  ( 199.0220583073800640, -19.74674823417053915, -3.257374120286249397 ) ) ;
#18854 = CARTESIAN_POINT ( 'NONE',  ( 199.9999999999999432, -14.14213562373115884, 14.14213562373085153 ) ) ;
#18855 = CARTESIAN_POINT ( 'NONE',  ( -87.08748155317185535, -21.19318107433443643, 3.397954955125616294 ) ) ;
#18856 = CARTESIAN_POINT ( 'NONE',  ( -362.0709805440841365, -10.00000000000009770, 1.224646799147362328E-15 ) ) ;
#18857 = CARTESIAN_POINT ( 'NONE',  ( -189.0115661350366167, -17.94954792649329178, 43.33404204260367720 ) ) ;
#18858 = CARTESIAN_POINT ( 'NONE',  ( 146.6084372240433993, 24.48358557860307272, 24.48358557860347418 ) ) ;
#18859 = CARTESIAN_POINT ( 'NONE',  ( -30.26275506840323359, -1.198031551616339341, 57.76657404653985139 ) ) ;
#18860 = CARTESIAN_POINT ( 'NONE',  ( 0.2972598230770011618, 10.13633138497555919, -66.70487387989845729 ) ) ;
#18861 = CARTESIAN_POINT ( 'NONE',  ( 91.82158438592158234, 12.16597498397756993, 12.16597498397776356 ) ) ;
#18863 = CARTESIAN_POINT ( 'NONE',  ( -162.0762913951020892, 29.48230308784799902, -29.48230308784730980 ) ) ;
#18862 = CARTESIAN_POINT ( 'NONE',  ( -197.4153392275520673, 14.14666332909923874, -49.11379398044257982 ) ) ;
#18864 = CARTESIAN_POINT ( 'NONE',  ( -56.48582580120559982, 21.81201906317729922, 34.75652343174635917 ) ) ;
#18865 = CARTESIAN_POINT ( 'NONE',  ( 130.8568914410475088, -5.949712681206671405, 40.00000000000002132 ) ) ;
#18866 = CARTESIAN_POINT ( 'NONE',  ( 163.1118516004056573, 12.73709011382478806, -40.00000000000002132 ) ) ;
#18867 = CARTESIAN_POINT ( 'NONE',  ( -105.3755690713226585, 12.89780903124410472, -43.67073346367977393 ) ) ;
#18868 = CARTESIAN_POINT ( 'NONE',  ( -103.9663809734196747, 20.15238534367561130, -8.026122150878887140 ) ) ;
#18869 = CARTESIAN_POINT ( 'NONE',  ( -259.2033419157646676, -21.55415060305824326, -21.55415060305857367 ) ) ;
#18870 =( REPRESENTATION_RELATIONSHIP ('NONE','NONE', #23888, #24774 ) REPRESENTATION_RELATIONSHIP_WITH_TRANSFORMATION ( #7686 )SHAPE_REPRESENTATION_RELATIONSHIP( ) );
#18871 = CARTESIAN_POINT ( 'NONE',  ( -188.3065677117184578, 43.00727648871550457, -23.45084385698009655 ) ) ;
#18872 = ORIENTED_EDGE ( 'NONE', *, *, #9553, .F. ) ;
#18873 = CARTESIAN_POINT ( 'NONE',  ( 57.59792236341147031, 26.56190807104684382, 26.56190807104692553 ) ) ;
#18874 = DIRECTION ( 'NONE',  ( 1.000000000000000000, 1.836970198721030181E-16, 0.000000000000000000 ) ) ;
#18875 = CARTESIAN_POINT ( 'NONE',  ( -100.7734535825088358, -12.25131212657493052, 12.25131212657478130 ) ) ;
#18876 = CARTESIAN_POINT ( 'NONE',  ( -4.076660308449255865, -46.97758120990484798, -13.82548859978903266 ) ) ;
#18877 = ORIENTED_EDGE ( 'NONE', *, *, #7793, .F. ) ;
#18878 = CARTESIAN_POINT ( 'NONE',  ( 7.307793755307403494, -49.33439594495633429, -14.18010697691869026 ) ) ;
#18879 = CARTESIAN_POINT ( 'NONE',  ( -200.0000000000000284, -42.45148791631893204, 35.57044988732123159 ) ) ;
#18880 = EDGE_CURVE ( 'NONE', #9962, #21773, #22195, .T. ) ;
#18881 = CARTESIAN_POINT ( 'NONE',  ( 199.9999999999999716, 7.832101404672591194, -17.31171755797958056 ) ) ;
#18882 = CARTESIAN_POINT ( 'NONE',  ( -114.4364955367328491, -20.29001642038857156, 8.064892380842218600 ) ) ;
#18883 = EDGE_CURVE ( 'NONE', #12962, #9216, #14325, .T. ) ;
#18884 = CARTESIAN_POINT ( 'NONE',  ( 57.59792236341147031, 37.56421063658187620, 2.449293598294708485E-15 ) ) ;
#18885 = CARTESIAN_POINT ( 'NONE',  ( 136.1360204305621266, -24.77266263493151044, 24.77266263493093135 ) ) ;
#18886 = CARTESIAN_POINT ( 'NONE',  ( 199.0168302869249999, 12.92424399662411005, 15.26720349029574564 ) ) ;
#18887 = CARTESIAN_POINT ( 'NONE',  ( -213.1075012329537230, -37.98287015391257881, 18.58567234101111509 ) ) ;
#18888 = CARTESIAN_POINT ( 'NONE',  ( -105.3755690713226727, -8.549198663894545631E-14, 18.24025645688352881 ) ) ;
#18889 = CARTESIAN_POINT ( 'NONE',  ( -91.56559293963836410, 39.99999999999994316, 17.32597176626825330 ) ) ;
#18890 = CARTESIAN_POINT ( 'NONE',  ( -3.486753633152357867, 47.18604396268668921, -13.85715877881427538 ) ) ;
#18891 = CARTESIAN_POINT ( 'NONE',  ( 151.7948205124836534, -6.767089262349000656, -40.00000000000002132 ) ) ;
#18893 = CARTESIAN_POINT ( 'NONE',  ( 146.6084372240433993, 24.48358557860341733, -24.48358557860313311 ) ) ;
#18892 = CARTESIAN_POINT ( 'NONE',  ( 23.40652632868016170, -23.33303889678506948, -42.84715492600943776 ) ) ;
#18894 = CARTESIAN_POINT ( 'NONE',  ( 151.7948205124836250, -6.767089262349004208, -2.449293598294708485E-15 ) ) ;
#18895 = CARTESIAN_POINT ( 'NONE',  ( -192.9588430854689705, -38.51493924976963967, 38.51493924976919914 ) ) ;
#18896 = CARTESIAN_POINT ( 'NONE',  ( 154.0339099654740949, -11.67508747798869528, -28.18615453125294223 ) ) ;
#18897 = CARTESIAN_POINT ( 'NONE',  ( 190.0000000000000000, -61.50000000000001421, 66.50000000000005684 ) ) ;
#18898 = CARTESIAN_POINT ( 'NONE',  ( -213.1075012329537230, 40.00000000000055422, -53.71589010953623244 ) ) ;
#18899 = CARTESIAN_POINT ( 'NONE',  ( 0.2972598230769956662, 39.99999999999983658, 54.33493731733950938 ) ) ;
#18900 = DIRECTION ( 'NONE',  ( 0.000000000000000000, 0.000000000000000000, 1.000000000000000000 ) ) ;
#18901 = CARTESIAN_POINT ( 'NONE',  ( -114.4364955367327497, -8.064892380842218600, -20.29001642038850406 ) ) ;
#18902 = CARTESIAN_POINT ( 'NONE',  ( -114.7827960788991248, -16.12461489702645423, 15.17504536827576977 ) ) ;
#18903 = CARTESIAN_POINT ( 'NONE',  ( 57.59792236341147031, -26.56190807104670171, -30.00663442387710234 ) ) ;
#18904 = EDGE_LOOP ( 'NONE', ( #12255, #10529, #24814, #7726 ) ) ;
#18906 = CARTESIAN_POINT ( 'NONE',  ( -24.88648382766318790, 39.69105101984397521, -12.31763033301884391 ) ) ;
#18905 = LINE ( 'NONE', #25296, #22809 ) ;
#18907 = CARTESIAN_POINT ( 'NONE',  ( 155.1206158682453804, 27.79897307351031088, -11.51471166709240634 ) ) ;
#18908 = CARTESIAN_POINT ( 'NONE',  ( 57.59792236341148453, -37.56421063658185489, -40.00000000000002132 ) ) ;
#18909 = CARTESIAN_POINT ( 'NONE',  ( -86.86493150571118349, -7.943527260495776510, -19.77569912839190280 ) ) ;
#18910 = PLANE ( 'NONE',  #692 ) ;
#18911 = ORIENTED_EDGE ( 'NONE', *, *, #24699, .T. ) ;
#18912 = ORIENTED_EDGE ( 'NONE', *, *, #24587, .T. ) ;
#18913 = CARTESIAN_POINT ( 'NONE',  ( 199.9999999999999716, -10.04560847499968368, 16.14005499122785281 ) ) ;
#18914 = FACE_OUTER_BOUND ( 'NONE', #14716, .T. ) ;
#18915 = ORIENTED_EDGE ( 'NONE', *, *, #5749, .T. ) ;
#18916 = ADVANCED_FACE ( 'NONE', ( #21461 ), #9599, .T. ) ;
#18917 = VERTEX_POINT ( 'NONE', #26050 ) ;
#18918 = CARTESIAN_POINT ( 'NONE',  ( 163.1118516004056573, -19.27778845538761132, -19.27778845538770724 ) ) ;
#18919 = CARTESIAN_POINT ( 'NONE',  ( 199.0249934254769926, -19.32713910159323589, 5.171593721336591010 ) ) ;
#18920 = CARTESIAN_POINT ( 'NONE',  ( -114.4364955367334318, -8.064892380823156515, 20.29001642039686004 ) ) ;
#18921 = EDGE_CURVE ( 'NONE', #7623, #7784, #7530, .T. ) ;
#18922 = CARTESIAN_POINT ( 'NONE',  ( -100.7734535825088500, -44.31723036834903695, 12.25131212657476709 ) ) ;
#18923 = CARTESIAN_POINT ( 'NONE',  ( -198.0356074513804572, 10.87444709759714989, 10.87444709759722450 ) ) ;
#18924 = CARTESIAN_POINT ( 'NONE',  ( 14.38125909742180220, 39.99999999999997158, 15.17850393972647716 ) ) ;
#18925 = CARTESIAN_POINT ( 'NONE',  ( -210.0000000000000000, -82.49999999999991473, -52.49999999999977973 ) ) ;
#18926 = EDGE_CURVE ( 'NONE', #14258, #22079, #1799, .T. ) ;
#18927 = EDGE_CURVE ( 'NONE', #12165, #12795, #2896, .T. ) ;
#18928 = CARTESIAN_POINT ( 'NONE',  ( -105.4741150117382062, 7.943527260750565588, -19.77569912955109288 ) ) ;
#18929 = CARTESIAN_POINT ( 'NONE',  ( 4.995406935893298872, 5.820775922023080204E-13, -55.24977328854835434 ) ) ;
#18930 = CARTESIAN_POINT ( 'NONE',  ( -162.0762913951021176, 40.00000000000001421, -1.694272876827905394 ) ) ;
#18931 = CARTESIAN_POINT ( 'NONE',  ( -87.10188448154612217, 17.05386097136903700, 13.04993700312317628 ) ) ;
#18932 = CARTESIAN_POINT ( 'NONE',  ( 190.0000000000000000, -52.49999999999972289, -82.49999999999998579 ) ) ;
#18933 = CARTESIAN_POINT ( 'NONE',  ( 199.0112867096082141, 18.93484222638594616, 6.440921653838688421 ) ) ;
#18934 = CARTESIAN_POINT ( 'NONE',  ( -188.8531444083250790, 17.93248118558191706, 43.29283928523306457 ) ) ;
#18935 = CARTESIAN_POINT ( 'NONE',  ( 130.8568914410475088, -4.207082182990058428, 52.36146031193416661 ) ) ;
#18936 = CARTESIAN_POINT ( 'NONE',  ( -88.39148973765269091, 8.577159256668403842, 19.92926839984458098 ) ) ;
#18937 = CARTESIAN_POINT ( 'NONE',  ( -280.0000000000000568, 14.14213562373067745, 42.42640687119295251 ) ) ;
#18938 = CARTESIAN_POINT ( 'NONE',  ( -77.55632011645045054, -15.16702236933177517, 16.13210123264064322 ) ) ;
#18939 = CIRCLE ( 'NONE', #5742, 14.99999999999999822 ) ;
#18940 = VECTOR ( 'NONE', #18666, 1000.000000000000000 ) ;
#18941 = CARTESIAN_POINT ( 'NONE',  ( 91.82158438592159655, 12.16597498400091304, -44.40256751092321963 ) ) ;
#18942 = CARTESIAN_POINT ( 'NONE',  ( -661.9254414355356175, 44.95389495940958824, -2.363913691310066234 ) ) ;
#18943 = CARTESIAN_POINT ( 'NONE',  ( -238.4067589809705794, -0.9644942799826262680, 0.000000000000000000 ) ) ;
#18944 = CARTESIAN_POINT ( 'NONE',  ( -135.8532207217289738, 21.81201906317729566, 34.75652343174635917 ) ) ;
#18945 = CARTESIAN_POINT ( 'NONE',  ( -259.2033419157646676, 9.517827891722582478, 40.00000000000002132 ) ) ;
#18946 =( BOUNDED_SURFACE ( )  B_SPLINE_SURFACE ( 3, 3, ( 
 ( #19297, #21553, #23797, #19425, #17171, #13307, #25304, #3454, #21426, #1080, #7559, #15671, #17302, #9189, #15178, #23303, #5081, #25561, #25434, #7181, #23426, #3198, #5203, #1211, #23549, #3327, #13808, #15933, #6107, #26221 ),
 ( #5702, #3718, #10229, #5842, #17935, #4128, #24475, #14215, #1860, #18338, #12222, #7689, #22350, #9695, #17802, #4258, #13946, #11820, #21942, #120, #7957, #15802, #20344, #22081, #24066, #26351, #16075, #22215, #18198, #3854 ),
 ( #8225, #2121, #9964, #8092, #24343, #23927, #11957, #19938, #16343, #6237, #24203, #1723, #14351, #26082, #18070, #9831, #22479, #12348, #25948, #7817, #1594, #20082, #20212, #16212, #5976, #14084, #3991, #1990, #12090, #10096 ),
 ( #10763, #8894, #12754, #20607, #14874, #6762, #14479, #24872, #655, #8762, #18875, #2250, #4651, #24606, #23141, #17005, #16480, #20477, #6627, #10631, #6360, #20878, #23014, #2516, #2658, #16877, #25009, #19012, #22738, #790 ),
 ( #4787, #18607, #22612, #12891, #16608, #21005, #2787, #25142, #10900, #6893, #523, #4388, #4521, #15008, #14744, #18469, #4912, #10359, #386, #18742, #250, #8359, #12480, #2382, #8495, #10494, #24741, #6496, #14607, #12619 ),
 ( #20747, #8628, #16739, #22874, #13024, #7018, #21144, #2918, #11026, #17135, #920, #9031, #19136, #25268, #15139, #23269, #15973, #7852, #10490, #18465, #6355, #2377, #26113, #20742, #17966, #3891, #15832, #16735, #22870, #14474 ),
 ( #23962, #8488, #16603, #242, #5737, #2511, #9864, #11991, #25981, #22733, #24867, #9732, #13842, #519, #14739, #4383, #18603, #24099, #5874, #9996, #12475, #21976, #8624, #20602, #382, #13981, #3748, #11854, #22114, #24736 ) ),
 .UNSPECIFIED., .T., .F., .T. ) 
 B_SPLINE_SURFACE_WITH_KNOTS ( ( 4, 3, 4 ),
 ( 4, 2, 2, 2, 2, 2, 2, 2, 2, 2, 2, 2, 2, 2, 4 ),
 ( 0.000000000000000000, 0.5000000000000000000, 1.000000000000000000 ),
 ( 0.000000000000000000, 0.1357259735107005372, 0.1651108541090157700, 0.1944957347073310028, 0.3598804999793158710, 0.3867117631979620773, 0.4135430264166082281, 0.5789277916885930964, 0.6062785021374117456, 0.6336292125862302838, 0.8508620842112317728, 0.8814014469398914198, 0.9119408096685510667, 0.9559704048342755334, 1.000000000000000000 ),
 .UNSPECIFIED. ) 
 GEOMETRIC_REPRESENTATION_ITEM ( )  RATIONAL_B_SPLINE_SURFACE ( (
 ( 1.000000000000000000, 1.000000000000000000, 1.000000000000000000, 1.000000000000000000, 1.000000000000000000, 1.000000000000000000, 1.000000000000000000, 1.000000000000000000, 1.000000000000000000, 1.000000000000000000, 1.000000000000000000, 1.000000000000000000, 1.000000000000000000, 1.000000000000000000, 1.000000000000000000, 1.000000000000000000, 1.000000000000000000, 1.000000000000000000, 1.000000000000000000, 1.000000000000000000, 1.000000000000000000, 1.000000000000000000, 1.000000000000000000, 1.000000000000000000, 1.000000000000000000, 1.000000000000000000, 1.000000000000000000, 1.000000000000000000, 1.000000000000000000, 1.000000000000000000),
 ( 0.3333333333333333703, 0.3333333333333333703, 0.3333333333333333703, 0.3333333333333333703, 0.3333333333333333703, 0.3333333333333333703, 0.3333333333333333703, 0.3333333333333333703, 0.3333333333333333703, 0.3333333333333333703, 0.3333333333333333703, 0.3333333333333333703, 0.3333333333333333703, 0.3333333333333333703, 0.3333333333333333703, 0.3333333333333333703, 0.3333333333333333703, 0.3333333333333333703, 0.3333333333333333703, 0.3333333333333333703, 0.3333333333333333703, 0.3333333333333333703, 0.3333333333333333703, 0.3333333333333333703, 0.3333333333333333703, 0.3333333333333333703, 0.3333333333333333703, 0.3333333333333333703, 0.3333333333333333703, 0.3333333333333333703),
 ( 0.3333333333333333703, 0.3333333333333333703, 0.3333333333333333703, 0.3333333333333333703, 0.3333333333333333703, 0.3333333333333333703, 0.3333333333333333703, 0.3333333333333333703, 0.3333333333333333703, 0.3333333333333333703, 0.3333333333333333703, 0.3333333333333333703, 0.3333333333333333703, 0.3333333333333333703, 0.3333333333333333703, 0.3333333333333333703, 0.3333333333333333703, 0.3333333333333333703, 0.3333333333333333703, 0.3333333333333333703, 0.3333333333333333703, 0.3333333333333333703, 0.3333333333333333703, 0.3333333333333333703, 0.3333333333333333703, 0.3333333333333333703, 0.3333333333333333703, 0.3333333333333333703, 0.3333333333333333703, 0.3333333333333333703),
 ( 1.000000000000000000, 1.000000000000000000, 1.000000000000000000, 1.000000000000000000, 1.000000000000000000, 1.000000000000000000, 1.000000000000000000, 1.000000000000000000, 1.000000000000000000, 1.000000000000000000, 1.000000000000000000, 1.000000000000000000, 1.000000000000000000, 1.000000000000000000, 1.000000000000000000, 1.000000000000000000, 1.000000000000000000, 1.000000000000000000, 1.000000000000000000, 1.000000000000000000, 1.000000000000000000, 1.000000000000000000, 1.000000000000000000, 1.000000000000000000, 1.000000000000000000, 1.000000000000000000, 1.000000000000000000, 1.000000000000000000, 1.000000000000000000, 1.000000000000000000),
 ( 0.3333333333333333703, 0.3333333333333333703, 0.3333333333333333703, 0.3333333333333333703, 0.3333333333333333703, 0.3333333333333333703, 0.3333333333333333703, 0.3333333333333333703, 0.3333333333333333703, 0.3333333333333333703, 0.3333333333333333703, 0.3333333333333333703, 0.3333333333333333703, 0.3333333333333333703, 0.3333333333333333703, 0.3333333333333333703, 0.3333333333333333703, 0.3333333333333333703, 0.3333333333333333703, 0.3333333333333333703, 0.3333333333333333703, 0.3333333333333333703, 0.3333333333333333703, 0.3333333333333333703, 0.3333333333333333703, 0.3333333333333333703, 0.3333333333333333703, 0.3333333333333333703, 0.3333333333333333703, 0.3333333333333333703),
 ( 0.3333333333333333703, 0.3333333333333333703, 0.3333333333333333703, 0.3333333333333333703, 0.3333333333333333703, 0.3333333333333333703, 0.3333333333333333703, 0.3333333333333333703, 0.3333333333333333703, 0.3333333333333333703, 0.3333333333333333703, 0.3333333333333333703, 0.3333333333333333703, 0.3333333333333333703, 0.3333333333333333703, 0.3333333333333333703, 0.3333333333333333703, 0.3333333333333333703, 0.3333333333333333703, 0.3333333333333333703, 0.3333333333333333703, 0.3333333333333333703, 0.3333333333333333703, 0.3333333333333333703, 0.3333333333333333703, 0.3333333333333333703, 0.3333333333333333703, 0.3333333333333333703, 0.3333333333333333703, 0.3333333333333333703),
 ( 1.000000000000000000, 1.000000000000000000, 1.000000000000000000, 1.000000000000000000, 1.000000000000000000, 1.000000000000000000, 1.000000000000000000, 1.000000000000000000, 1.000000000000000000, 1.000000000000000000, 1.000000000000000000, 1.000000000000000000, 1.000000000000000000, 1.000000000000000000, 1.000000000000000000, 1.000000000000000000, 1.000000000000000000, 1.000000000000000000, 1.000000000000000000, 1.000000000000000000, 1.000000000000000000, 1.000000000000000000, 1.000000000000000000, 1.000000000000000000, 1.000000000000000000, 1.000000000000000000, 1.000000000000000000, 1.000000000000000000, 1.000000000000000000, 1.000000000000000000) ) ) 
 REPRESENTATION_ITEM ( '' )  SURFACE ( )  );
#18947 = CARTESIAN_POINT ( 'NONE',  ( -605.6757189317567054, 35.38093617889416720, -27.85243504741141862 ) ) ;
#18948 = EDGE_LOOP ( 'NONE', ( #8673, #19547, #14684, #13544, #13580, #23796 ) ) ;
#18949 = CARTESIAN_POINT ( 'NONE',  ( -105.3755690713226727, 1.741486606973311632E-13, -18.24025645688352881 ) ) ;
#18950 = CARTESIAN_POINT ( 'NONE',  ( 199.0055949646623503, 10.60095110936554974, -16.96607438669680334 ) ) ;
#18951 = CARTESIAN_POINT ( 'NONE',  ( 121.8740240556052612, -11.10671848392298777, 26.81399039734603207 ) ) ;
#18952 = ORIENTED_EDGE ( 'NONE', *, *, #7511, .F. ) ;
#18953 = ORIENTED_EDGE ( 'NONE', *, *, #2842, .T. ) ;
#18954 = ORIENTED_EDGE ( 'NONE', *, *, #4120, .T. ) ;
#18955 = CARTESIAN_POINT ( 'NONE',  ( 14.38125909742180752, 55.17850393974265444, 40.00000000000002132 ) ) ;
#18956 =( GEOMETRIC_REPRESENTATION_CONTEXT ( 3 ) GLOBAL_UNCERTAINTY_ASSIGNED_CONTEXT ( ( #11660 ) ) GLOBAL_UNIT_ASSIGNED_CONTEXT ( ( #15541, #5449, #1459 ) ) REPRESENTATION_CONTEXT ( 'NONE', 'WORKASPACE' ) );
#18957 = CARTESIAN_POINT ( 'NONE',  ( -102.4309680866992238, -20.17061239832209196, -8.733065090195987423 ) ) ;
#18958 = AXIS2_PLACEMENT_3D ( 'NONE', #13347, #1774, #13595 ) ;
#18959 = CARTESIAN_POINT ( 'NONE',  ( -110.0563856373316440, -19.19543633473033850, -6.246938629539779519 ) ) ;
#18960 = DIRECTION ( 'NONE',  ( 0.000000000000000000, 1.000000000000000000, 0.000000000000000000 ) ) ;
#18961 = CARTESIAN_POINT ( 'NONE',  ( -213.1075012329537230, -8.703598725189323045E-14, 13.71589010951911902 ) ) ;
#18962 = CARTESIAN_POINT ( 'NONE',  ( 200.0000000000003126, 15.08009544811998204, -11.56244146370294779 ) ) ;
#18963 = CONICAL_SURFACE ( 'NONE', #1133, 30.00000000000003908, 0.7853981633974531640 ) ;
#18964 = CARTESIAN_POINT ( 'NONE',  ( 170.0000000000000284, -3.062538285713274799, 24.95097643316997704 ) ) ;
#18965 = CARTESIAN_POINT ( 'NONE',  ( -208.1127848780265026, 10.60833733269551615, -10.60833733269529766 ) ) ;
#18966 = DIRECTION ( 'NONE',  ( 0.000000000000000000, 1.000000000000000000, 0.000000000000000000 ) ) ;
#18967 = CARTESIAN_POINT ( 'NONE',  ( 180.0000000000000000, -66.50000000000001421, -66.50000000000005684 ) ) ;
#18968 = CARTESIAN_POINT ( 'NONE',  ( -56.48582580120559982, 40.00000000000034106, -30.84685318188602210 ) ) ;
#18969 = CARTESIAN_POINT ( 'NONE',  ( -103.9474983245001312, -8.027156558344865189, 20.15710290851540520 ) ) ;
#18970 = CARTESIAN_POINT ( 'NONE',  ( -208.1127848780265026, -15.00245453012673202, 0.000000000000000000 ) ) ;
#18971 = CARTESIAN_POINT ( 'NONE',  ( 200.0000000000000000, -42.42640687119269671, -14.14213562373124766 ) ) ;
#18972 = CARTESIAN_POINT ( 'NONE',  ( -162.0762913951020892, -1.694272876828353702, 0.000000000000000000 ) ) ;
#18974 = CARTESIAN_POINT ( 'NONE',  ( -238.4067589809705794, 39.99999999999997158, 0.9644942799827220803 ) ) ;
#18973 = CARTESIAN_POINT ( 'NONE',  ( -86.96347745069644475, -15.38646221621807442, 15.38646221621768184 ) ) ;
#18975 = CLOSED_SHELL ( 'NONE', ( #5819, #4600, #10633, #24792 ) ) ;
#18976 = CARTESIAN_POINT ( 'NONE',  ( -200.0000000000000000, -52.49999999999991473, 82.49999999999998579 ) ) ;
#18977 = CARTESIAN_POINT ( 'NONE',  ( 0.2972598230770011618, 10.13633138497462305, 66.70487387989858519 ) ) ;
#18978 = CARTESIAN_POINT ( 'NONE',  ( 200.0000000000000000, -20.00000000000006750, 40.00000000000002132 ) ) ;
#18979 = ORIENTED_EDGE ( 'NONE', *, *, #11905, .T. ) ;
#18980 = CARTESIAN_POINT ( 'NONE',  ( 9.006212071528537422, -44.90541342374581291, 24.85331907608552271 ) ) ;
#18981 = CARTESIAN_POINT ( 'NONE',  ( 200.0000000000000000, 19.99999999999996447, -40.00000000000002132 ) ) ;
#18982 = CONICAL_SURFACE ( 'NONE', #25777, 30.00000000000003908, 0.7853981633974531640 ) ;
#18983 = VERTEX_POINT ( 'NONE', #21909 ) ;
#18984 = DIRECTION ( 'NONE',  ( 0.000000000000000000, 0.000000000000000000, 1.000000000000000000 ) ) ;
#18985 = CARTESIAN_POINT ( 'NONE',  ( -100.7734535825088500, -44.31723036834903695, 12.25131212657476709 ) ) ;
#18986 = CARTESIAN_POINT ( 'NONE',  ( -70.30307074921901744, -10.20829450076744394, 22.52851052539943666 ) ) ;
#18987 = LINE ( 'NONE', #3271, #21491 ) ;
#18988 = CARTESIAN_POINT ( 'NONE',  ( -47.45115950041520136, 10.57586762663035707, -31.57405104335990487 ) ) ;
#18989 = CARTESIAN_POINT ( 'NONE',  ( 199.0238156666156044, -19.96322609118500324, 1.315852278599464631 ) ) ;
#18990 = EDGE_CURVE ( 'NONE', #18845, #2697, #5202, .T. ) ;
#18991 = CARTESIAN_POINT ( 'NONE',  ( -162.0762913951020892, 1.198031840385732849, -1.198031840385733515 ) ) ;
#18992 = CARTESIAN_POINT ( 'NONE',  ( -87.13361725324693907, -21.49321519332800889, 0.6800178180920880555 ) ) ;
#18993 = CARTESIAN_POINT ( 'NONE',  ( 136.1360204305621266, -35.03383547441293899, 0.000000000000000000 ) ) ;
#18994 = CARTESIAN_POINT ( 'NONE',  ( -195.1685814578020484, -24.52825302093954107, 44.46431112710764211 ) ) ;
#18995 = CARTESIAN_POINT ( 'NONE',  ( -575.0231298121466352, 75.00000000000000000, -30.00000000000202505 ) ) ;
#18996 = CARTESIAN_POINT ( 'NONE',  ( -192.9588430854689989, -10.23066800230756890, 10.23066800230742501 ) ) ;
#18997 = CARTESIAN_POINT ( 'NONE',  ( -198.0356074513804572, 10.87444709759730088, -10.87444709759707173 ) ) ;
#18998 = DIRECTION ( 'NONE',  ( -0.000000000000000000, -1.000000000000000000, -0.000000000000000000 ) ) ;
#19000 = CARTESIAN_POINT ( 'NONE',  ( -91.56559293963834989, 12.25131212657497848, -12.25131212657469426 ) ) ;
#18999 = CARTESIAN_POINT ( 'NONE',  ( -259.2033419157646676, 6.730120644403426944, 6.730120644403592145 ) ) ;
#19001 = CARTESIAN_POINT ( 'NONE',  ( -91.56559293963834989, 12.25131212657497848, -12.25131212657469426 ) ) ;
#19002 = CARTESIAN_POINT ( 'NONE',  ( -100.7734535825088500, 22.67402823373189591, -0.000000000000000000 ) ) ;
#19003 = CARTESIAN_POINT ( 'NONE',  ( 91.82158438592158234, -17.20528682183298486, -40.00000000000002132 ) ) ;
#19004 = CARTESIAN_POINT ( 'NONE',  ( -280.0000000000000568, 14.14213562373097943, -42.42640687119285303 ) ) ;
#19005 = AXIS2_PLACEMENT_3D ( 'NONE', #10791, #8520, #16638 ) ;
#19006 = DIRECTION ( 'NONE',  ( 0.000000000000000000, 0.9767746502210203907, -0.2142691827715860198 ) ) ;
#19007 = CARTESIAN_POINT ( 'NONE',  ( -259.2033419157646676, -21.55415060305872998, 35.01439189186525880 ) ) ;
#19008 = DIRECTION ( 'NONE',  ( 1.000000000000000000, 0.000000000000000000, 0.000000000000000000 ) ) ;
#19009 = ORIENTED_EDGE ( 'NONE', *, *, #3876, .F. ) ;
#19010 = CARTESIAN_POINT ( 'NONE',  ( 91.82158438592158234, -12.16597498400057198, 44.40256751092329779 ) ) ;
#19011 = FACE_OUTER_BOUND ( 'NONE', #12656, .T. ) ;
#19012 = CARTESIAN_POINT ( 'NONE',  ( 184.8905102610680444, -13.49065550809810965, 13.49065550809799596 ) ) ;
#19013 = CARTESIAN_POINT ( 'NONE',  ( 13.28449813601913654, -44.77439867187360534, -24.75673736220152676 ) ) ;
#19014 = VERTEX_POINT ( 'NONE', #11791 ) ;
#19015 = CARTESIAN_POINT ( 'NONE',  ( -184.9729924864174677, -45.83719276899095263, 13.59277144555537298 ) ) ;
#19016 = CARTESIAN_POINT ( 'NONE',  ( -110.1017833366007892, -13.38816311907946144, -15.17212531755836125 ) ) ;
#19017 = CARTESIAN_POINT ( 'NONE',  ( 200.0000000000001421, 16.62132632430557777, -9.210632111445709924 ) ) ;
#19018 = CARTESIAN_POINT ( 'NONE',  ( -200.0000000000000000, 60.00000000000011369, 0.000000000000000000 ) ) ;
#19019 = CARTESIAN_POINT ( 'NONE',  ( -91.56559293963834989, 17.32597176626809699, -40.00000000000002132 ) ) ;
#19020 = CARTESIAN_POINT ( 'NONE',  ( -86.96347745069644475, -43.67073346367964604, -12.89780903124457545 ) ) ;
#19021 = CARTESIAN_POINT ( 'NONE',  ( 199.0158819412750688, 14.24569456864689343, 14.03872682698725249 ) ) ;
#19022 = CARTESIAN_POINT ( 'NONE',  ( 163.1118516004056573, -9.006482792074626431, 47.56205970284951690 ) ) ;
#19023 = CARTESIAN_POINT ( 'NONE',  ( -91.56559293963834989, -40.00000000000009948, 17.32597176626796553 ) ) ;
#19024 = CARTESIAN_POINT ( 'NONE',  ( -208.1127848780264742, 39.99999999999992895, 15.00245453012683683 ) ) ;
#19025 = DIRECTION ( 'NONE',  ( 1.000000000000000000, 1.836970198721030181E-16, 0.000000000000000000 ) ) ;
#19026 = CARTESIAN_POINT ( 'NONE',  ( 57.59792236341148453, -37.56421063658185489, -2.449293598294708485E-15 ) ) ;
#19028 = CARTESIAN_POINT ( 'NONE',  ( -611.8588848697457934, 30.46712910405810959, 25.92524149612432893 ) ) ;
#19027 = CARTESIAN_POINT ( 'NONE',  ( 22.89778847645061788, -17.86913359794365874, -43.13990468001261291 ) ) ;
#19029 = CARTESIAN_POINT ( 'NONE',  ( -162.0762913951020892, -41.69427287672991866, -40.00000000000002132 ) ) ;
#19030 = CARTESIAN_POINT ( 'NONE',  ( -86.96347745069645896, 43.67073346367970288, 12.89780903124427702 ) ) ;
#19031 = CARTESIAN_POINT ( 'NONE',  ( 153.3020327024398455, -11.77299484472929159, -28.42252382389425946 ) ) ;
#19032 = CARTESIAN_POINT ( 'NONE',  ( -114.7755410848721880, 16.60116338994188467, -14.64251757340711357 ) ) ;
#19033 = CARTESIAN_POINT ( 'NONE',  ( -208.1127848780264742, -39.99999999999948841, -55.00245453010965235 ) ) ;
#19034 = CARTESIAN_POINT ( 'NONE',  ( 192.4448373802101173, 14.14213562370320076, -42.42640687122072762 ) ) ;
#19035 = CARTESIAN_POINT ( 'NONE',  ( -726.9846540392142060, 39.99999999999991473, 0.000000000000000000 ) ) ;
#19036 = CARTESIAN_POINT ( 'NONE',  ( -103.9474983244996196, -8.577167319634884990, -19.92928099173804668 ) ) ;
#19037 = CARTESIAN_POINT ( 'NONE',  ( -259.2033419157646676, 35.01439189186528722, 21.55415060305857011 ) ) ;
#19038 = EDGE_LOOP ( 'NONE', ( #26220, #12191, #17002, #9350, #13918, #4126, #12928 ) ) ;
#19040 = CARTESIAN_POINT ( 'NONE',  ( -77.90255099906771363, 20.04994828523961203, -8.644468104261394004 ) ) ;
#19039 = CARTESIAN_POINT ( 'NONE',  ( -77.72892396114323788, -5.803299710953224277, -21.20265378149535351 ) ) ;
#19041 = CARTESIAN_POINT ( 'NONE',  ( 118.9130007099546305, 25.80693111732296074, -10.68958087202326723 ) ) ;
#19042 = CARTESIAN_POINT ( 'NONE',  ( 200.0000000000000000, 20.00000000000013856, -40.00000000000002132 ) ) ;
#19043 = DIRECTION ( 'NONE',  ( 1.750717563385750846E-16, -0.9530462522498561739, -0.3028247695821854046 ) ) ;
#19044 = CARTESIAN_POINT ( 'NONE',  ( -194.4222775681010376, 48.65439176090173135, -14.07715774766184502 ) ) ;
#19045 = ORIENTED_EDGE ( 'NONE', *, *, #18653, .F. ) ;
#19046 = ORIENTED_EDGE ( 'NONE', *, *, #21498, .F. ) ;
#19047 = CARTESIAN_POINT ( 'NONE',  ( -210.0000000000000284, -52.49999999999991473, 82.49999999999998579 ) ) ;
#19048 = ORIENTED_EDGE ( 'NONE', *, *, #8097, .F. ) ;
#19049 = ORIENTED_EDGE ( 'NONE', *, *, #14014, .F. ) ;
#19050 = CARTESIAN_POINT ( 'NONE',  ( 184.8905102610680444, -43.07788698682576722, 13.49065550809799063 ) ) ;
#19051 = CARTESIAN_POINT ( 'NONE',  ( 199.0152737994447136, -13.19951906643276374, -15.03942049639883294 ) ) ;
#19052 = CARTESIAN_POINT ( 'NONE',  ( 180.0000000000000000, -35.78896085774750446, 65.91016826501511616 ) ) ;
#19053 = CARTESIAN_POINT ( 'NONE',  ( -105.3755690713226585, -43.67073346367983788, 12.89780903124397149 ) ) ;
#19054 = LINE ( 'NONE', #14921, #10654 ) ;
#19055 = CARTESIAN_POINT ( 'NONE',  ( 19.06497207195980792, 39.99999999999983658, 54.19242893257857929 ) ) ;
#19056 = LINE ( 'NONE', #4571, #20228 ) ;
#19057 = CARTESIAN_POINT ( 'NONE',  ( -199.9999999999999147, -14.17215463606694925, 49.28189405767609088 ) ) ;
#19058 = CARTESIAN_POINT ( 'NONE',  ( 91.82158438592159655, -39.99999999999976552, -22.79471317813512599 ) ) ;
#19059 = CARTESIAN_POINT ( 'NONE',  ( 184.8905102610680444, 39.99999999999983658, 20.92133201514485563 ) ) ;
#19060 = CARTESIAN_POINT ( 'NONE',  ( 190.0000000000000000, 61.50000000000009948, -66.50000000000005684 ) ) ;
#19061 = CARTESIAN_POINT ( 'NONE',  ( -86.95492405012092263, 9.645501174397823618, 19.11844758104726694 ) ) ;
#19062 = CARTESIAN_POINT ( 'NONE',  ( 199.0054122081438948, 15.86953797770180508, -12.16778084942700211 ) ) ;
#19063 = CARTESIAN_POINT ( 'NONE',  ( -91.56559293963836410, 16.03295912088714203, -16.03295912088699282 ) ) ;
#19064 = CARTESIAN_POINT ( 'NONE',  ( 192.4448373802101173, -42.42640687116510634, 14.14213562375845257 ) ) ;
#19065 = EDGE_CURVE ( 'NONE', #24474, #12861, #11984, .T. ) ;
#19066 = CARTESIAN_POINT ( 'NONE',  ( -189.2428547182112197, -47.31876910929170776, 13.87687415872445662 ) ) ;
#19067 = CARTESIAN_POINT ( 'NONE',  ( 151.7948205124836534, 23.49921654116009506, 33.06932595376371609 ) ) ;
#19068 = FACE_OUTER_BOUND ( 'NONE', #8630, .T. ) ;
#19069 = CARTESIAN_POINT ( 'NONE',  ( 91.82158438592156813, 40.45024623143973486, -16.11829626348390931 ) ) ;
#19070 = LINE ( 'NONE', #25072, #22747 ) ;
#19071 = CARTESIAN_POINT ( 'NONE',  ( 192.4448373802100889, 20.00000000003945644, 0.000000000000000000 ) ) ;
#19072 = VERTEX_POINT ( 'NONE', #24032 ) ;
#19073 = CARTESIAN_POINT ( 'NONE',  ( -86.96347745069644475, 41.18208027870576871, 15.38646221621837107 ) ) ;
#19074 = EDGE_CURVE ( 'NONE', #21974, #12692, #25652, .T. ) ;
#19075 = CARTESIAN_POINT ( 'NONE',  ( 130.8568914410475088, 34.05028731879790627, 40.00000000000002132 ) ) ;
#19076 = CARTESIAN_POINT ( 'NONE',  ( -594.4172314860030610, 43.13402369259207347, -12.87267148120193383 ) ) ;
#19077 = VERTEX_POINT ( 'NONE', #24170 ) ;
#19078 = CARTESIAN_POINT ( 'NONE',  ( -213.1075012329537230, -39.99999999999948841, -53.71589010950208376 ) ) ;
#19079 = EDGE_CURVE ( 'NONE', #1336, #15830, #20178, .T. ) ;
#19080 = CARTESIAN_POINT ( 'NONE',  ( 199.0084611626479045, -0.003522264206503993803, -19.99626311085798136 ) ) ;
#19081 = EDGE_CURVE ( 'NONE', #24779, #14740, #3961, .T. ) ;
#19082 = CARTESIAN_POINT ( 'NONE',  ( 144.1620285550791039, -12.51613133675892975, 30.21661402164544441 ) ) ;
#19083 = ORIENTED_EDGE ( 'NONE', *, *, #1189, .T. ) ;
#19084 = ORIENTED_EDGE ( 'NONE', *, *, #17606, .T. ) ;
#19085 = ORIENTED_EDGE ( 'NONE', *, *, #965, .F. ) ;
#19086 = CARTESIAN_POINT ( 'NONE',  ( -86.96347745069644475, 18.24025645688351105, 2.449293598294708485E-15 ) ) ;
#19087 = SURFACE_SIDE_STYLE ('',( #6836 ) ) ;
#19088 = AXIS2_PLACEMENT_3D ( 'NONE', #9361, #1518, #1648 ) ;
#19089 = DIRECTION ( 'NONE',  ( -1.937599346585394162E-16, -1.000000000000000000, 0.000000000000000000 ) ) ;
#19090 = CARTESIAN_POINT ( 'NONE',  ( 169.9999999999674571, -17.64300463372919836, -17.64300463252165585 ) ) ;
#19091 = CARTESIAN_POINT ( 'NONE',  ( -91.56559293963834989, 6.234561990864368500E-14, -22.67402823373191723 ) ) ;
#19092 = CARTESIAN_POINT ( 'NONE',  ( 199.9999999999999432, 15.63063699308155030, -10.80328371702407786 ) ) ;
#19093 = CARTESIAN_POINT ( 'NONE',  ( 199.9999999999999432, -0.3235039025349020214, -19.00140615985569070 ) ) ;
#19094 = CARTESIAN_POINT ( 'NONE',  ( -86.96347745069644475, -43.67073346367964604, -12.89780903124457545 ) ) ;
#19095 = CARTESIAN_POINT ( 'NONE',  ( 14.38125909742181285, -10.73282306404712472, -10.73282306404731301 ) ) ;
#19096 = CARTESIAN_POINT ( 'NONE',  ( -91.56559293963834989, 1.671088883502053755E-13, -17.32597176626811120 ) ) ;
#19097 = DIRECTION ( 'NONE',  ( 0.000000000000000000, 1.000000000000000000, 0.000000000000000000 ) ) ;
#19098 = DIRECTION ( 'NONE',  ( 0.000000000000000000, -0.3995982397413241904, 0.9166903767334068087 ) ) ;
#19099 = CARTESIAN_POINT ( 'NONE',  ( -105.3755690713226585, 15.38646221621762678, 41.18208027870604582 ) ) ;
#19100 = CARTESIAN_POINT ( 'NONE',  ( -238.4067589809705794, -0.9644942799826262680, 0.000000000000000000 ) ) ;
#19102 = CARTESIAN_POINT ( 'NONE',  ( 19.06497207195979726, 39.99999999999997158, 14.19242893257854554 ) ) ;
#19101 = CARTESIAN_POINT ( 'NONE',  ( 200.0000000000000000, -42.42640687119272513, -14.14213562373140753 ) ) ;
#19103 = CARTESIAN_POINT ( 'NONE',  ( -200.0000000000000000, -52.49999999999991473, 52.49999999999999289 ) ) ;
#19104 = CARTESIAN_POINT ( 'NONE',  ( -213.1075012329537230, -18.58567234101155208, 37.98287015391234434 ) ) ;
#19105 = CARTESIAN_POINT ( 'NONE',  ( 170.2234770963711128, -24.55285855007183926, 0.000000000000000000 ) ) ;
#19106 = VERTEX_POINT ( 'NONE', #18037 ) ;
#19107 = CARTESIAN_POINT ( 'NONE',  ( 17.65190073994094533, -44.23515346912825663, 24.35922420890246087 ) ) ;
#19108 = CARTESIAN_POINT ( 'NONE',  ( -86.96347745069644475, 18.24025645688350750, -40.00000000000002132 ) ) ;
#19109 = CARTESIAN_POINT ( 'NONE',  ( 200.0000000000000000, 57.47694228411675255, -64.52066607436459833 ) ) ;
#19111 = CARTESIAN_POINT ( 'NONE',  ( 163.1118516004056573, -47.56205970284957374, 9.006482792074162802 ) ) ;
#19110 = APPLICATION_CONTEXT ( 'automotive_design' ) ;
#19112 = CARTESIAN_POINT ( 'NONE',  ( -91.56559293963834989, -39.99999999999995737, -22.67402823373205933 ) ) ;
#19113 = CARTESIAN_POINT ( 'NONE',  ( -82.29166192294638904, 18.99061817120102802, -6.834568285704429869 ) ) ;
#19114 = CARTESIAN_POINT ( 'NONE',  ( -24.53392603775095537, 19.42583462371737113, -36.88304647106937750 ) ) ;
#19115 = CARTESIAN_POINT ( 'NONE',  ( 200.0000000000003695, -13.00390091431020956, 13.88089034683036616 ) ) ;
#19116 = CARTESIAN_POINT ( 'NONE',  ( -91.56559293963834989, 12.25131212657428748, 44.31723036834913643 ) ) ;
#19117 = CARTESIAN_POINT ( 'NONE',  ( -82.23726319238257076, -20.19517362728035437, 0.6309363043619388156 ) ) ;
#19118 = CARTESIAN_POINT ( 'NONE',  ( -77.90255099906863734, -20.04994828524331396, -8.644468104250957907 ) ) ;
#19119 = CARTESIAN_POINT ( 'NONE',  ( -200.5022929845067381, -18.58571294254484840, 44.86988025226722243 ) ) ;
#19120 = CARTESIAN_POINT ( 'NONE',  ( 91.82158438592158234, 12.16597498397756993, 12.16597498397776356 ) ) ;
#19121 = AXIS2_PLACEMENT_3D ( 'NONE', #20639, #17036, #12922 ) ;
#19122 = CARTESIAN_POINT ( 'NONE',  ( -259.2033419157646676, 6.730120644403521979, -6.730120644403498886 ) ) ;
#19123 = DIRECTION ( 'NONE',  ( 0.000000000000000000, -0.9307566067079452443, 0.3656393565653338062 ) ) ;
#19124 = LINE ( 'NONE', #3030, #9204 ) ;
#19126 = CARTESIAN_POINT ( 'NONE',  ( -238.4067589809705794, 57.25054294065799354, -0.6820004457334954973 ) ) ;
#19125 = CARTESIAN_POINT ( 'NONE',  ( -135.8532207217289738, 34.75652343174625258, -21.81201906317744132 ) ) ;
#19127 = CARTESIAN_POINT ( 'NONE',  ( -238.4067589809705794, 28.96627169325354956, -28.96627169325289231 ) ) ;
#19128 = CARTESIAN_POINT ( 'NONE',  ( -91.56559293963834989, 17.32597176626809699, -40.00000000000002132 ) ) ;
#19129 = CARTESIAN_POINT ( 'NONE',  ( 192.4448373802101173, 42.42640687116508502, -14.14213562375874567 ) ) ;
#19130 = CARTESIAN_POINT ( 'NONE',  ( -200.0000000000000000, 52.50000000000007816, -52.49999999999999289 ) ) ;
#19131 = CARTESIAN_POINT ( 'NONE',  ( 14.38125909742183062, -67.30136555895943218, -10.73282306403629605 ) ) ;
#19132 = CARTESIAN_POINT ( 'NONE',  ( -188.3120147333544310, 43.00887716025408025, -23.45203116714288427 ) ) ;
#19133 = ORIENTED_EDGE ( 'NONE', *, *, #25271, .F. ) ;
#19134 = CARTESIAN_POINT ( 'NONE',  ( -198.0356074513804572, 10.87444709758468875, 67.44298959250869530 ) ) ;
#19135 = CARTESIAN_POINT ( 'NONE',  ( 160.9163046357249129, -205.7889608577475542, 55.61140153332249980 ) ) ;
#19136 = CARTESIAN_POINT ( 'NONE',  ( -86.96347745069645896, 43.67073346367970288, 12.89780903124427702 ) ) ;
#19137 = CARTESIAN_POINT ( 'NONE',  ( 98.29820294267362613, -18.95183585406276094, -6.423630604794682064 ) ) ;
#19138 = ORIENTED_EDGE ( 'NONE', *, *, #13283, .F. ) ;
#19139 = CARTESIAN_POINT ( 'NONE',  ( -188.2870673237729306, -43.00153493964099738, 23.44688076656430198 ) ) ;
#19140 = AXIS2_PLACEMENT_3D ( 'NONE', #7094, #21457, #23335 ) ;
#19141 = CARTESIAN_POINT ( 'NONE',  ( 200.0000000000001137, 2.164978928433492822, -18.87806096587463855 ) ) ;
#19142 = CARTESIAN_POINT ( 'NONE',  ( 45.01779936581511521, -18.90344565813661859, 36.09695843556287542 ) ) ;
#19143 = CARTESIAN_POINT ( 'NONE',  ( -56.48582580120559982, -9.153146818113595984, -40.00000000000002132 ) ) ;
#19144 = CARTESIAN_POINT ( 'NONE',  ( 67.78092418456155599, 12.11998378897419570, -29.26022923856843860 ) ) ;
#19145 = CARTESIAN_POINT ( 'NONE',  ( 199.0106735244355320, 19.32142130491951804, 5.196343561012195522 ) ) ;
#19146 = CARTESIAN_POINT ( 'NONE',  ( 130.8568914410475088, -32.49135343045495006, 24.07718906446878648 ) ) ;
#19147 = CARTESIAN_POINT ( 'NONE',  ( 14.38125909742181818, -1.924622159709266762E-13, 55.17850393972636880 ) ) ;
#19148 = CARTESIAN_POINT ( 'NONE',  ( 14.38125909742181108, -5.035366881890652543E-14, 15.17850393972633682 ) ) ;
#19149 = CARTESIAN_POINT ( 'NONE',  ( 192.4448373802100889, 1.051811698935164031E-13, -20.00000000003942091 ) ) ;
#19150 = CARTESIAN_POINT ( 'NONE',  ( 151.7948205124835681, 33.23291073765556547, -40.00000000000002132 ) ) ;
#19152 = CARTESIAN_POINT ( 'NONE',  ( -614.3942928892040527, 29.28923948339344108, 27.24720710369317089 ) ) ;
#19151 = CARTESIAN_POINT ( 'NONE',  ( 23.49666234703796519, -13.79192166426271626, -46.76389514419435756 ) ) ;
#19153 = CARTESIAN_POINT ( 'NONE',  ( -105.3755690713226869, 21.75974354311648540, -0.000000000000000000 ) ) ;
#19154 = EDGE_CURVE ( 'NONE', #19072, #862, #7929, .T. ) ;
#19155 = CARTESIAN_POINT ( 'NONE',  ( -91.56559293963836410, 44.31723036834890905, 12.25131212657507795 ) ) ;
#19156 = CARTESIAN_POINT ( 'NONE',  ( 0.2972598230769883387, 40.00000000000017053, -14.33493731733891607 ) ) ;
#19157 = LINE ( 'NONE', #17026, #24691 ) ;
#19158 = CARTESIAN_POINT ( 'NONE',  ( 0.2972598230770030492, -39.99999999999987210, -14.33493731733975451 ) ) ;
#19159 = CARTESIAN_POINT ( 'NONE',  ( 199.0253172846266523, -6.444568167316012008, 18.94088585829734228 ) ) ;
#19160 = CARTESIAN_POINT ( 'NONE',  ( 147.2811880046590147, -29.82808195031421405, -12.35519608339632214 ) ) ;
#19161 = CARTESIAN_POINT ( 'NONE',  ( 19.06497207195979726, 38.31983398719604139, 18.24870850772803976 ) ) ;
#19162 = CARTESIAN_POINT ( 'NONE',  ( 19.06497207195980792, 18.24870850772737185, 38.31983398719634692 ) ) ;
#19163 = EDGE_CURVE ( 'NONE', #2989, #11173, #15381, .T. ) ;
#19164 = ORIENTED_EDGE ( 'NONE', *, *, #15559, .F. ) ;
#19166 = CARTESIAN_POINT ( 'NONE',  ( -198.0012279374158481, 24.77357825033897498, -44.79720170867052786 ) ) ;
#19165 = CARTESIAN_POINT ( 'NONE',  ( -77.90255099906767100, 8.064892378658102601, -20.29001641120677846 ) ) ;
#19167 = PLANE ( 'NONE',  #19520 ) ;
#19168 = CARTESIAN_POINT ( 'NONE',  ( -105.3755690713226585, 21.75974354311648185, 40.00000000000002132 ) ) ;
#19169 = EDGE_CURVE ( 'NONE', #14253, #11184, #17085, .T. ) ;
#19170 =( LENGTH_UNIT ( ) NAMED_UNIT ( * ) SI_UNIT ( .MILLI., .METRE. ) );
#19171 = CARTESIAN_POINT ( 'NONE',  ( -192.1963514251034724, 48.17613439255902108, -14.00508311691898733 ) ) ;
#19172 = DIRECTION ( 'NONE',  ( 0.000000000000000000, 0.000000000000000000, -1.000000000000000000 ) ) ;
#19173 = ORIENTED_EDGE ( 'NONE', *, *, #26237, .T. ) ;
#19174 = ORIENTED_EDGE ( 'NONE', *, *, #3298, .F. ) ;
#19175 = CARTESIAN_POINT ( 'NONE',  ( 73.43468551893278118, -9.843145830824733267, 28.18272074650135295 ) ) ;
#19176 = CARTESIAN_POINT ( 'NONE',  ( -200.0000000000000000, 1.308061781956697717E-29, 0.000000000000000000 ) ) ;
#19177 = CARTESIAN_POINT ( 'NONE',  ( 98.29820294267527458, 2.689882573189819553E-13, -20.00000000000500222 ) ) ;
#19178 = ORIENTED_EDGE ( 'NONE', *, *, #12164, .F. ) ;
#19179 = CARTESIAN_POINT ( 'NONE',  ( 199.0253131443098766, -18.94683372192476156, 6.427280041807147626 ) ) ;
#19180 = AXIS2_PLACEMENT_3D ( 'NONE', #13850, #18241, #18381 ) ;
#19181 = CARTESIAN_POINT ( 'NONE',  ( -114.6821015619662489, -4.467609313239589319, 21.58745106896960664 ) ) ;
#19182 = CARTESIAN_POINT ( 'NONE',  ( 151.7948205124836250, -23.49921654116339553, -23.49921654116350211 ) ) ;
#19183 = AXIS2_PLACEMENT_3D ( 'NONE', #9, #6003, #22105 ) ;
#19184 = CARTESIAN_POINT ( 'NONE',  ( -200.0000000000000000, -69.99999999999998579, 0.000000000000000000 ) ) ;
#19185 = CARTESIAN_POINT ( 'NONE',  ( 130.8568914410475088, 40.00000000000002842, 5.949712681206834830 ) ) ;
#19186 = CARTESIAN_POINT ( 'NONE',  ( -210.0000000000000284, 61.50000000000009948, 66.50000000000005684 ) ) ;
#19187 = DIRECTION ( 'NONE',  ( 1.000000000000000000, 1.836970198721030181E-16, 0.000000000000000000 ) ) ;
#19188 = CARTESIAN_POINT ( 'NONE',  ( 151.7948205124836534, -39.99999999999992184, -6.767089262349454515 ) ) ;
#19189 = CARTESIAN_POINT ( 'NONE',  ( -100.7734535825088358, 1.654174317907124744E-13, -17.32597176626811120 ) ) ;
#19190 = CARTESIAN_POINT ( 'NONE',  ( -77.62095083827057351, 17.94746523758837142, 12.85593168005540043 ) ) ;
#19191 = CARTESIAN_POINT ( 'NONE',  ( -362.0709805440841365, -4.857225732735059864E-14, 0.000000000000000000 ) ) ;
#19192 = CARTESIAN_POINT ( 'NONE',  ( -200.0000000000000000, 18.14835560308000950, -46.41341197396098295 ) ) ;
#19193 = CARTESIAN_POINT ( 'NONE',  ( 184.8905102610680444, 14.79361573936396113, -14.79361573936377461 ) ) ;
#19194 = CARTESIAN_POINT ( 'NONE',  ( -86.86493150571115507, 7.943527260496353826, 19.77569912839162569 ) ) ;
#19195 = LINE ( 'NONE', #23325, #18308 ) ;
#19196 = FACE_OUTER_BOUND ( 'NONE', #14553, .T. ) ;
#19197 = CARTESIAN_POINT ( 'NONE',  ( -77.78761611096672368, -9.949180589415803411, 19.59005896970126770 ) ) ;
#19198 = CIRCLE ( 'NONE', #930, 4.999999999999997335 ) ;
#19199 = CARTESIAN_POINT ( 'NONE',  ( 14.38125909742183062, -67.30136555895943218, -10.73282306403629605 ) ) ;
#19200 = CARTESIAN_POINT ( 'NONE',  ( -653.0828039730662340, 38.48173582175917318, -23.34791170400915306 ) ) ;
#19201 = CARTESIAN_POINT ( 'NONE',  ( 180.0000000000000000, -71.50000000000002842, 66.50000000000005684 ) ) ;
#19202 = ORIENTED_EDGE ( 'NONE', *, *, #9711, .F. ) ;
#19203 = CARTESIAN_POINT ( 'NONE',  ( 130.8568914410475372, -24.07718906447255947, 24.07718906447199458 ) ) ;
#19204 = DIRECTION ( 'NONE',  ( -1.000000000000000000, 0.000000000000000000, 0.000000000000000000 ) ) ;
#19205 = CARTESIAN_POINT ( 'NONE',  ( -595.2966944841457462, 42.47393186636156059, 14.90703951832045959 ) ) ;
#19206 = ORIENTED_EDGE ( 'NONE', *, *, #10297, .F. ) ;
#19207 = CARTESIAN_POINT ( 'NONE',  ( -100.7734535825088500, -40.00000000000027711, 22.67402823373149801 ) ) ;
#19208 = CARTESIAN_POINT ( 'NONE',  ( 199.0082391558451320, 0.5918947795737343753, -19.98868739452279897 ) ) ;
#19209 = VERTEX_POINT ( 'NONE', #8053 ) ;
#19210 = EDGE_LOOP ( 'NONE', ( #12224, #25216, #20508, #26020 ) ) ;
#19211 = ORIENTED_EDGE ( 'NONE', *, *, #5900, .T. ) ;
#19212 = CARTESIAN_POINT ( 'NONE',  ( -259.2033419157646676, 30.48217210827735713, -40.00000000000002132 ) ) ;
#19213 = UNCERTAINTY_MEASURE_WITH_UNIT (LENGTH_MEASURE( 1.000000000000000082E-05 ), #10268, 'distance_accuracy_value', 'NONE');
#19214 =( NAMED_UNIT ( * ) SI_UNIT ( $, .STERADIAN. ) SOLID_ANGLE_UNIT ( ) );
#19215 = EDGE_CURVE ( 'NONE', #13305, #15869, #18425, .T. ) ;
#19216 = VECTOR ( 'NONE', #14053, 1000.000000000000000 ) ;
#19217 = CARTESIAN_POINT ( 'NONE',  ( 136.1360204305621266, -24.77266263493116583, -24.77266263493127951 ) ) ;
#19218 = CARTESIAN_POINT ( 'NONE',  ( -56.48582580120558561, -40.00000000000000000, -9.153146818113723882 ) ) ;
#19219 = CARTESIAN_POINT ( 'NONE',  ( 199.9999999999999432, -14.29115147104986860, -12.53286550942210198 ) ) ;
#19220 = EDGE_CURVE ( 'NONE', #19936, #6393, #5604, .T. ) ;
#19221 = DIRECTION ( 'NONE',  ( -1.836970198721030181E-16, -1.000000000000000000, 0.000000000000000000 ) ) ;
#19222 = CARTESIAN_POINT ( 'NONE',  ( -30.26275506840324070, 1.198031551616030033, -1.198031551616006496 ) ) ;
#19223 = CARTESIAN_POINT ( 'NONE',  ( 200.0000000000000000, -14.14213562373122457, 42.42640687119282461 ) ) ;
#19224 = CARTESIAN_POINT ( 'NONE',  ( -397.9898987322331436, -3.637015436189069562E-14, 0.000000000000000000 ) ) ;
#19225 = CARTESIAN_POINT ( 'NONE',  ( -100.7734535825088358, 1.654174317907124744E-13, -17.32597176626811120 ) ) ;
#19226 = CARTESIAN_POINT ( 'NONE',  ( -93.02511667906880177, -8.169918093965820916, 20.82219708225673571 ) ) ;
#19227 = CARTESIAN_POINT ( 'NONE',  ( 14.38125909742182884, -55.17850393974264733, -40.00000000000002132 ) ) ;
#19228 = CARTESIAN_POINT ( 'NONE',  ( 4.995406935893301537, -10.78321810390187530, 67.35176059882529387 ) ) ;
#19229 = CARTESIAN_POINT ( 'NONE',  ( 163.1118516004056573, 27.26290988616875310, 0.000000000000000000 ) ) ;
#19231 = CARTESIAN_POINT ( 'NONE',  ( -56.48582580120560692, 40.00000000000004263, -9.153146818113443217 ) ) ;
#19230 = CARTESIAN_POINT ( 'NONE',  ( 91.82158438592158234, -12.16597498399995203, -44.40256751092347542 ) ) ;
#19232 = CARTESIAN_POINT ( 'NONE',  ( 130.8568914410475088, -34.05028731879786363, -40.00000000000002132 ) ) ;
#19233 = CARTESIAN_POINT ( 'NONE',  ( -198.0356074513804572, -17.40982414986482141, 39.15871834505909987 ) ) ;
#19234 = CARTESIAN_POINT ( 'NONE',  ( 0.2972598230769930017, 14.33493731733933352, 40.00000000000002132 ) ) ;
#19235 = ORIENTED_EDGE ( 'NONE', *, *, #5121, .F. ) ;
#19236 = CARTESIAN_POINT ( 'NONE',  ( 2.303792037518819669, -44.43800799079054542, 18.40682559463526502 ) ) ;
#19237 = CARTESIAN_POINT ( 'NONE',  ( 136.1360204305621551, -35.03383547441293899, -40.00000000000002132 ) ) ;
#19238 = CARTESIAN_POINT ( 'NONE',  ( -190.0000000000000284, -82.49999999999991473, -52.49999999999977973 ) ) ;
#19239 = ADVANCED_FACE ( 'NONE', ( #12980 ), #4187, .T. ) ;
#19240 = CARTESIAN_POINT ( 'NONE',  ( 163.1118516004056573, 9.006482792069629539, 9.006482792069634868 ) ) ;
#19241 = CARTESIAN_POINT ( 'NONE',  ( 151.7948205124836250, 1.439163438361279259E-13, -33.23291073765553705 ) ) ;
#19242 = CARTESIAN_POINT ( 'NONE',  ( -210.0000000000000284, 0.000000000000000000, 0.000000000000000000 ) ) ;
#19243 = CARTESIAN_POINT ( 'NONE',  ( -70.28815428469411586, 9.450978466794646593, -22.81668038993611347 ) ) ;
#19244 = CARTESIAN_POINT ( 'NONE',  ( 199.9999999999996589, -3.408648353384132079, 18.70401797595889448 ) ) ;
#19245 = EDGE_CURVE ( 'NONE', #16255, #3931, #5038, .T. ) ;
#19246 = CARTESIAN_POINT ( 'NONE',  ( 184.8905102610680444, 13.49065550809757497, 43.07788698682593065 ) ) ;
#19247 = ADVANCED_FACE ( 'NONE', ( #23578 ), #21582, .T. ) ;
#19248 = CARTESIAN_POINT ( 'NONE',  ( -82.26533530497842150, 5.042645448768844574, -19.58509566191921181 ) ) ;
#19249 = CARTESIAN_POINT ( 'NONE',  ( 199.9999999999999432, -14.14213562373115884, 14.14213562373085153 ) ) ;
#19250 = CARTESIAN_POINT ( 'NONE',  ( -266.9101291198153376, 0.000000000000000000, -44.99999999999997158 ) ) ;
#19251 = PRODUCT_DEFINITION_CONTEXT ( 'detailed design', #19366, 'design' ) ;
#19252 = CARTESIAN_POINT ( 'NONE',  ( -280.0000000000000568, 42.42640687119274645, 14.14213562373118194 ) ) ;
#19253 = LINE ( 'NONE', #21384, #10418 ) ;
#19254 = CARTESIAN_POINT ( 'NONE',  ( 0.2972598230769976091, -10.13633138497465147, -10.13633138497482733 ) ) ;
#19256 = CARTESIAN_POINT ( 'NONE',  ( 136.1360204305621266, 3.511608612530757068, -3.511608612530642937 ) ) ;
#19255 = CARTESIAN_POINT ( 'NONE',  ( -197.6433718613433825, 18.53520099273998412, -44.74793361789878787 ) ) ;
#19257 = CARTESIAN_POINT ( 'NONE',  ( -198.0356074513804572, 39.15871834505956173, -39.15871834505865223 ) ) ;
#19258 = CARTESIAN_POINT ( 'NONE',  ( -259.2033419157646676, -9.517827891722680178, 0.000000000000000000 ) ) ;
#19259 = CARTESIAN_POINT ( 'NONE',  ( 146.6084372240433709, 32.08495691632064961, -24.48358557860320417 ) ) ;
#19260 = DIRECTION ( 'NONE',  ( -1.000000000000000000, -1.836970198721030181E-16, -2.465190328815661892E-32 ) ) ;
#19261 = CARTESIAN_POINT ( 'NONE',  ( -91.56559293963834989, -40.53558337403692491, 16.03295912088671571 ) ) ;
#19262 = ORIENTED_EDGE ( 'NONE', *, *, #2687, .F. ) ;
#19263 = CARTESIAN_POINT ( 'NONE',  ( 130.8568914410475372, 4.207082182992862407, 4.207082182992856190 ) ) ;
#19264 = CARTESIAN_POINT ( 'NONE',  ( -105.4741150117382773, -19.77569912955116749, -7.943527260750395946 ) ) ;
#19265 = CARTESIAN_POINT ( 'NONE',  ( 22.72189371635424138, 23.48424859981869517, 43.05215026464263417 ) ) ;
#19266 = CARTESIAN_POINT ( 'NONE',  ( -47.30403195807869565, -30.40121262112982237, -12.59259458005243282 ) ) ;
#19267 = ORIENTED_EDGE ( 'NONE', *, *, #16697, .T. ) ;
#19268 = CARTESIAN_POINT ( 'NONE',  ( -129.2920181225733813, -25.26067667731744848, 10.46331487444209074 ) ) ;
#19269 = CARTESIAN_POINT ( 'NONE',  ( 199.9999999999998295, 1.074487055219422560, -18.97158139261448540 ) ) ;
#19270 = CARTESIAN_POINT ( 'NONE',  ( 22.72611120194076761, -17.88893075486376105, 43.18769924474467814 ) ) ;
#19271 = CARTESIAN_POINT ( 'NONE',  ( 98.29820294270297154, 18.47759065022021474, -7.653668647299666894 ) ) ;
#19272 = CARTESIAN_POINT ( 'NONE',  ( 199.0097993503064515, 19.72850438885342328, 3.281923459752313921 ) ) ;
#19273 = CARTESIAN_POINT ( 'NONE',  ( -86.96347745069645896, -12.89780903124443689, 43.67073346367968156 ) ) ;
#19274 = CARTESIAN_POINT ( 'NONE',  ( -135.8532207217289738, 7.002209520526292428E-15, -9.153146818113572891 ) ) ;
#19275 = CARTESIAN_POINT ( 'NONE',  ( -82.28158553065811986, -6.254237062281328363, 19.22561360847505085 ) ) ;
#19276 = CARTESIAN_POINT ( 'NONE',  ( -362.0709805440841365, -4.857225732735059864E-14, 0.000000000000000000 ) ) ;
#19277 = CARTESIAN_POINT ( 'NONE',  ( -56.48582580120558561, -30.84685318188645553, -40.00000000000002132 ) ) ;
#19279 = LINE ( 'NONE', #16894, #14269 ) ;
#19278 = CARTESIAN_POINT ( 'NONE',  ( 23.64688638900278050, -23.28414885118052524, -42.77321027809716725 ) ) ;
#19280 = CARTESIAN_POINT ( 'NONE',  ( 151.7948205124835681, 33.23291073765556547, 40.00000000000002132 ) ) ;
#19281 = CARTESIAN_POINT ( 'NONE',  ( 0.2972598230769976091, -10.13633138497479180, 10.13633138497468522 ) ) ;
#19282 = CARTESIAN_POINT ( 'NONE',  ( -213.1075012329537230, 40.00000000000055422, -53.71589010953623244 ) ) ;
#19283 = CARTESIAN_POINT ( 'NONE',  ( 190.0000000000000000, -66.50000000000001421, 66.50000000000005684 ) ) ;
#19284 = CARTESIAN_POINT ( 'NONE',  ( 170.2234770963711128, 1.955190573858485757E-13, -15.44714144992816074 ) ) ;
#19285 = CARTESIAN_POINT ( 'NONE',  ( 130.8879939280389237, -29.49769239790404640, -12.21834424992166923 ) ) ;
#19286 = CARTESIAN_POINT ( 'NONE',  ( 146.6084372240433993, -24.48358557860353457, 24.48358557860296258 ) ) ;
#19287 = CARTESIAN_POINT ( 'NONE',  ( -91.56559293963834989, 16.03295912088683650, 40.53558337403684675 ) ) ;
#19288 = VERTEX_POINT ( 'NONE', #19705 ) ;
#19290 = CARTESIAN_POINT ( 'NONE',  ( 11.38508063392656666, 49.30460303390188415, -14.17561098847166967 ) ) ;
#19289 = CARTESIAN_POINT ( 'NONE',  ( 199.9999999999999432, 14.14213562373093680, 14.14213562373114641 ) ) ;
#19291 = CARTESIAN_POINT ( 'NONE',  ( 146.6084372240433709, 34.62501878078307982, 40.00000000000002132 ) ) ;
#19292 = FILL_AREA_STYLE_COLOUR ( '', #4704 ) ;
#19293 = CARTESIAN_POINT ( 'NONE',  ( 160.9163046357249129, -205.7889608577475542, 49.61140153332248559 ) ) ;
#19294 = DIRECTION ( 'NONE',  ( 1.000000000000000000, 1.836970198721036590E-16, 1.836970198721030181E-16 ) ) ;
#19295 = ORIENTED_EDGE ( 'NONE', *, *, #4520, .F. ) ;
#19296 = VERTEX_POINT ( 'NONE', #13091 ) ;
#19297 = CARTESIAN_POINT ( 'NONE',  ( -280.0000000000000000, 14.14213562373098299, -14.14213562373088706 ) ) ;
#19298 = CARTESIAN_POINT ( 'NONE',  ( 98.29820294267321401, -18.47759065023119973, -7.653668647304142425 ) ) ;
#19299 = VERTEX_POINT ( 'NONE', #17329 ) ;
#19300 = ORIENTED_EDGE ( 'NONE', *, *, #6706, .T. ) ;
#19301 = CARTESIAN_POINT ( 'NONE',  ( 200.0000000000001421, -0.6349535514222880428, 19.00853270881595591 ) ) ;
#19302 = FACE_OUTER_BOUND ( 'NONE', #14055, .T. ) ;
#19303 = CARTESIAN_POINT ( 'NONE',  ( -56.48582580120559982, -34.75652343174615311, 21.81201906317766870 ) ) ;
#19304 = CARTESIAN_POINT ( 'NONE',  ( -199.9999999999998010, 24.82633483071100500, -44.86878812508844305 ) ) ;
#19305 = CARTESIAN_POINT ( 'NONE',  ( -198.0356074513804572, 39.99999999999992895, 15.37879056873084771 ) ) ;
#19306 = CARTESIAN_POINT ( 'NONE',  ( -199.9999999999999432, -45.24754806068997937, 21.40989205436307685 ) ) ;
#19307 = CARTESIAN_POINT ( 'NONE',  ( -626.9846540392142060, 90.00000000000000000, -60.00000000000000000 ) ) ;
#19308 = EDGE_CURVE ( 'NONE', #16073, #24029, #14115, .T. ) ;
#19309 = CARTESIAN_POINT ( 'NONE',  ( 184.8905102610680444, 2.362515690532070066E-13, -19.07866798485558490 ) ) ;
#19310 = CARTESIAN_POINT ( 'NONE',  ( -56.48582580120558561, 3.151766524733697544E-13, -30.84685318188644132 ) ) ;
#19311 = CARTESIAN_POINT ( 'NONE',  ( -77.56416967749056823, 16.64106674400274954, 14.59748372935088412 ) ) ;
#19312 = CARTESIAN_POINT ( 'NONE',  ( 163.1118516004056573, -9.006482792073960297, -47.56205970284963769 ) ) ;
#19313 = CARTESIAN_POINT ( 'NONE',  ( 190.0000000000000000, -35.78896085774750446, -82.49999999999998579 ) ) ;
#19314 = CARTESIAN_POINT ( 'NONE',  ( -195.1686598215018762, 24.52826087131413502, 44.46432177480297554 ) ) ;
#19315 = CARTESIAN_POINT ( 'NONE',  ( 144.9504669809063557, 30.13886470195693335, 12.48392651407845122 ) ) ;
#19316 =( BOUNDED_SURFACE ( )  B_SPLINE_SURFACE ( 3, 3, ( 
 ( #815, #22899, #12780, #6265, #4289, #12378, #20506, #8386, #4413, #11171, #2940, #3541, #7171, #13174, #19763, #1069, #15288, #13771, #6917, #15167, #5801, #17289, #11641, #19286, #24022, #4943, #11783, #1687, #25166, #13049 ),
 ( #23292, #21295, #13908, #3069, #25423, #15034, #20041, #9178, #23418, #5536, #15895, #21167, #13642, #11050, #23164, #21898, #7050, #3675, #19161, #1554, #21768, #19903, #9791, #17894, #946, #9659, #8921, #26042, #9054, #17763 ),
 ( #11919, #17159, #7779, #25905, #25293, #22043, #5068, #7646, #15760, #3816, #17031, #23889, #5665, #6324, #14310, #12050, #2344, #10059, #2217, #24431, #18295, #8319, #16572, #22309, #10456, #18569, #24306, #349, #24568, #1951 ),
 ( #14446, #22178, #16444, #26312, #18028, #8191, #18165, #10326, #24703, #14044, #81, #8055, #10192, #14175, #18435, #210, #3952, #4085, #6073, #14573, #16171, #5937, #8453, #16307, #22702, #12186, #20308, #22573, #6457, #4477 ),
 ( #4351, #12579, #2085, #6198, #12443, #22444, #4224, #12313, #20439, #20572, #1820, #9922, #26178, #7918, #16035, #24161, #20169, #485, #25363, #25231, #19230, #4747, #17098, #6983, #12853, #15098, #2884, #7118, #14707, #15228 ),
 ( #617, #17224, #2752, #23106, #20971, #9113, #16702, #23232, #13114, #10587, #24834, #6586, #5136, #18839, #23359, #8857, #18702, #20709, #8723, #22968, #8592, #2614, #22840, #5009, #4615, #2475, #3009, #12711, #21235, #19101 ),
 ( #12982, #10855, #11116, #1010, #20839, #10727, #6723, #16841, #24974, #14835, #10992, #885, #18973, #753, #16969, #25105, #6854, #14971, #4878, #21104, #8994, #17478, #7366, #3648, #15604, #5510, #21482, #1526, #19354, #17866 ) ),
 .UNSPECIFIED., .T., .F., .T. ) 
 B_SPLINE_SURFACE_WITH_KNOTS ( ( 4, 3, 4 ),
 ( 4, 2, 2, 2, 2, 2, 2, 2, 2, 2, 2, 2, 2, 2, 4 ),
 ( 0.000000000000000000, 0.5000000000000000000, 1.000000000000000000 ),
 ( 0.000000000000000000, 0.1357259735107005372, 0.1651108541090157700, 0.1944957347073310028, 0.3598804999793158710, 0.3867117631979620773, 0.4135430264166082281, 0.5789277916885930964, 0.6062785021374117456, 0.6336292125862302838, 0.8508620842112317728, 0.8814014469398914198, 0.9119408096685510667, 0.9559704048342755334, 1.000000000000000000 ),
 .UNSPECIFIED. ) 
 GEOMETRIC_REPRESENTATION_ITEM ( )  RATIONAL_B_SPLINE_SURFACE ( (
 ( 1.000000000000000000, 1.000000000000000000, 1.000000000000000000, 1.000000000000000000, 1.000000000000000000, 1.000000000000000000, 1.000000000000000000, 1.000000000000000000, 1.000000000000000000, 1.000000000000000000, 1.000000000000000000, 1.000000000000000000, 1.000000000000000000, 1.000000000000000000, 1.000000000000000000, 1.000000000000000000, 1.000000000000000000, 1.000000000000000000, 1.000000000000000000, 1.000000000000000000, 1.000000000000000000, 1.000000000000000000, 1.000000000000000000, 1.000000000000000000, 1.000000000000000000, 1.000000000000000000, 1.000000000000000000, 1.000000000000000000, 1.000000000000000000, 1.000000000000000000),
 ( 0.3333333333333333703, 0.3333333333333333703, 0.3333333333333333703, 0.3333333333333333703, 0.3333333333333333703, 0.3333333333333333703, 0.3333333333333333703, 0.3333333333333333703, 0.3333333333333333703, 0.3333333333333333703, 0.3333333333333333703, 0.3333333333333333703, 0.3333333333333333703, 0.3333333333333333703, 0.3333333333333333703, 0.3333333333333333703, 0.3333333333333333703, 0.3333333333333333703, 0.3333333333333333703, 0.3333333333333333703, 0.3333333333333333703, 0.3333333333333333703, 0.3333333333333333703, 0.3333333333333333703, 0.3333333333333333703, 0.3333333333333333703, 0.3333333333333333703, 0.3333333333333333703, 0.3333333333333333703, 0.3333333333333333703),
 ( 0.3333333333333333703, 0.3333333333333333703, 0.3333333333333333703, 0.3333333333333333703, 0.3333333333333333703, 0.3333333333333333703, 0.3333333333333333703, 0.3333333333333333703, 0.3333333333333333703, 0.3333333333333333703, 0.3333333333333333703, 0.3333333333333333703, 0.3333333333333333703, 0.3333333333333333703, 0.3333333333333333703, 0.3333333333333333703, 0.3333333333333333703, 0.3333333333333333703, 0.3333333333333333703, 0.3333333333333333703, 0.3333333333333333703, 0.3333333333333333703, 0.3333333333333333703, 0.3333333333333333703, 0.3333333333333333703, 0.3333333333333333703, 0.3333333333333333703, 0.3333333333333333703, 0.3333333333333333703, 0.3333333333333333703),
 ( 1.000000000000000000, 1.000000000000000000, 1.000000000000000000, 1.000000000000000000, 1.000000000000000000, 1.000000000000000000, 1.000000000000000000, 1.000000000000000000, 1.000000000000000000, 1.000000000000000000, 1.000000000000000000, 1.000000000000000000, 1.000000000000000000, 1.000000000000000000, 1.000000000000000000, 1.000000000000000000, 1.000000000000000000, 1.000000000000000000, 1.000000000000000000, 1.000000000000000000, 1.000000000000000000, 1.000000000000000000, 1.000000000000000000, 1.000000000000000000, 1.000000000000000000, 1.000000000000000000, 1.000000000000000000, 1.000000000000000000, 1.000000000000000000, 1.000000000000000000),
 ( 0.3333333333333333703, 0.3333333333333333703, 0.3333333333333333703, 0.3333333333333333703, 0.3333333333333333703, 0.3333333333333333703, 0.3333333333333333703, 0.3333333333333333703, 0.3333333333333333703, 0.3333333333333333703, 0.3333333333333333703, 0.3333333333333333703, 0.3333333333333333703, 0.3333333333333333703, 0.3333333333333333703, 0.3333333333333333703, 0.3333333333333333703, 0.3333333333333333703, 0.3333333333333333703, 0.3333333333333333703, 0.3333333333333333703, 0.3333333333333333703, 0.3333333333333333703, 0.3333333333333333703, 0.3333333333333333703, 0.3333333333333333703, 0.3333333333333333703, 0.3333333333333333703, 0.3333333333333333703, 0.3333333333333333703),
 ( 0.3333333333333333703, 0.3333333333333333703, 0.3333333333333333703, 0.3333333333333333703, 0.3333333333333333703, 0.3333333333333333703, 0.3333333333333333703, 0.3333333333333333703, 0.3333333333333333703, 0.3333333333333333703, 0.3333333333333333703, 0.3333333333333333703, 0.3333333333333333703, 0.3333333333333333703, 0.3333333333333333703, 0.3333333333333333703, 0.3333333333333333703, 0.3333333333333333703, 0.3333333333333333703, 0.3333333333333333703, 0.3333333333333333703, 0.3333333333333333703, 0.3333333333333333703, 0.3333333333333333703, 0.3333333333333333703, 0.3333333333333333703, 0.3333333333333333703, 0.3333333333333333703, 0.3333333333333333703, 0.3333333333333333703),
 ( 1.000000000000000000, 1.000000000000000000, 1.000000000000000000, 1.000000000000000000, 1.000000000000000000, 1.000000000000000000, 1.000000000000000000, 1.000000000000000000, 1.000000000000000000, 1.000000000000000000, 1.000000000000000000, 1.000000000000000000, 1.000000000000000000, 1.000000000000000000, 1.000000000000000000, 1.000000000000000000, 1.000000000000000000, 1.000000000000000000, 1.000000000000000000, 1.000000000000000000, 1.000000000000000000, 1.000000000000000000, 1.000000000000000000, 1.000000000000000000, 1.000000000000000000, 1.000000000000000000, 1.000000000000000000, 1.000000000000000000, 1.000000000000000000, 1.000000000000000000) ) ) 
 REPRESENTATION_ITEM ( '' )  SURFACE ( )  );
#19317 = LINE ( 'NONE', #25581, #3870 ) ;
#19318 = CARTESIAN_POINT ( 'NONE',  ( -162.0762913951020892, -1.198031840385783919, 1.198031840385741731 ) ) ;
#19319 = CARTESIAN_POINT ( 'NONE',  ( -82.24857225180262787, -11.87278284862285105, 16.34324723836312998 ) ) ;
#19320 = CARTESIAN_POINT ( 'NONE',  ( -162.0762913951021176, 1.198031840315997298, 57.76657433523996588 ) ) ;
#19321 = CARTESIAN_POINT ( 'NONE',  ( 19.06497207195982568, -38.31983398719592770, -38.31983398719660272 ) ) ;
#19322 = CARTESIAN_POINT ( 'NONE',  ( -187.3037411061693263, -13.75782484033365449, -46.64555264106012800 ) ) ;
#19323 = CARTESIAN_POINT ( 'NONE',  ( 5.009866156928151071, 24.71463403307581430, 44.71726210619342368 ) ) ;
#19324 = EDGE_LOOP ( 'NONE', ( #116, #14947, #2354, #20882 ) ) ;
#19325 = CARTESIAN_POINT ( 'NONE',  ( 192.4448373802100889, 14.14213562370330379, -14.14213562370292365 ) ) ;
#19326 = CARTESIAN_POINT ( 'NONE',  ( -210.0000000000000284, -71.50000000000002842, -66.50000000000005684 ) ) ;
#19327 = CARTESIAN_POINT ( 'NONE',  ( -623.9547998620685121, 28.43996653510315653, 34.87374174356184398 ) ) ;
#19328 = ORIENTED_EDGE ( 'NONE', *, *, #9622, .F. ) ;
#19329 = CARTESIAN_POINT ( 'NONE',  ( -30.26275506840324070, 1.218738420030236455E-14, -1.694272468446259783 ) ) ;
#19330 = CARTESIAN_POINT ( 'NONE',  ( 199.0238548747951484, -20.00383568556590674, 1.381665862992945915 ) ) ;
#19331 = CARTESIAN_POINT ( 'NONE',  ( -296.0000000000000000, -4.857225732735059864E-14, 20.53474504356812247 ) ) ;
#19332 = ORIENTED_EDGE ( 'NONE', *, *, #11709, .F. ) ;
#19333 = VERTEX_POINT ( 'NONE', #986 ) ;
#19334 = CARTESIAN_POINT ( 'NONE',  ( 57.59792236341147031, 37.56421063658187620, 40.00000000000002132 ) ) ;
#19335 = CARTESIAN_POINT ( 'NONE',  ( 192.4448373802100889, 14.14213562375893574, -14.14213562375874922 ) ) ;
#19336 = CARTESIAN_POINT ( 'NONE',  ( 14.38125909742180220, 39.99999999999997158, 15.17850393972647716 ) ) ;
#19337 = DIRECTION ( 'NONE',  ( -1.000000000000000000, 1.836970198721030181E-16, 0.000000000000000000 ) ) ;
#19338 = AXIS2_PLACEMENT_3D ( 'NONE', #23794, #19545, #9435 ) ;
#19339 = PRODUCT_DEFINITION_CONTEXT ( 'detailed design', #21585, 'design' ) ;
#19340 = CARTESIAN_POINT ( 'NONE',  ( -77.90255099906859471, -8.644468104251766150, 20.04994828524300843 ) ) ;
#19341 = CARTESIAN_POINT ( 'NONE',  ( -238.4067589809705794, -4.716212492215116094E-14, 0.9644942799825824142 ) ) ;
#19342 = CARTESIAN_POINT ( 'NONE',  ( 200.0000000000000568, -17.44062545528135999, -7.562669404541021656 ) ) ;
#19343 = MECHANICAL_DESIGN_GEOMETRIC_PRESENTATION_REPRESENTATION (  '', ( #11689 ), #15105 ) ;
#19344 = VECTOR ( 'NONE', #10648, 1000.000000000000114 ) ;
#19345 = CARTESIAN_POINT ( 'NONE',  ( -86.95455990305946159, 9.640326247162176898, 19.12039797428042220 ) ) ;
#19346 = CARTESIAN_POINT ( 'NONE',  ( 163.1118516004056573, -19.27778845538787422, 19.27778845538743724 ) ) ;
#19347 = CARTESIAN_POINT ( 'NONE',  ( 184.8905102610680444, 14.79361573936375507, 14.79361573936398067 ) ) ;
#19348 = CARTESIAN_POINT ( 'NONE',  ( -210.0000000000000284, -61.50000000000001421, 66.50000000000005684 ) ) ;
#19349 = CARTESIAN_POINT ( 'NONE',  ( 192.4448373802101173, -39.99999999999977973, -19.99999999996102673 ) ) ;
#19350 = DIRECTION ( 'NONE',  ( 0.000000000000000000, 1.000000000000000000, 0.000000000000000000 ) ) ;
#19351 = CARTESIAN_POINT ( 'NONE',  ( -30.26275506840324425, -1.694272468446265334, -40.00000000000002132 ) ) ;
#19352 = CARTESIAN_POINT ( 'NONE',  ( -259.2033419157646676, 6.730120644403521979, -6.730120644403498886 ) ) ;
#19353 = CARTESIAN_POINT ( 'NONE',  ( -30.26275506840324425, -1.694272468446265334, -40.00000000000002132 ) ) ;
#19355 = CARTESIAN_POINT ( 'NONE',  ( 146.6084372240433993, 1.478241399363601114E-13, -34.62501878078305850 ) ) ;
#19354 = CARTESIAN_POINT ( 'NONE',  ( 192.4448373802100889, -14.14213562375896061, 14.14213562375865330 ) ) ;
#19356 = CARTESIAN_POINT ( 'NONE',  ( -56.48582580120559271, -9.153146818113595984, 0.000000000000000000 ) ) ;
#19357 = CARTESIAN_POINT ( 'NONE',  ( -56.48582580120559982, 50.09629031063966664, -6.472252184284094767 ) ) ;
#19358 = CARTESIAN_POINT ( 'NONE',  ( -198.0356074513804572, 55.37879056873070027, 2.449293598294708485E-15 ) ) ;
#19359 = ORIENTED_EDGE ( 'NONE', *, *, #5571, .T. ) ;
#19360 = CARTESIAN_POINT ( 'NONE',  ( 22.90311673804475845, -46.98314248934332227, 13.82691048573679815 ) ) ;
#19361 = CIRCLE ( 'NONE', #1103, 29.99999999999999289 ) ;
#19362 = CARTESIAN_POINT ( 'NONE',  ( -4.039451493210497901, 23.44932283416708074, -43.00522595893983890 ) ) ;
#19363 = CARTESIAN_POINT ( 'NONE',  ( 170.2234770963711128, -17.36149277826995885, 39.20704971665388427 ) ) ;
#19364 = CARTESIAN_POINT ( 'NONE',  ( -135.8532207217289738, 7.002209520526292428E-15, -9.153146818113572891 ) ) ;
#19365 = CARTESIAN_POINT ( 'NONE',  ( -82.23936494317537438, 20.15025730830772233, 1.484621625134467937 ) ) ;
#19366 = APPLICATION_CONTEXT ( 'automotive_design' ) ;
#19367 = AXIS2_PLACEMENT_3D ( 'NONE', #23908, #15780, #11663 ) ;
#19368 = VECTOR ( 'NONE', #11551, 1000.000000000000000 ) ;
#19369 = CARTESIAN_POINT ( 'NONE',  ( 18.89824444022307048, -14.00990882958388184, -48.20791849611967450 ) ) ;
#19370 = CARTESIAN_POINT ( 'NONE',  ( 200.0000000000002842, -5.234650960127995134, 18.27551028936266775 ) ) ;
#19371 = CARTESIAN_POINT ( 'NONE',  ( -653.7294268227522025, 37.61632567776710800, -13.73334781262508564 ) ) ;
#19372 = CARTESIAN_POINT ( 'NONE',  ( -82.29192131167501145, -6.849507299441772723, -18.98456886706201274 ) ) ;
#19373 = CARTESIAN_POINT ( 'NONE',  ( 170.2234770963711128, 10.92277846919147066, 45.64576402573197811 ) ) ;
#19374 = CARTESIAN_POINT ( 'NONE',  ( 163.1118516004056573, 19.27778845539265618, -37.29075403953135037 ) ) ;
#19375 = CARTESIAN_POINT ( 'NONE',  ( 0.2972598230769923355, 18.14793986248697166, 38.42060263243675422 ) ) ;
#19376 = DIRECTION ( 'NONE',  ( -0.01051738777840964360, -0.3656191333258750342, -0.9307051272558644062 ) ) ;
#19377 = CARTESIAN_POINT ( 'NONE',  ( -100.7734535825088358, -12.25131212657475643, -12.25131212657495539 ) ) ;
#19378 = VECTOR ( 'NONE', #9328, 1000.000000000000000 ) ;
#19380 = CARTESIAN_POINT ( 'NONE',  ( 200.0000000000000000, -42.42640687119272513, -14.14213562373140753 ) ) ;
#19379 = CARTESIAN_POINT ( 'NONE',  ( 19.06497207195980792, 18.24870850772790831, -38.31983398719609824 ) ) ;
#19381 = CARTESIAN_POINT ( 'NONE',  ( -105.3755690713226727, 12.89780903124418998, -12.89780903124389155 ) ) ;
#19382 = CARTESIAN_POINT ( 'NONE',  ( -280.0000000000000000, -20.00000000000006750, 0.000000000000000000 ) ) ;
#19383 = CARTESIAN_POINT ( 'NONE',  ( 170.2234770963711128, -17.36149277826985937, -17.36149277826995174 ) ) ;
#19384 = EDGE_CURVE ( 'NONE', #15935, #6279, #958, .T. ) ;
#19385 = CARTESIAN_POINT ( 'NONE',  ( -265.0000000000000000, -4.867971026610730343E-14, -6.532754371361504014E-30 ) ) ;
#19386 = CARTESIAN_POINT ( 'NONE',  ( 184.8905102610680444, -41.77492675556007384, 14.79361573936348684 ) ) ;
#19387 = EDGE_CURVE ( 'NONE', #24980, #23006, #9218, .T. ) ;
#19388 = CARTESIAN_POINT ( 'NONE',  ( -121.8281105898230692, 22.46071553299150381, -10.16551987237939336 ) ) ;
#19389 = ORIENTED_EDGE ( 'NONE', *, *, #11896, .F. ) ;
#19390 = CIRCLE ( 'NONE', #12156, 4.999999999999962697 ) ;
#19391 = CARTESIAN_POINT ( 'NONE',  ( -56.48582580120559982, 50.09629031063966664, -6.472252184284094767 ) ) ;
#19392 = CARTESIAN_POINT ( 'NONE',  ( -28.75808802591298630, 38.33175228464058648, -12.03522322449772552 ) ) ;
#19393 = CARTESIAN_POINT ( 'NONE',  ( 11.28112952480474895, 18.58737866930062665, 44.87390167243342631 ) ) ;
#19394 = CARTESIAN_POINT ( 'NONE',  ( -24.53392603777601977, -39.81639166317236800, -12.34411287782893041 ) ) ;
#19395 = EDGE_CURVE ( 'NONE', #10429, #9342, #9091, .T. ) ;
#19396 = ADVANCED_FACE ( 'NONE', ( #1239 ), #15329, .F. ) ;
#19397 = ORIENTED_EDGE ( 'NONE', *, *, #1492, .T. ) ;
#19398 = CARTESIAN_POINT ( 'NONE',  ( -151.4802849348335769, -33.96623543976281212, 11.09498666344389761 ) ) ;
#19399 = CARTESIAN_POINT ( 'NONE',  ( 199.9999999999998863, -9.504749071264818383, -16.45922038047892144 ) ) ;
#19400 = CIRCLE ( 'NONE', #13862, 5.000000000000004441 ) ;
#19401 = CARTESIAN_POINT ( 'NONE',  ( 23.10188454848158557, -13.81611343686630100, 46.91040837924295204 ) ) ;
#19402 = FACE_OUTER_BOUND ( 'NONE', #12521, .T. ) ;
#19403 = CARTESIAN_POINT ( 'NONE',  ( 199.0070327355206246, 4.219744681889460836, -19.54794762927634366 ) ) ;
#19404 = FACE_OUTER_BOUND ( 'NONE', #23454, .T. ) ;
#19405 = CARTESIAN_POINT ( 'NONE',  ( 4.995406935893290878, -5.232665749138292703E-14, 15.24977328854832592 ) ) ;
#19406 = CARTESIAN_POINT ( 'NONE',  ( -198.0356074513804572, -9.007331120208026888E-14, 15.37879056873070560 ) ) ;
#19407 = CARTESIAN_POINT ( 'NONE',  ( 23.37394308801976450, 46.80823611210215063, -13.80096434448263309 ) ) ;
#19408 = CARTESIAN_POINT ( 'NONE',  ( 163.1118516004056573, -12.73709011382471878, -40.00000000000002132 ) ) ;
#19410 = CARTESIAN_POINT ( 'NONE',  ( -280.0000000000000000, -20.00000000000006750, 0.000000000000000000 ) ) ;
#19409 = CARTESIAN_POINT ( 'NONE',  ( -184.9730489280930215, 22.80026000644289752, -42.02334742179726135 ) ) ;
#19411 = CARTESIAN_POINT ( 'NONE',  ( -56.48582580120558561, -30.84685318188645908, 40.00000000000002132 ) ) ;
#19412 = CARTESIAN_POINT ( 'NONE',  ( 130.8568914410475372, 24.07718906447243867, -24.07718906447216156 ) ) ;
#19413 = CARTESIAN_POINT ( 'NONE',  ( 130.8568914410475088, 40.00000000000011369, -5.949712681206269949 ) ) ;
#19414 = CARTESIAN_POINT ( 'NONE',  ( 146.6084372240433709, -40.00000000000036238, 34.62501878078263218 ) ) ;
#19415 = DIRECTION ( 'NONE',  ( 1.000000000000000000, -1.937599346585394162E-16, -0.000000000000000000 ) ) ;
#19416 = EDGE_LOOP ( 'NONE', ( #20953, #23214 ) ) ;
#19418 = CARTESIAN_POINT ( 'NONE',  ( 9.028290303185290355, 44.88859993222921929, -18.59346688788140867 ) ) ;
#19417 = CARTESIAN_POINT ( 'NONE',  ( 14.38125909742181285, -10.73282306404712472, -10.73282306404731301 ) ) ;
#19419 = CARTESIAN_POINT ( 'NONE',  ( 184.8905102610680444, -19.07866798485554938, 40.00000000000002132 ) ) ;
#19420 =( NAMED_UNIT ( * ) SI_UNIT ( $, .STERADIAN. ) SOLID_ANGLE_UNIT ( ) );
#19421 = CARTESIAN_POINT ( 'NONE',  ( -193.3669111531376075, 44.23532963564892384, -18.32287347112458065 ) ) ;
#19422 = CARTESIAN_POINT ( 'NONE',  ( 0.000000000000000000, 0.000000000000000000, 0.000000000000000000 ) ) ;
#19423 = ORIENTED_EDGE ( 'NONE', *, *, #14494, .F. ) ;
#19424 = VERTEX_POINT ( 'NONE', #4984 ) ;
#19425 = CARTESIAN_POINT ( 'NONE',  ( -213.1075012329537230, -9.698598906450557777, 9.698598906450415669 ) ) ;
#19426 = CARTESIAN_POINT ( 'NONE',  ( 83.11963132847050417, -23.63628489299456348, -10.90660717668977497 ) ) ;
#19427 = EDGE_LOOP ( 'NONE', ( #21672, #23143, #3415, #19045 ) ) ;
#19428 = VERTEX_POINT ( 'NONE', #19326 ) ;
#19429 = CARTESIAN_POINT ( 'NONE',  ( 199.0263189878286028, -15.57072488730636017, 12.56115478513486217 ) ) ;
#19430 = DIRECTION ( 'NONE',  ( 0.000000000000000000, 0.3028247695821853491, -0.9530462522498560629 ) ) ;
#19431 = CARTESIAN_POINT ( 'NONE',  ( 0.2972598230769959993, 38.42060263243659080, 38.42060263243672580 ) ) ;
#19432 = DIRECTION ( 'NONE',  ( 0.000000000000000000, 0.9767746502210203907, -0.2142691827715860198 ) ) ;
#19433 = CARTESIAN_POINT ( 'NONE',  ( -105.3755690713226727, 5.661656051307470077E-14, -21.75974354311649961 ) ) ;
#19434 = DIRECTION ( 'NONE',  ( -1.000000000000000000, -1.836970198721030181E-16, -2.465190328815661892E-32 ) ) ;
#19435 = CARTESIAN_POINT ( 'NONE',  ( 200.0000000000000000, -39.99999999999977973, -20.00000000000034817 ) ) ;
#19436 = CARTESIAN_POINT ( 'NONE',  ( -56.48582580120559982, 40.00000000000034106, -30.84685318188602210 ) ) ;
#19437 = CARTESIAN_POINT ( 'NONE',  ( -114.7248266913187678, -17.87714126012797422, 12.97729011816987565 ) ) ;
#19438 = CARTESIAN_POINT ( 'NONE',  ( -135.8532207217289738, -21.81201906317758343, -34.75652343174620995 ) ) ;
#19439 = DIRECTION ( 'NONE',  ( 0.000000000000000000, 1.000000000000000000, 0.000000000000000000 ) ) ;
#19440 = CARTESIAN_POINT ( 'NONE',  ( -194.7885354600661572, 18.40784581029643263, 44.44047100928790428 ) ) ;
#19441 = CARTESIAN_POINT ( 'NONE',  ( 130.1167162091013836, 29.33455044752954777, 12.15076864148460878 ) ) ;
#19442 = CARTESIAN_POINT ( 'NONE',  ( -3.903133374382439236, -47.03983734342246947, 13.83543723413883342 ) ) ;
#19443 = CARTESIAN_POINT ( 'NONE',  ( 136.1360204305621266, 24.77266263493138965, -24.77266263493110188 ) ) ;
#19444 = CARTESIAN_POINT ( 'NONE',  ( -82.24297220891752147, -15.98176361808475576, 12.40742895866242890 ) ) ;
#19445 = CARTESIAN_POINT ( 'NONE',  ( 146.6084372240433709, -52.76785682606516303, 3.800685668858563737 ) ) ;
#19446 = CARTESIAN_POINT ( 'NONE',  ( -280.0000000000000568, -42.42640687119305198, 14.14213562373058686 ) ) ;
#19447 = CARTESIAN_POINT ( 'NONE',  ( -635.2543834470891397, 29.44729488742095924, -34.02929410116306741 ) ) ;
#19448 = CARTESIAN_POINT ( 'NONE',  ( 98.29820294267490510, 4.808046699556526995E-12, 20.00000000000513722 ) ) ;
#19449 = ORIENTED_EDGE ( 'NONE', *, *, #15781, .T. ) ;
#19450 = CARTESIAN_POINT ( 'NONE',  ( -259.2033419157646676, 21.55415060305860209, -21.55415060305812602 ) ) ;
#19451 = CARTESIAN_POINT ( 'NONE',  ( 180.0000000000000000, -71.50000000000002842, -66.50000000000005684 ) ) ;
#19452 = CARTESIAN_POINT ( 'NONE',  ( -28.75791583366072501, 12.03523584680509551, -38.33181286256363052 ) ) ;
#19453 = VERTEX_POINT ( 'NONE', #23334 ) ;
#19454 = CARTESIAN_POINT ( 'NONE',  ( 19.06497207195981147, 1.521599808664285085E-13, -14.19242893257840521 ) ) ;
#19455 = CARTESIAN_POINT ( 'NONE',  ( -4.039451493210490796, -23.44932283416679297, 43.00522595894000943 ) ) ;
#19456 = CARTESIAN_POINT ( 'NONE',  ( -28.75808802781981655, 18.59445401971606060, 35.61482992978285722 ) ) ;
#19457 = VERTEX_POINT ( 'NONE', #23204 ) ;
#19458 = ORIENTED_EDGE ( 'NONE', *, *, #15475, .F. ) ;
#19459 = CARTESIAN_POINT ( 'NONE',  ( 151.7948205124836250, 23.49921654116361225, -23.49921654116333514 ) ) ;
#19460 = ADVANCED_FACE ( 'NONE', ( #25335 ), #23457, .F. ) ;
#19461 = CARTESIAN_POINT ( 'NONE',  ( -100.7734535825088500, 39.99999999999994316, 17.32597176626825686 ) ) ;
#19462 = CARTESIAN_POINT ( 'NONE',  ( -96.94449363886086246, -20.74048850971937696, -8.590991631070833634 ) ) ;
#19463 = CARTESIAN_POINT ( 'NONE',  ( -100.7734535825088358, 12.25131212657497848, -12.25131212657469604 ) ) ;
#19464 =( BOUNDED_SURFACE ( )  B_SPLINE_SURFACE ( 3, 2, ( 
 ( #12282, #2183, #16003 ),
 ( #4050, #3919, #10552 ),
 ( #8157, #12151, #12018 ),
 ( #20274, #18131, #20671 ),
 ( #2052, #26138, #10292 ),
 ( #16135, #16270, #10159 ) ),
 .UNSPECIFIED., .F., .F., .F. ) 
 B_SPLINE_SURFACE_WITH_KNOTS ( ( 4, 2, 4 ),
 ( 3, 3 ),
 ( 0.04143195986180998186, 0.04845790097405862362, 0.05548384208630727232 ),
 ( 0.000000000000000000, 1.000000000000000000 ),
 .UNSPECIFIED. ) 
 GEOMETRIC_REPRESENTATION_ITEM ( )  RATIONAL_B_SPLINE_SURFACE ( (
 ( 1.000000000000000000, 0.9541700777564564584, 1.000000000000000000),
 ( 1.000000000000000000, 0.9520117016566322921, 1.000000000000000000),
 ( 1.000000000000000000, 0.9503157806802187135, 1.000000000000000000),
 ( 1.000000000000000000, 0.9480088156000070487, 1.000000000000000000),
 ( 1.000000000000000000, 0.9474362554095308031, 1.000000000000000000),
 ( 1.000000000000000000, 0.9474350312570029020, 1.000000000000000000) ) ) 
 REPRESENTATION_ITEM ( '' )  SURFACE ( )  );
#19465 = CARTESIAN_POINT ( 'NONE',  ( -162.0762913951021176, -40.00000000000005684, 1.694272876828184504 ) ) ;
#19466 = CARTESIAN_POINT ( 'NONE',  ( 199.9999999999998863, -15.98179559645994097, -10.29177186004950961 ) ) ;
#19467 = EDGE_CURVE ( 'NONE', #22119, #21182, #23067, .T. ) ;
#19468 = DIRECTION ( 'NONE',  ( 0.000000000000000000, 1.000000000000000000, 0.000000000000000000 ) ) ;
#19469 = CARTESIAN_POINT ( 'NONE',  ( 136.1360204305621551, 24.77266263493153176, -31.79587985999237887 ) ) ;
#19470 = LINE ( 'NONE', #1389, #15647 ) ;
#19471 = CARTESIAN_POINT ( 'NONE',  ( -86.96347745069643054, -39.99999999999985079, -18.24025645688394448 ) ) ;
#19472 = CARTESIAN_POINT ( 'NONE',  ( 23.37394308801978582, -46.80823611210187352, -13.80096434448294396 ) ) ;
#19473 = CARTESIAN_POINT ( 'NONE',  ( -198.0356074513804572, -15.37879056873074290, 40.00000000000002132 ) ) ;
#19474 = CARTESIAN_POINT ( 'NONE',  ( -100.7734535825088500, -17.32597176626812185, -40.00000000000002132 ) ) ;
#19475 = EDGE_CURVE ( 'NONE', #22942, #11462, #13334, .T. ) ;
#19476 = CARTESIAN_POINT ( 'NONE',  ( -198.0356074513804572, -10.87444709759729911, 10.87444709759714812 ) ) ;
#19477 = CARTESIAN_POINT ( 'NONE',  ( -105.3755690713226585, 21.75974354311648185, -40.00000000000002132 ) ) ;
#19479 = CARTESIAN_POINT ( 'NONE',  ( -190.0000000000000000, 52.49999999999987210, 82.49999999999998579 ) ) ;
#19478 = CARTESIAN_POINT ( 'NONE',  ( -3.762763306026898569, -43.08566851766588712, -23.50897034858821399 ) ) ;
#19480 = B_SPLINE_CURVE_WITH_KNOTS ( 'NONE', 3,
 ( #20635, #16639, #24899, #14769, #12916, #18634, #24633, #18902, #12647, #6391, #18769, #20772, #24768, #2411 ),
 .UNSPECIFIED., .F., .F.,
 ( 4, 2, 2, 2, 2, 2, 4 ),
 ( 0.0003146819161523679766, 0.002410867973011127964, 0.004507054029869887735, 0.008699426143587403806, 0.01079561220044616271, 0.01289179825730491814, 0.01708417037102243421 ),
 .UNSPECIFIED. ) ;
#19481 = CARTESIAN_POINT ( 'NONE',  ( -213.1075012329537230, 1.045191102001431893E-13, -13.71589010951911902 ) ) ;
#19482 = CARTESIAN_POINT ( 'NONE',  ( 130.8568914410475088, -24.07718906446910623, 32.49135343045471558 ) ) ;
#19483 = CARTESIAN_POINT ( 'NONE',  ( -56.48582580120559271, 30.84685318188643066, 2.449293598294708485E-15 ) ) ;
#19485 = VERTEX_POINT ( 'NONE', #15451 ) ;
#19484 = AXIS2_PLACEMENT_3D ( 'NONE', #6283, #2174, #22663 ) ;
#19486 = EDGE_CURVE ( 'NONE', #22320, #10668, #14973, .T. ) ;
#19487 = CARTESIAN_POINT ( 'NONE',  ( 60.14720761599947707, -33.22245024482351994, 10.94158980378562163 ) ) ;
#19488 = DIRECTION ( 'NONE',  ( -0.01051738777841029586, 0.3995761382614174129, 0.9166396752739929266 ) ) ;
#19489 = CARTESIAN_POINT ( 'NONE',  ( -30.26275506840324070, 1.198031551615912571, 57.76657404653985139 ) ) ;
#19490 = CARTESIAN_POINT ( 'NONE',  ( 163.1118516004056573, 1.251511021549353291E-13, -27.26290988616872824 ) ) ;
#19491 = CARTESIAN_POINT ( 'NONE',  ( -82.30853939107804251, 18.59635467392883612, 7.798227509426476800 ) ) ;
#19492 = CARTESIAN_POINT ( 'NONE',  ( -16.87994666116171061, 20.93785811897321025, -39.19724034061671603 ) ) ;
#19493 = CARTESIAN_POINT ( 'NONE',  ( 200.0000000000000284, 7.828075510571024687, 17.32306842307162142 ) ) ;
#19494 = DIRECTION ( 'NONE',  ( 0.000000000000000000, 0.000000000000000000, 1.000000000000000000 ) ) ;
#19495 = CARTESIAN_POINT ( 'NONE',  ( -82.25988539629348395, -4.395343885513712578, -19.70400758346194436 ) ) ;
#19496 = CARTESIAN_POINT ( 'NONE',  ( -198.0356074513804572, 39.15871834505887250, 17.40982414986519089 ) ) ;
#19497 = CARTESIAN_POINT ( 'NONE',  ( -259.2033419157646676, 6.730120644403918995, -49.83842185052024831 ) ) ;
#19498 = CARTESIAN_POINT ( 'NONE',  ( -110.0995178903039715, 20.14662320684453789, -1.423929044649810516 ) ) ;
#19499 = CARTESIAN_POINT ( 'NONE',  ( 184.8905102610680444, -14.79361573936399665, 14.79361573936367158 ) ) ;
#19500 = CARTESIAN_POINT ( 'NONE',  ( 4.995406935893305977, -39.06748935135157552, -39.06748935135225764 ) ) ;
#19502 = CARTESIAN_POINT ( 'NONE',  ( 192.4448373802101173, -14.14213562375826605, -42.42640687116518450 ) ) ;
#19501 = CARTESIAN_POINT ( 'NONE',  ( -105.3755690713226727, -12.89780903124395550, -12.89780903124416511 ) ) ;
#19503 = CARTESIAN_POINT ( 'NONE',  ( 19.06497207195980792, 66.60410523465830579, -10.03556273973354251 ) ) ;
#19504 = AXIS2_PLACEMENT_3D ( 'NONE', #16699, #10724, #16568 ) ;
#19505 = DIRECTION ( 'NONE',  ( 0.000000000000000000, 1.000000000000000000, 0.000000000000000000 ) ) ;
#19506 = DIRECTION ( 'NONE',  ( -1.836970198721030427E-16, 1.000000000000000000, -1.682156097916904081E-16 ) ) ;
#19507 = CARTESIAN_POINT ( 'NONE',  ( -189.9999999999999716, 82.50000000000008527, 52.49999999999977973 ) ) ;
#19508 = CARTESIAN_POINT ( 'NONE',  ( -280.0000000000000000, 14.14213562373078581, 14.14213562373108424 ) ) ;
#19509 = CARTESIAN_POINT ( 'NONE',  ( -198.0356074513804572, 55.37879056871320671, 40.00000000000002132 ) ) ;
#19510 = ORIENTED_EDGE ( 'NONE', *, *, #14999, .T. ) ;
#19511 = CARTESIAN_POINT ( 'NONE',  ( -91.56559293963834989, 12.25131212657490209, -44.31723036834897300 ) ) ;
#19512 = CARTESIAN_POINT ( 'NONE',  ( -82.28158354860731549, -18.01692715714676041, -9.172261728117373281 ) ) ;
#19513 = CARTESIAN_POINT ( 'NONE',  ( 23.42154907652751561, 13.79745687233752349, 46.79103593565447738 ) ) ;
#19514 = DIRECTION ( 'NONE',  ( 0.000000000000000000, 1.000000000000000000, 0.000000000000000000 ) ) ;
#19515 = VERTEX_POINT ( 'NONE', #25712 ) ;
#19516 = FACE_OUTER_BOUND ( 'NONE', #25396, .T. ) ;
#19517 = CARTESIAN_POINT ( 'NONE',  ( 199.9999999999999716, -5.826418053481885906, -18.09029720167993105 ) ) ;
#19518 = CARTESIAN_POINT ( 'NONE',  ( 37.37129771730447203, -12.75330473319407254, 41.71823991403014276 ) ) ;
#19519 = EDGE_CURVE ( 'NONE', #1180, #7095, #25195, .T. ) ;
#19520 = AXIS2_PLACEMENT_3D ( 'NONE', #951, #9059, #10660 ) ;
#19521 = DIRECTION ( 'NONE',  ( -1.000000000000000000, 0.000000000000000000, 0.000000000000000000 ) ) ;
#19522 = CARTESIAN_POINT ( 'NONE',  ( 199.0053905349878107, 15.66748078252780374, -12.42684713134076979 ) ) ;
#19523 = EDGE_CURVE ( 'NONE', #14253, #17137, #21709, .T. ) ;
#19524 = DIRECTION ( 'NONE',  ( 0.000000000000000000, 0.000000000000000000, 1.000000000000000000 ) ) ;
#19525 = CARTESIAN_POINT ( 'NONE',  ( -213.1075012329537230, 39.99999999999992895, 13.71589010951925935 ) ) ;
#19526 = CARTESIAN_POINT ( 'NONE',  ( -82.30220482034330587, -7.441767004318910139, 18.74474319042423076 ) ) ;
#19527 = CARTESIAN_POINT ( 'NONE',  ( 21.99343714674524364, 47.30053030063396591, -13.87412077874980554 ) ) ;
#19528 = CARTESIAN_POINT ( 'NONE',  ( 151.7948205124836250, -6.767089262349004208, -2.449293598294708485E-15 ) ) ;
#19530 = CARTESIAN_POINT ( 'NONE',  ( -603.3435784881913833, 35.47800896442519303, -18.49335706250612077 ) ) ;
#19529 = CARTESIAN_POINT ( 'NONE',  ( -166.7090905287452358, 15.35183918158013405, -37.06261835976449248 ) ) ;
#19531 = EDGE_CURVE ( 'NONE', #3571, #10760, #25847, .T. ) ;
#19532 = CARTESIAN_POINT ( 'NONE',  ( 170.2234770963711128, 24.55285855007190676, 40.00000000000002132 ) ) ;
#19533 = CARTESIAN_POINT ( 'NONE',  ( 151.7948205124836250, 23.49921654116361225, -23.49921654116333514 ) ) ;
#19534 = CARTESIAN_POINT ( 'NONE',  ( -56.48582580120559982, -9.153146818113595984, 40.00000000000002132 ) ) ;
#19535 = CARTESIAN_POINT ( 'NONE',  ( -135.8532207217289738, 39.99999999999990763, 9.153146818113990335 ) ) ;
#19536 = CARTESIAN_POINT ( 'NONE',  ( 163.1118516004056573, -40.00000000000027711, 27.26290988616830546 ) ) ;
#19537 = CARTESIAN_POINT ( 'NONE',  ( 140.2228883168555456, -30.42137490627649044, -12.60094607221633289 ) ) ;
#19538 = ORIENTED_EDGE ( 'NONE', *, *, #23713, .F. ) ;
#19540 = CARTESIAN_POINT ( 'NONE',  ( -3.417371742523410028, 43.31092608455699633, -17.93997298316182665 ) ) ;
#19539 = CARTESIAN_POINT ( 'NONE',  ( -210.0000000000000284, 66.50000000000001421, -66.50000000000005684 ) ) ;
#19541 = CARTESIAN_POINT ( 'NONE',  ( 136.1360204305621266, -4.966164525587039691, -2.449293598294708485E-15 ) ) ;
#19542 = AXIS2_PLACEMENT_3D ( 'NONE', #19842, #5231, #7339 ) ;
#19543 = CARTESIAN_POINT ( 'NONE',  ( -100.7734535825088358, -16.03295912088728770, 16.03295912088687913 ) ) ;
#19544 = CARTESIAN_POINT ( 'NONE',  ( -200.5022718138935431, 44.86987976039424098, -18.58571273880625441 ) ) ;
#19545 = DIRECTION ( 'NONE',  ( 0.000000000000000000, 0.000000000000000000, -1.000000000000000000 ) ) ;
#19546 = EDGE_LOOP ( 'NONE', ( #23700, #23340, #14156, #1149, #9277, #21043 ) ) ;
#19547 = ORIENTED_EDGE ( 'NONE', *, *, #9481, .T. ) ;
#19548 = DIRECTION ( 'NONE',  ( 0.000000000000000000, 1.000000000000000000, 0.000000000000000000 ) ) ;
#19549 = CARTESIAN_POINT ( 'NONE',  ( 151.0853911467766295, 12.04115959308003525, -29.06993079631216048 ) ) ;
#19550 = CARTESIAN_POINT ( 'NONE',  ( -192.1131137119204766, 43.98782916596428549, -24.17676406461154315 ) ) ;
#19551 = ORIENTED_EDGE ( 'NONE', *, *, #2404, .F. ) ;
#19552 = CARTESIAN_POINT ( 'NONE',  ( 200.0000000000003695, -13.00390091431020956, 13.88089034683036616 ) ) ;
#19553 = FACE_OUTER_BOUND ( 'NONE', #20421, .T. ) ;
#19554 = CARTESIAN_POINT ( 'NONE',  ( -30.26275506840323715, 29.48230279907789253, 29.48230279907799556 ) ) ;
#19555 = DIRECTION ( 'NONE',  ( 0.000000000000000000, -1.000000000000000000, 0.000000000000000000 ) ) ;
#19556 = CARTESIAN_POINT ( 'NONE',  ( 91.82158438592158234, 7.693928927950222250E-14, -17.20528682183300262 ) ) ;
#19557 = CARTESIAN_POINT ( 'NONE',  ( -199.9999999999999716, -49.28189405767602693, 14.17215463606940595 ) ) ;
#19558 = CARTESIAN_POINT ( 'NONE',  ( -200.0000000000000000, -52.49999999999992895, -52.49999999999999289 ) ) ;
#19559 = DIRECTION ( 'NONE',  ( 0.000000000000000000, 1.000000000000000000, 0.000000000000000000 ) ) ;
#19560 = CIRCLE ( 'NONE', #18714, 14.99999999999999645 ) ;
#19561 = CARTESIAN_POINT ( 'NONE',  ( 4.995406935893297984, -39.99999999999986500, -15.24977328854874870 ) ) ;
#19562 = CARTESIAN_POINT ( 'NONE',  ( 170.2234770963711128, 1.955190573858485757E-13, -15.44714144992816074 ) ) ;
#19563 = CARTESIAN_POINT ( 'NONE',  ( -114.7755410848754281, -16.60116338991689489, 14.64251757343854976 ) ) ;
#19564 = CARTESIAN_POINT ( 'NONE',  ( -56.48582580120559982, -21.81201906317755501, -34.75652343174621706 ) ) ;
#19565 = CARTESIAN_POINT ( 'NONE',  ( 184.8905102610680444, 1.070102760522089011E-13, -20.92133201514444352 ) ) ;
#19566 = EDGE_CURVE ( 'NONE', #287, #16217, #3892, .T. ) ;
#19567 = CARTESIAN_POINT ( 'NONE',  ( -30.26275506840324070, -1.198031551616032919, 1.198031551616014712 ) ) ;
#19568 = CARTESIAN_POINT ( 'NONE',  ( 147.2817042152898068, 29.82799917201313633, 12.35516179550145210 ) ) ;
#19569 = CYLINDRICAL_SURFACE ( 'NONE', #3022, 5.000000000000004441 ) ;
#19570 = CARTESIAN_POINT ( 'NONE',  ( 146.6084372240433709, 52.76785682606519146, 3.800685668858932775 ) ) ;
#19571 = CARTESIAN_POINT ( 'NONE',  ( -213.1075012329537230, -40.00000000000011369, 13.71589010951897691 ) ) ;
#19572 = CARTESIAN_POINT ( 'NONE',  ( 14.38125909742181463, 10.73282306405862485, 67.30136555898259587 ) ) ;
#19573 =( BOUNDED_SURFACE ( )  B_SPLINE_SURFACE ( 3, 2, ( 
 ( #13078, #25576, #23563 ),
 ( #8817, #6814, #13320 ),
 ( #5216, #10818, #16928 ),
 ( #2846, #23190, #7322 ),
 ( #19190, #21440, #25062 ),
 ( #25320, #5338, #18931 ),
 ( #21322, #6942, #23066 ),
 ( #19311, #15436, #21193 ),
 ( #25194, #5095, #8952 ),
 ( #17184, #4838, #13447 ) ),
 .UNSPECIFIED., .F., .F., .F. ) 
 B_SPLINE_SURFACE_WITH_KNOTS ( ( 4, 2, 2, 2, 4 ),
 ( 3, 3 ),
 ( 0.04080948307332495084, 0.04814637154418376086, 0.04998059366189846336, 0.05181481577961316587, 0.05548326001504257088 ),
 ( 0.000000000000000000, 1.000000000000000000 ),
 .UNSPECIFIED. ) 
 GEOMETRIC_REPRESENTATION_ITEM ( )  RATIONAL_B_SPLINE_SURFACE ( (
 ( 1.000000000000000000, 0.9547549646669141188, 1.000000000000000000),
 ( 1.000000000000000000, 0.9524144703618939722, 1.000000000000000000),
 ( 1.000000000000000000, 0.9505737003611494096, 1.000000000000000000),
 ( 1.000000000000000000, 0.9490046242078488126, 1.000000000000000000),
 ( 1.000000000000000000, 0.9487292854021939226, 1.000000000000000000),
 ( 1.000000000000000000, 0.9482585386214895662, 1.000000000000000000),
 ( 1.000000000000000000, 0.9480625482234854573, 1.000000000000000000),
 ( 1.000000000000000000, 0.9475921161413758398, 1.000000000000000000),
 ( 1.000000000000000000, 0.9474351228594215524, 1.000000000000000000),
 ( 1.000000000000000000, 0.9474350314971546894, 1.000000000000000000) ) ) 
 REPRESENTATION_ITEM ( '' )  SURFACE ( )  );
#19574 = CARTESIAN_POINT ( 'NONE',  ( -198.0356074513804572, -39.15871834505931304, 17.40982414986437377 ) ) ;
#19575 = CARTESIAN_POINT ( 'NONE',  ( -658.6516411767275940, 42.45902836772346944, -14.91759928563551263 ) ) ;
#19576 = CARTESIAN_POINT ( 'NONE',  ( 22.27781863254865158, 23.58928354748257661, 43.19367102556063287 ) ) ;
#19577 = VERTEX_POINT ( 'NONE', #7853 ) ;
#19578 = CARTESIAN_POINT ( 'NONE',  ( -30.26275506840323715, 29.48230279907829754, -29.48230279907758344 ) ) ;
#19579 = CARTESIAN_POINT ( 'NONE',  ( 180.0000000000000284, -115.7889608577475400, 1.947751065783218452E-14 ) ) ;
#19580 = DIRECTION ( 'NONE',  ( 0.000000000000000000, 0.000000000000000000, 1.000000000000000000 ) ) ;
#19581 = ORIENTED_EDGE ( 'NONE', *, *, #24913, .F. ) ;
#19582 = CIRCLE ( 'NONE', #21712, 5.000000000000004441 ) ;
#19583 = DIRECTION ( 'NONE',  ( 1.000000000000000000, -0.000000000000000000, -0.000000000000000000 ) ) ;
#19584 = CARTESIAN_POINT ( 'NONE',  ( -3.762763306026896792, -23.50897034858817491, 43.08566851766595107 ) ) ;
#19585 = CARTESIAN_POINT ( 'NONE',  ( -62.79433447035942351, 9.335111860984262933, 25.93934121792603875 ) ) ;
#19586 = CIRCLE ( 'NONE', #8562, 5.000000000000004441 ) ;
#19587 = ORIENTED_EDGE ( 'NONE', *, *, #23125, .T. ) ;
#19588 = VERTEX_POINT ( 'NONE', #11722 ) ;
#19589 = AXIS2_PLACEMENT_3D ( 'NONE', #11721, #22607, #17834 ) ;
#19590 = AXIS2_PLACEMENT_3D ( 'NONE', #17556, #21691, #13961 ) ;
#19591 = CARTESIAN_POINT ( 'NONE',  ( -238.4067589809705794, -28.96627169325313389, -27.60227080167074831 ) ) ;
#19592 = CARTESIAN_POINT ( 'NONE',  ( -198.0356074513804572, 39.99999999999992895, 15.37879056873084771 ) ) ;
#19593 = CARTESIAN_POINT ( 'NONE',  ( 48.46159167847756066, 11.89574563387566464, -37.63079830025095163 ) ) ;
#19594 = CARTESIAN_POINT ( 'NONE',  ( -86.96347745069644475, 12.89780903124419353, -12.89780903124389333 ) ) ;
#19595 = CARTESIAN_POINT ( 'NONE',  ( -208.1127848780265026, -2.327190355601776466E-13, 55.00245453012672670 ) ) ;
#19596 = CARTESIAN_POINT ( 'NONE',  ( 199.9999999999998863, -18.99932777274695539, 0.6272729670678898195 ) ) ;
#19597 = AXIS2_PLACEMENT_3D ( 'NONE', #3725, #20089, #9971 ) ;
#19598 = CARTESIAN_POINT ( 'NONE',  ( 91.82158438592156813, 39.99999999999995737, 22.79471317813484887 ) ) ;
#19599 = FACE_OUTER_BOUND ( 'NONE', #8134, .T. ) ;
#19600 = VECTOR ( 'NONE', #9580, 1000.000000000000000 ) ;
#19601 = CARTESIAN_POINT ( 'NONE',  ( -5.304449574936379364, -17.72890873421744473, -42.80137191221640336 ) ) ;
#19602 = CARTESIAN_POINT ( 'NONE',  ( -280.0000000000000568, 42.42640687119294540, -14.14213562373059041 ) ) ;
#19603 = CARTESIAN_POINT ( 'NONE',  ( -105.2334157265396044, -21.31091308246848115, 2.725992507772964757 ) ) ;
#19604 = CARTESIAN_POINT ( 'NONE',  ( 130.8568914410475088, -39.99999999999992895, -5.949712681207114606 ) ) ;
#19605 = DIRECTION ( 'NONE',  ( 0.000000000000000000, -0.6739498806388346530, -0.7387770694782699321 ) ) ;
#19606 = CARTESIAN_POINT ( 'NONE',  ( 57.59792236341147031, 2.435789363418170872, 40.00000000000002132 ) ) ;
#19607 = CARTESIAN_POINT ( 'NONE',  ( -280.0000000000000568, -20.00000000000006395, -40.00000000000002132 ) ) ;
#19608 = CARTESIAN_POINT ( 'NONE',  ( -86.96347745069645896, 43.67073346367970288, 12.89780903124427702 ) ) ;
#19609 = CARTESIAN_POINT ( 'NONE',  ( 57.59792236341147031, 2.435789363418170872, -40.00000000000002132 ) ) ;
#19611 = DIRECTION ( 'NONE',  ( -0.3301743753983408247, 0.000000000000000000, -0.9439199552029374773 ) ) ;
#19610 = CARTESIAN_POINT ( 'NONE',  ( -3.901164313503183934, -43.04571088859058392, -23.47934491069905505 ) ) ;
#19612 = CARTESIAN_POINT ( 'NONE',  ( -86.96347745069644475, -2.438961472018186339E-13, 21.75974354311649961 ) ) ;
#19613 = CARTESIAN_POINT ( 'NONE',  ( 170.2234770963711128, 10.92277846919201068, 10.92277846919202133 ) ) ;
#19614 = CARTESIAN_POINT ( 'NONE',  ( 130.8568914410475088, 5.949712681206719367, -40.00000000000002132 ) ) ;
#19615 = ORIENTED_EDGE ( 'NONE', *, *, #16052, .T. ) ;
#19616 = CARTESIAN_POINT ( 'NONE',  ( 59.93546481438061591, -31.86477106141256499, 13.19882033579247960 ) ) ;
#19617 = VECTOR ( 'NONE', #26189, 1000.000000000000000 ) ;
#19618 = LINE ( 'NONE', #13621, #8549 ) ;
#19619 =( BOUNDED_SURFACE ( )  B_SPLINE_SURFACE ( 3, 2, ( 
 ( #11876, #22408, #22273 ),
 ( #4184, #10288, #19859 ),
 ( #1645, #17854, #26005 ),
 ( #5761, #13869, #19996 ),
 ( #1782, #9886, #26135 ),
 ( #7878, #5897, #22135 ),
 ( #22801, #16798, #6421 ),
 ( #4578, #173, #20938 ),
 ( #14407, #24935, #22537 ),
 ( #6684, #22669, #4441 ),
 ( #12535, #12675, #20669 ),
 ( #2716, #8689, #10550 ),
 ( #2304, #18934, #312 ),
 ( #14799, #16536, #24664 ),
 ( #6817, #8414, #4841 ),
 ( #14539, #8279, #25066 ),
 ( #22931, #12408, #18396 ),
 ( #20805, #582, #2438 ),
 ( #8820, #18662, #448 ),
 ( #10821, #12947, #16405 ),
 ( #14933, #21063, #10690 ),
 ( #2576, #10413, #2849 ),
 ( #18802, #8552, #16668 ),
 ( #24533, #24799, #4711 ),
 ( #6551, #14661, #12815 ),
 ( #716, #16931, #23070 ),
 ( #6289, #4318, #20533 ),
 ( #18531, #13323, #7452 ),
 ( #17318, #13203, #9332 ),
 ( #17064, #19440, #15196 ),
 ( #21698, #9081, #19314 ),
 ( #23691, #8955, #15063 ),
 ( #13572, #3218, #17441 ),
 ( #23322, #9207, #25323 ) ),
 .UNSPECIFIED., .F., .F., .F. ) 
 B_SPLINE_SURFACE_WITH_KNOTS ( ( 4, 2, 2, 2, 2, 2, 2, 2, 2, 2, 2, 2, 2, 2, 2, 2, 4 ),
 ( 3, 3 ),
 ( 0.005135432767688113270, 0.02907015807668449081, 0.05300488338568087182, 0.07693960869467725283, 0.08292329002192634635, 0.08441921035373861626, 0.08446595786410775186, 0.08448933161929231273, 0.08451270537447688747, 0.08460620039521515867, 0.08479319043669168721, 0.08516717051964475815, 0.08591513068555090005, 0.08890697134917543987, 0.09189881201279997969, 0.09489065267642453338, 0.1008743340036736269 ),
 ( 0.000000000000000000, 1.000000000000000000 ),
 .UNSPECIFIED. ) 
 GEOMETRIC_REPRESENTATION_ITEM ( )  RATIONAL_B_SPLINE_SURFACE ( (
 ( 1.000000000000000000, 0.9997813423552078804, 1.000000000000000000),
 ( 1.000000000000000000, 0.9991063898506408192, 1.000000000000000000),
 ( 1.000000000000000000, 0.9968824705949637099, 1.000000000000000000),
 ( 1.000000000000000000, 0.9891556793369806755, 1.000000000000000000),
 ( 1.000000000000000000, 0.9836552277522174759, 1.000000000000000000),
 ( 1.000000000000000000, 0.9690805015303916026, 1.000000000000000000),
 ( 1.000000000000000000, 0.9600094330334334458, 1.000000000000000000),
 ( 1.000000000000000000, 0.9461485276689314272, 1.000000000000000000),
 ( 1.000000000000000000, 0.9432497373318702305, 1.000000000000000000),
 ( 1.000000000000000000, 0.9394620364517939359, 1.000000000000000000),
 ( 1.000000000000000000, 0.9386962831138077057, 1.000000000000000000),
 ( 1.000000000000000000, 0.9378980481303066385, 1.000000000000000000),
 ( 1.000000000000000000, 0.9378738510928930072, 1.000000000000000000),
 ( 1.000000000000000000, 0.9378375433852924603, 1.000000000000000000),
 ( 1.000000000000000000, 0.9378253334781214701, 1.000000000000000000),
 ( 1.000000000000000000, 0.9378014123365938648, 1.000000000000000000),
 ( 1.000000000000000000, 0.9377894572438921772, 1.000000000000000000),
 ( 1.000000000000000000, 0.9377297092068129780, 1.000000000000000000),
 ( 1.000000000000000000, 0.9376819985415359993, 1.000000000000000000),
 ( 1.000000000000000000, 0.9375391312191762028, 1.000000000000000000),
 ( 1.000000000000000000, 0.9374442392361908016, 1.000000000000000000),
 ( 1.000000000000000000, 0.9371606329892256948, 1.000000000000000000),
 ( 1.000000000000000000, 0.9369729884417120624, 1.000000000000000000),
 ( 1.000000000000000000, 0.9364144211479323854, 1.000000000000000000),
 ( 1.000000000000000000, 0.9360478649890134895, 1.000000000000000000),
 ( 1.000000000000000000, 0.9342453465010656100, 1.000000000000000000),
 ( 1.000000000000000000, 0.9329002455189610021, 1.000000000000000000),
 ( 1.000000000000000000, 0.9304321598239908564, 1.000000000000000000),
 ( 1.000000000000000000, 0.9293115443287026656, 1.000000000000000000),
 ( 1.000000000000000000, 0.9273348408776519447, 1.000000000000000000),
 ( 1.000000000000000000, 0.9264755133098839801, 1.000000000000000000),
 ( 1.000000000000000000, 0.9243017816397209874, 1.000000000000000000),
 ( 1.000000000000000000, 0.9233922826851888033, 1.000000000000000000),
 ( 1.000000000000000000, 0.9230541040371973427, 1.000000000000000000) ) ) 
 REPRESENTATION_ITEM ( '' )  SURFACE ( )  );
#19620 = CARTESIAN_POINT ( 'NONE',  ( -198.0356074513804572, 39.15871834505901461, 39.15871834505919935 ) ) ;
#19621 = CARTESIAN_POINT ( 'NONE',  ( -100.7734535825088500, -39.99999999999995737, -22.67402823373205578 ) ) ;
#19622 = CARTESIAN_POINT ( 'NONE',  ( 130.8568914410475372, -24.07718906447255947, 24.07718906447199458 ) ) ;
#19623 = CARTESIAN_POINT ( 'NONE',  ( 4.995406935893289102, 55.24977328856464709, -40.00000000000002132 ) ) ;
#19624 = DIRECTION ( 'NONE',  ( -1.000000000000000000, 0.000000000000000000, 0.000000000000000000 ) ) ;
#19625 = CARTESIAN_POINT ( 'NONE',  ( 199.9999999999998863, -7.850736592177782747, 17.31604939001003274 ) ) ;
#19626 = CARTESIAN_POINT ( 'NONE',  ( -86.95438060917183520, 6.705903726404473630, -20.33578048843545361 ) ) ;
#19627 = CARTESIAN_POINT ( 'NONE',  ( 130.8568914410475372, -24.07718906447255947, 24.07718906447199458 ) ) ;
#19628 = CARTESIAN_POINT ( 'NONE',  ( -135.8532207217289738, 6.472252184284583265, -50.09629031063960980 ) ) ;
#19629 = EDGE_CURVE ( 'NONE', #854, #20872, #5875, .T. ) ;
#19630 = CARTESIAN_POINT ( 'NONE',  ( -110.1018896729135577, 20.19745059498566064, -0.1210535641494778075 ) ) ;
#19631 = CARTESIAN_POINT ( 'NONE',  ( 170.2234770963711128, -17.36149277827010096, 17.36149277826970660 ) ) ;
#19632 = CARTESIAN_POINT ( 'NONE',  ( 184.8905102610680444, 43.07788698682591644, -13.49065550809769221 ) ) ;
#19633 = CIRCLE ( 'NONE', #84, 5.000000000000004441 ) ;
#19635 = CARTESIAN_POINT ( 'NONE',  ( -56.48582580120559982, -6.472252184283581400, -50.09629031063973059 ) ) ;
#19634 = CARTESIAN_POINT ( 'NONE',  ( -208.1127848780264742, -10.60833733270725787, -67.17687982763172272 ) ) ;
#19636 = CARTESIAN_POINT ( 'NONE',  ( -162.0762913951021176, -27.08623940707584055, -29.48230308784799547 ) ) ;
#19637 = CARTESIAN_POINT ( 'NONE',  ( 19.06497207195980792, 14.19242893257840876, 0.000000000000000000 ) ) ;
#19638 = FACE_BOUND ( 'NONE', #21082, .T. ) ;
#19639 = CARTESIAN_POINT ( 'NONE',  ( -198.0356074513804572, -40.00000000000025580, 55.37879056871310013 ) ) ;
#19640 = CARTESIAN_POINT ( 'NONE',  ( -208.1127848780265026, 10.60833733269551615, -10.60833733269529766 ) ) ;
#19641 = CARTESIAN_POINT ( 'NONE',  ( -208.1127848780265026, 55.00245453012668406, 2.449293598294708485E-15 ) ) ;
#19642 = VERTEX_POINT ( 'NONE', #13982 ) ;
#19643 = CARTESIAN_POINT ( 'NONE',  ( -192.9588430854690273, 66.79921049721887982, 10.23066800229522677 ) ) ;
#19644 = CARTESIAN_POINT ( 'NONE',  ( -26.85274238233094479, 36.33581074325618232, 15.05078560967874424 ) ) ;
#19645 = CARTESIAN_POINT ( 'NONE',  ( 44.82887508595239723, 12.17256213114513130, 38.96139886165431676 ) ) ;
#19646 = CARTESIAN_POINT ( 'NONE',  ( -87.10560006382461040, -21.31071338413648064, 2.727320883041552957 ) ) ;
#19647 = VERTEX_POINT ( 'NONE', #6013 ) ;
#19648 = CARTESIAN_POINT ( 'NONE',  ( -188.3392535381819926, -43.01687576774265409, 23.45796413246070244 ) ) ;
#19649 = CARTESIAN_POINT ( 'NONE',  ( 200.0000000000000568, -11.58056098922197563, -15.07187815445410806 ) ) ;
#19650 = CARTESIAN_POINT ( 'NONE',  ( 23.72853009152353820, -23.26754081577996658, 42.74808902029987223 ) ) ;
#19651 = CARTESIAN_POINT ( 'NONE',  ( 85.88462004898991609, 22.72792989851439316, -10.32535764751219176 ) ) ;
#19652 = CARTESIAN_POINT ( 'NONE',  ( 199.0056040927672711, 16.99126215759308778, -10.54120702991739122 ) ) ;
#19653 = CARTESIAN_POINT ( 'NONE',  ( -87.12771530791273733, 21.45464684660704791, 1.404361561684027704 ) ) ;
#19654 = CARTESIAN_POINT ( 'NONE',  ( -259.2033419157646676, -1.438356298054549103E-14, -9.517827891722632216 ) ) ;
#19655 = CARTESIAN_POINT ( 'NONE',  ( -208.1127848780265026, -9.061048840815752106E-14, 15.00245453012669472 ) ) ;
#19656 = DIRECTION ( 'NONE',  ( 1.000000000000000000, 1.836970198721030427E-16, -0.000000000000000000 ) ) ;
#19657 = CARTESIAN_POINT ( 'NONE',  ( 57.59792236341147031, 2.435789363418170872, 40.00000000000002132 ) ) ;
#19659 = DIRECTION ( 'NONE',  ( 0.000000000000000000, -1.000000000000000000, 0.000000000000000000 ) ) ;
#19658 = CARTESIAN_POINT ( 'NONE',  ( -166.3490736462251220, 19.13702016909153514, -36.43932733833390358 ) ) ;
#19660 = CARTESIAN_POINT ( 'NONE',  ( -135.8532207217289454, -30.84685318188649106, 40.00000000000002132 ) ) ;
#19661 = CARTESIAN_POINT ( 'NONE',  ( 170.2234770963711128, 24.55285855007190321, 0.000000000000000000 ) ) ;
#19662 = CARTESIAN_POINT ( 'NONE',  ( -91.56559293963834989, -22.67402823373193499, 40.00000000000002132 ) ) ;
#19663 = CARTESIAN_POINT ( 'NONE',  ( -56.48582580120560692, 39.99999999999991473, 9.153146818114004546 ) ) ;
#19664 = CARTESIAN_POINT ( 'NONE',  ( -162.0762913951020892, -1.202636532414034422E-14, -1.694272876828323948 ) ) ;
#19665 = CARTESIAN_POINT ( 'NONE',  ( -105.3755690713226727, 15.38646221621771737, 15.38646221621800514 ) ) ;
#19666 = ORIENTED_EDGE ( 'NONE', *, *, #3474, .F. ) ;
#19668 = CARTESIAN_POINT ( 'NONE',  ( 3.774039766332595747, 44.61221010187614411, -18.47898247163319851 ) ) ;
#19667 = CARTESIAN_POINT ( 'NONE',  ( -362.0709805440841365, -4.857225732735059864E-14, 10.00000000000004796 ) ) ;
#19669 = CARTESIAN_POINT ( 'NONE',  ( -30.26275506840324070, 1.198031551616013601, 1.198031551616023371 ) ) ;
#19670 = CARTESIAN_POINT ( 'NONE',  ( -97.73860346100528318, -8.185503821043738526, 20.89580782305262829 ) ) ;
#19671 = ORIENTED_EDGE ( 'NONE', *, *, #348, .F. ) ;
#19672 = EDGE_LOOP ( 'NONE', ( #3581, #4332 ) ) ;
#19673 = CARTESIAN_POINT ( 'NONE',  ( -94.58366989427237570, 9.000605044545558542, -20.58370269626824367 ) ) ;
#19674 = CARTESIAN_POINT ( 'NONE',  ( 156.1979191798867532, 11.34289806466608219, -27.38417834433175102 ) ) ;
#19675 = ORIENTED_EDGE ( 'NONE', *, *, #4120, .F. ) ;
#19676 = CARTESIAN_POINT ( 'NONE',  ( -105.4741150117398831, -19.77569912955107156, 7.943527260749587704 ) ) ;
#19677 = EDGE_LOOP ( 'NONE', ( #26079, #9404, #5968, #14155, #699, #16074 ) ) ;
#19678 = CARTESIAN_POINT ( 'NONE',  ( 199.9999999999999432, -11.20938440123365432, 15.35472082164171326 ) ) ;
#19679 = CARTESIAN_POINT ( 'NONE',  ( 169.9999999999999716, 21.59613885783086928, 12.70659020859114818 ) ) ;
#19680 = CARTESIAN_POINT ( 'NONE',  ( 0.2972598230769907257, 66.70487387989857098, 10.13633138497486641 ) ) ;
#19681 = CARTESIAN_POINT ( 'NONE',  ( -109.1264249741457775, -13.72187187121248719, 33.12752917270314867 ) ) ;
#19682 = CARTESIAN_POINT ( 'NONE',  ( 199.9999999999999432, 1.065690307512836407E-13, -20.00000000000010303 ) ) ;
#19683 = CARTESIAN_POINT ( 'NONE',  ( -199.9999999999999716, -44.96258949770061264, 22.85346793133696153 ) ) ;
#19684 = DIRECTION ( 'NONE',  ( -1.303213150798907793E-16, 1.000000000000000000, -1.682156097916904081E-16 ) ) ;
#19685 = FACE_OUTER_BOUND ( 'NONE', #20752, .T. ) ;
#19686 = CARTESIAN_POINT ( 'NONE',  ( 14.38125909742181108, 1.616281842095393922E-13, -15.17850393972633682 ) ) ;
#19687 = B_SPLINE_CURVE_WITH_KNOTS ( 'NONE', 3,
 ( #18035, #8197, #22450, #4358, #2350, #24030, #12056, #215, #20176, #8459, #22316, #5808, #12192, #26187, #14316, #10463 ),
 .UNSPECIFIED., .F., .F.,
 ( 4, 2, 2, 2, 2, 2, 2, 4 ),
 ( -5.998499567488215554E-08, 0.003520343011582076007, 0.007040746008159827485, 0.01408155200131532524, 0.01760195499789306978, 0.02112235799447082299, 0.02464276099104856926, 0.02816316398762631901 ),
 .UNSPECIFIED. ) ;
#19688 = CARTESIAN_POINT ( 'NONE',  ( -198.0356074513804572, -39.99999999999990052, -15.37879056873112482 ) ) ;
#19689 = CARTESIAN_POINT ( 'NONE',  ( -110.0791661673102766, -10.82529631553216554, 17.04053483149554182 ) ) ;
#19690 = CARTESIAN_POINT ( 'NONE',  ( -135.8532207217289738, 6.472252184284186249, -6.472252184284142729 ) ) ;
#19691 = CARTESIAN_POINT ( 'NONE',  ( -200.0000000000000568, 17.27712336974197882, -46.88040655664261891 ) ) ;
#19692 = CARTESIAN_POINT ( 'NONE',  ( 151.7948205124836534, -33.06932595376343897, -23.49921654116042902 ) ) ;
#19693 = CARTESIAN_POINT ( 'NONE',  ( -103.9474983245025044, 8.027156558344222148, 20.15710290851511033 ) ) ;
#19694 = CIRCLE ( 'NONE', #6970, 28.79780246617542616 ) ;
#19695 = DIRECTION ( 'NONE',  ( -0.000000000000000000, -1.000000000000000000, -0.000000000000000000 ) ) ;
#19696 = CARTESIAN_POINT ( 'NONE',  ( -135.8532207217289738, 6.472252184284186249, -6.472252184284142729 ) ) ;
#19697 = CARTESIAN_POINT ( 'NONE',  ( -30.26275506840324070, -1.147469862568086380E-14, 1.694272468446259783 ) ) ;
#19698 = CARTESIAN_POINT ( 'NONE',  ( -198.0356074513804572, 10.87444709758468875, 67.44298959250869530 ) ) ;
#19699 = CARTESIAN_POINT ( 'NONE',  ( 151.7948205124836250, -4.785054706301600902, -4.785054706301715477 ) ) ;
#19700 = CARTESIAN_POINT ( 'NONE',  ( -173.7925586249088212, -20.60916590992073338, -38.69493321930081464 ) ) ;
#19701 = CARTESIAN_POINT ( 'NONE',  ( 12.01676469546555204, 24.84032989753427501, 44.88780742856546624 ) ) ;
#19702 = ORIENTED_EDGE ( 'NONE', *, *, #7195, .F. ) ;
#19703 = CARTESIAN_POINT ( 'NONE',  ( -100.7734535825088358, 12.25131212657497848, -12.25131212657469604 ) ) ;
#19704 = B_SPLINE_CURVE_WITH_KNOTS ( 'NONE', 3,
 ( #22341, #10622, #8484, #24464, #16601, #14343, #6490, #12473 ),
 .UNSPECIFIED., .F., .F.,
 ( 4, 2, 2, 4 ),
 ( -5.298247996846965421E-05, 0.001923793760055677064, 0.003900570000079824073, 0.007854122480128121128 ),
 .UNSPECIFIED. ) ;
#19705 = CARTESIAN_POINT ( 'NONE',  ( 169.9999999999999716, -9.369682556672181306, -22.62041470344887273 ) ) ;
#19706 = EDGE_CURVE ( 'NONE', #7498, #24112, #16179, .T. ) ;
#19707 = CARTESIAN_POINT ( 'NONE',  ( -617.5592893540214163, 29.80849998618563745, 33.71207106400992615 ) ) ;
#19708 = CARTESIAN_POINT ( 'NONE',  ( -82.23726319250467043, 0.6309363043577198571, 20.19517362731287946 ) ) ;
#19709 = ORIENTED_EDGE ( 'NONE', *, *, #22794, .T. ) ;
#19710 = CARTESIAN_POINT ( 'NONE',  ( 136.1360204305621266, -3.419521671106983309E-13, 35.03383547441296741 ) ) ;
#19711 = CARTESIAN_POINT ( 'NONE',  ( 199.0263771353515949, -14.14574067859894413, 14.14574067859863682 ) ) ;
#19712 = ADVANCED_FACE ( 'NONE', ( #11992 ), #7881, .T. ) ;
#19713 = DIRECTION ( 'NONE',  ( 1.000000000000000000, -0.000000000000000000, -0.000000000000000000 ) ) ;
#19714 = VERTEX_POINT ( 'NONE', #14578 ) ;
#19715 = ORIENTED_EDGE ( 'NONE', *, *, #1929, .F. ) ;
#19716 = CARTESIAN_POINT ( 'NONE',  ( 184.8905102610680444, 19.07866798485562398, -40.00000000000002132 ) ) ;
#19717 = CARTESIAN_POINT ( 'NONE',  ( -197.4153392275576664, -44.73189834454027647, -24.72549520222428754 ) ) ;
#19718 = CARTESIAN_POINT ( 'NONE',  ( -259.2033419157646676, 40.00000000000000711, -9.517827891722491884 ) ) ;
#19719 = EDGE_CURVE ( 'NONE', #22425, #8430, #25566, .T. ) ;
#19720 = EDGE_CURVE ( 'NONE', #10307, #2553, #1761, .T. ) ;
#19721 = FILL_AREA_STYLE_COLOUR ( '', #25309 ) ;
#19722 = DIRECTION ( 'NONE',  ( -1.000000000000000000, -1.836970198721030181E-16, -0.000000000000000000 ) ) ;
#19723 = CARTESIAN_POINT ( 'NONE',  ( 73.43467957758505804, 12.96803903966637961, -26.88835007753401385 ) ) ;
#19724 = CARTESIAN_POINT ( 'NONE',  ( 91.82158438592158234, -6.516925787240506436E-14, 22.79471317813470321 ) ) ;
#19725 = CARTESIAN_POINT ( 'NONE',  ( 199.9999999999998295, -11.08011877867584261, -15.44095579151349185 ) ) ;
#19726 =( BOUNDED_CURVE ( )  B_SPLINE_CURVE ( 3, ( #3655, #5392, #20151, #16016, #5517, #11761, #15871 ),
 .UNSPECIFIED., .F., .F. ) 
 B_SPLINE_CURVE_WITH_KNOTS ( ( 4, 3, 4 ),
 ( 0.007504621739143852409, 0.02318610956072935173, 0.03886759738231801431 ),
 .UNSPECIFIED. ) 
 CURVE ( )  GEOMETRIC_REPRESENTATION_ITEM ( )  RATIONAL_B_SPLINE_CURVE ( ( 0.5852718452494395374, 0.6660804010233950523, 0.8043231192735819102, 1.000000000000000000, 0.8043231192735423862, 0.6660804010233392081, 0.5852718452493905765 ) ) 
 REPRESENTATION_ITEM ( '' )  );
#19727 = CARTESIAN_POINT ( 'NONE',  ( 184.8905102610680444, 40.00000000000013500, -20.92133201514430141 ) ) ;
#19728 = CARTESIAN_POINT ( 'NONE',  ( -200.0000000000000000, -52.49999999999992895, -52.49999999999999289 ) ) ;
#19729 = CARTESIAN_POINT ( 'NONE',  ( -5.866564133087009303, -23.09290806364241533, -42.46617576965061858 ) ) ;
#19730 = CARTESIAN_POINT ( 'NONE',  ( 4.995406935893287326, 17.50105314357225694, -39.06748935135176026 ) ) ;
#19731 = CARTESIAN_POINT ( 'NONE',  ( -77.70130000790287284, -21.34877220993438485, 5.505113979786321110 ) ) ;
#19732 = CARTESIAN_POINT ( 'NONE',  ( -30.26275506840324070, 1.218738420030236455E-14, -1.694272468446259783 ) ) ;
#19733 = CARTESIAN_POINT ( 'NONE',  ( 190.0000000000000000, -52.49999999999992895, -52.49999999999999289 ) ) ;
#19734 = CARTESIAN_POINT ( 'NONE',  ( 19.06497207195981503, -14.19242893257840166, 0.000000000000000000 ) ) ;
#19735 = CARTESIAN_POINT ( 'NONE',  ( 14.38125909742181285, -15.17850393972633505, -40.00000000000002132 ) ) ;
#19736 = CARTESIAN_POINT ( 'NONE',  ( 184.8905102610680444, 14.79361573936366092, 41.77492675556006674 ) ) ;
#19737 = CARTESIAN_POINT ( 'NONE',  ( -208.1127848780264742, -55.00245453014425578, -40.00000000000002132 ) ) ;
#19738 = CARTESIAN_POINT ( 'NONE',  ( -110.0524710260411325, 18.17485046464500442, 8.855238217227519470 ) ) ;
#19739 = CARTESIAN_POINT ( 'NONE',  ( -114.7756370326901134, 22.09321776683328764, -1.238720794240111500 ) ) ;
#19740 = CARTESIAN_POINT ( 'NONE',  ( -198.0356074513804572, 39.15871834505901461, 39.15871834505919935 ) ) ;
#19741 = CARTESIAN_POINT ( 'NONE',  ( 130.8568914410475088, 5.949712681206712261, 40.00000000000002132 ) ) ;
#19742 = ORIENTED_EDGE ( 'NONE', *, *, #3862, .F. ) ;
#19743 = CARTESIAN_POINT ( 'NONE',  ( 23.64688638900328144, -46.70960658758826867, 13.78084749393243769 ) ) ;
#19744 = CARTESIAN_POINT ( 'NONE',  ( 121.8740240556054317, 11.10671848392250638, 26.81399039734629497 ) ) ;
#19745 = CARTESIAN_POINT ( 'NONE',  ( -56.48582580120559982, 21.81201906317778594, -34.75652343174606074 ) ) ;
#19746 = CARTESIAN_POINT ( 'NONE',  ( -86.96347745069643054, -40.00000000000009948, 18.24025645688337960 ) ) ;
#19747 = CARTESIAN_POINT ( 'NONE',  ( 200.0000000000000000, 14.14213562373041455, 42.42640687119311593 ) ) ;
#19748 = B_SPLINE_CURVE_WITH_KNOTS ( 'NONE', 3,
 ( #11027, #13025, #19137, #23898, #7531, #26051, #1563, #13653 ),
 .UNSPECIFIED., .F., .F.,
 ( 4, 2, 2, 4 ),
 ( -5.298247996938804799E-05, 0.001923793760048753132, 0.003900570000066894312, 0.007854122480103177539 ),
 .UNSPECIFIED. ) ;
#19749 = CARTESIAN_POINT ( 'NONE',  ( 91.82158438592158234, -17.20528682183298486, -40.00000000000002132 ) ) ;
#19750 = CARTESIAN_POINT ( 'NONE',  ( -678.9461782662789346, 90.00000000000000000, -29.99999999999836220 ) ) ;
#19751 = CARTESIAN_POINT ( 'NONE',  ( 199.9999999999996021, 1.536416165433052594, 18.94899354046687279 ) ) ;
#19752 = CARTESIAN_POINT ( 'NONE',  ( -82.24857225180258524, 3.161095685030960833, -19.95174621266928128 ) ) ;
#19753 = CARTESIAN_POINT ( 'NONE',  ( 130.8568914410475088, 4.207082182989012153, 52.36146031193425188 ) ) ;
#19754 = CARTESIAN_POINT ( 'NONE',  ( -105.3755690713226727, -12.89780903124395550, -12.89780903124416511 ) ) ;
#19755 = AXIS2_PLACEMENT_3D ( 'NONE', #21303, #13681, #13550 ) ;
#19756 = CARTESIAN_POINT ( 'NONE',  ( -114.5543403404773528, 20.90252105098865698, -6.785539716556657552 ) ) ;
#19757 = CARTESIAN_POINT ( 'NONE',  ( -30.26275506840324070, 1.218738420030236455E-14, -1.694272468446259783 ) ) ;
#19758 = CARTESIAN_POINT ( 'NONE',  ( -100.7734535825088500, 16.03295912088740494, -40.53558337403661938 ) ) ;
#19760 = CARTESIAN_POINT ( 'NONE',  ( -198.0356074513804572, -17.40982414986427429, -39.15871834505933435 ) ) ;
#19759 = CARTESIAN_POINT ( 'NONE',  ( -213.1075012329536946, -37.98287015391210275, -37.98287015391272092 ) ) ;
#19761 = CARTESIAN_POINT ( 'NONE',  ( 170.2234770963711128, -45.64576402573167258, -10.92277846919254891 ) ) ;
#19762 = CARTESIAN_POINT ( 'NONE',  ( 146.6084372240433993, 34.62501878078308692, 0.000000000000000000 ) ) ;
#19764 = CARTESIAN_POINT ( 'NONE',  ( 14.38125909742182529, -40.00000000000021316, 55.17850393974251944 ) ) ;
#19763 = CARTESIAN_POINT ( 'NONE',  ( -30.26275506840324070, 1.198031551616030033, -1.198031551616006496 ) ) ;
#19765 = CARTESIAN_POINT ( 'NONE',  ( 14.38125909742181996, -10.73282306403606157, 67.30136555895948902 ) ) ;
#19766 = PRESENTATION_LAYER_ASSIGNMENT (  '', '', ( #16380 ) ) ;
#19767 = CARTESIAN_POINT ( 'NONE',  ( 163.1118516004056573, 19.27778845538753316, 19.27778845538783870 ) ) ;
#19768 = VECTOR ( 'NONE', #6850, 1000.000000000000000 ) ;
#19769 = CARTESIAN_POINT ( 'NONE',  ( 91.82158438592158234, 22.79471317813471742, 40.00000000000002132 ) ) ;
#19770 = EDGE_LOOP ( 'NONE', ( #6010, #19551, #1213, #12483 ) ) ;
#19771 = CARTESIAN_POINT ( 'NONE',  ( -259.2033419157646676, -6.730120644403570829, -6.730120644403545960 ) ) ;
#19772 = CARTESIAN_POINT ( 'NONE',  ( 84.01322141327635507, 23.61859044091702131, 9.783140484763423572 ) ) ;
#19773 = CARTESIAN_POINT ( 'NONE',  ( 23.49666234703665424, 23.31470603676248032, 42.81942870555097613 ) ) ;
#19774 = CARTESIAN_POINT ( 'NONE',  ( -86.96347745069644475, -21.75974354311652093, 40.00000000000002132 ) ) ;
#19775 = CIRCLE ( 'NONE', #21912, 5.000000000000095035 ) ;
#19776 = ORIENTED_EDGE ( 'NONE', *, *, #12467, .T. ) ;
#19777 = CARTESIAN_POINT ( 'NONE',  ( -188.3065677117183441, -43.00727648871537667, 23.45084385698005391 ) ) ;
#19778 = CIRCLE ( 'NONE', #4937, 5.000000000000007994 ) ;
#19779 = CARTESIAN_POINT ( 'NONE',  ( 199.9999999999998863, -17.44218472118251384, 7.566354988273278792 ) ) ;
#19780 = EDGE_CURVE ( 'NONE', #18643, #15543, #11103, .T. ) ;
#19781 = CARTESIAN_POINT ( 'NONE',  ( 11.71430589699291502, -24.82930166510167069, 44.87285427231071111 ) ) ;
#19782 = CARTESIAN_POINT ( 'NONE',  ( 22.89002945277437817, 17.87003923493782764, -43.14209108112063973 ) ) ;
#19783 = CARTESIAN_POINT ( 'NONE',  ( 199.0065087001378572, 6.107362818253672998, -19.04251412529381327 ) ) ;
#19784 = CIRCLE ( 'NONE', #24482, 15.00000000000000000 ) ;
#19785 = CARTESIAN_POINT ( 'NONE',  ( -86.86493150571114086, -19.60045294882784717, -8.366608963953355627 ) ) ;
#19786 = CARTESIAN_POINT ( 'NONE',  ( 130.8568914410475088, 40.00000000000015632, -34.05028731879774284 ) ) ;
#19787 = FACE_BOUND ( 'NONE', #5079, .T. ) ;
#19788 = DIRECTION ( 'NONE',  ( 0.000000000000000000, 0.000000000000000000, -1.000000000000000000 ) ) ;
#19789 = CARTESIAN_POINT ( 'NONE',  ( -213.1075012329537230, -53.71589010950170717, 40.00000000000002132 ) ) ;
#19790 = CARTESIAN_POINT ( 'NONE',  ( -129.2303573020045633, 11.67678754050021617, -24.84170325986431038 ) ) ;
#19791 = LINE ( 'NONE', #17922, #3366 ) ;
#19793 = CARTESIAN_POINT ( 'NONE',  ( -56.48582580120559271, 9.153146818113576444, -0.000000000000000000 ) ) ;
#19792 = AXIS2_PLACEMENT_3D ( 'NONE', #11284, #21923, #9811 ) ;
#19794 = CARTESIAN_POINT ( 'NONE',  ( 4.995406935893288214, 15.24977328854832770, 40.00000000000002132 ) ) ;
#19795 = CARTESIAN_POINT ( 'NONE',  ( 130.8568914410475088, -39.99999999999992895, -5.949712681207114606 ) ) ;
#19796 = CARTESIAN_POINT ( 'NONE',  ( -86.96347745069644475, -2.438961472018186339E-13, 21.75974354311649961 ) ) ;
#19797 = CARTESIAN_POINT ( 'NONE',  ( -91.56559293963836410, 16.03295912088692177, 16.03295912088721664 ) ) ;
#19798 = ADVANCED_FACE ( 'NONE', ( #24573 ), #15049, .T. ) ;
#19799 = ORIENTED_EDGE ( 'NONE', *, *, #20058, .T. ) ;
#19800 = DIRECTION ( 'NONE',  ( 0.000000000000000000, 0.000000000000000000, 1.000000000000000000 ) ) ;
#19801 = CARTESIAN_POINT ( 'NONE',  ( 14.38125909742181285, -15.17850393972633505, 0.000000000000000000 ) ) ;
#19802 = CARTESIAN_POINT ( 'NONE',  ( 199.0263771353515949, -14.14574067859894413, 14.14574067859863682 ) ) ;
#19803 = CARTESIAN_POINT ( 'NONE',  ( -94.58414068594231594, -8.590713000773435581, 20.73981583680210150 ) ) ;
#19804 = CONTEXT_DEPENDENT_SHAPE_REPRESENTATION ( #24823, #12081 ) ;
#19805 = VERTEX_POINT ( 'NONE', #22945 ) ;
#19806 = EDGE_LOOP ( 'NONE', ( #17577, #21518 ) ) ;
#19807 = VECTOR ( 'NONE', #6015, 1000.000000000000000 ) ;
#19808 = CARTESIAN_POINT ( 'NONE',  ( -86.86493150571111244, 8.366608963953098055, -19.60045294882791467 ) ) ;
#19809 = CARTESIAN_POINT ( 'NONE',  ( 23.32574057153203029, -46.82643129194535447, -13.80366151303456235 ) ) ;
#19810 = ORIENTED_EDGE ( 'NONE', *, *, #49, .F. ) ;
#19811 = CARTESIAN_POINT ( 'NONE',  ( 136.1360204305621551, 4.966164525587093870, -40.00000000000002132 ) ) ;
#19812 = VERTEX_POINT ( 'NONE', #23083 ) ;
#19813 = CARTESIAN_POINT ( 'NONE',  ( 200.0000000000000000, 2.625635831523228880, 18.82681798050185051 ) ) ;
#19814 = CYLINDRICAL_SURFACE ( 'NONE', #1364, 5.000000000000004441 ) ;
#19815 = CARTESIAN_POINT ( 'NONE',  ( 163.1118516004056573, -19.27778845539233998, 37.29075403953149959 ) ) ;
#19816 = CARTESIAN_POINT ( 'NONE',  ( -296.0000000000000000, -4.857225732735059864E-14, 0.000000000000000000 ) ) ;
#19817 = AXIS2_PLACEMENT_3D ( 'NONE', #21730, #1134, #15088 ) ;
#19818 = VECTOR ( 'NONE', #5862, 1000.000000000000000 ) ;
#19819 = CARTESIAN_POINT ( 'NONE',  ( 130.8568914410475372, 1.429239637432775288E-13, -34.05028731879788495 ) ) ;
#19820 = CARTESIAN_POINT ( 'NONE',  ( 192.4448373802101173, 42.42640687116487896, 14.14213562375934075 ) ) ;
#19821 = CARTESIAN_POINT ( 'NONE',  ( -99.21568817060988010, -2.557234656049328691E-13, 22.67402823373191723 ) ) ;
#19822 = CARTESIAN_POINT ( 'NONE',  ( -215.0000000000000284, 60.27431767988564104, -73.32453023895048716 ) ) ;
#19823 = CARTESIAN_POINT ( 'NONE',  ( -105.2054292635175585, -15.19799821370250825, 15.19799821370211923 ) ) ;
#19824 = CARTESIAN_POINT ( 'NONE',  ( -162.0762913951021176, -40.00000000000003553, -1.694272876828743168 ) ) ;
#19825 = CARTESIAN_POINT ( 'NONE',  ( -105.2958943009710708, -11.44501736922669366, 18.12177707673897586 ) ) ;
#19826 = CARTESIAN_POINT ( 'NONE',  ( -105.3755690713226585, -12.89780903124383471, -43.67073346367985920 ) ) ;
#19827 = CARTESIAN_POINT ( 'NONE',  ( 163.1118516004056573, 27.26290988616876021, -40.00000000000002132 ) ) ;
#19828 = CARTESIAN_POINT ( 'NONE',  ( -213.1075012329536946, -37.98287015391263566, 37.98287015391218802 ) ) ;
#19829 = DIRECTION ( 'NONE',  ( 0.000000000000000000, 0.3995982397413447851, -0.9166903767333977049 ) ) ;
#19830 = CARTESIAN_POINT ( 'NONE',  ( -575.0231298121445889, 75.00000000000000000, 24.99999999999828759 ) ) ;
#19831 = CARTESIAN_POINT ( 'NONE',  ( 199.9999999999999432, -1.727494763561684666E-13, 20.00000000000010303 ) ) ;
#19832 = CARTESIAN_POINT ( 'NONE',  ( 14.38125909742181108, -5.035366881890652543E-14, 15.17850393972633682 ) ) ;
#19833 = CARTESIAN_POINT ( 'NONE',  ( 57.59792236341147031, -30.00663442387700641, 26.56190807104681895 ) ) ;
#19834 = CARTESIAN_POINT ( 'NONE',  ( 146.6084372240433993, 24.48358557860307272, 24.48358557860347418 ) ) ;
#19835 = CARTESIAN_POINT ( 'NONE',  ( -194.4222169614567974, -24.44978956119031466, -44.35789444896748535 ) ) ;
#19836 = CARTESIAN_POINT ( 'NONE',  ( -56.48582580120559982, -21.81201906317755501, -34.75652343174621706 ) ) ;
#19837 = ORIENTED_EDGE ( 'NONE', *, *, #24600, .T. ) ;
#19838 = CARTESIAN_POINT ( 'NONE',  ( -56.48582580120559271, 21.81201906317798489, -21.81201906317746619 ) ) ;
#19839 = FACE_OUTER_BOUND ( 'NONE', #5201, .T. ) ;
#19840 = CARTESIAN_POINT ( 'NONE',  ( 0.2972598230769983307, -14.33493731733933352, 0.000000000000000000 ) ) ;
#19841 = CIRCLE ( 'NONE', #9170, 5.000000000000007994 ) ;
#19842 = CARTESIAN_POINT ( 'NONE',  ( -200.0000000000000000, 6.162975822039154730E-30, 0.000000000000000000 ) ) ;
#19843 = CARTESIAN_POINT ( 'NONE',  ( -56.48582580120559982, -34.75652343174584047, -21.81201906317815187 ) ) ;
#19844 = FACE_OUTER_BOUND ( 'NONE', #14977, .T. ) ;
#19845 = ORIENTED_EDGE ( 'NONE', *, *, #25121, .T. ) ;
#19846 = CARTESIAN_POINT ( 'NONE',  ( -280.0000000000000000, -2.609240458947769655E-13, 20.00000000000001421 ) ) ;
#19847 = CARTESIAN_POINT ( 'NONE',  ( 199.0164104981701030, -14.74880145479427007, -13.53568457017083659 ) ) ;
#19848 = CARTESIAN_POINT ( 'NONE',  ( -3.615356597031627039, 17.91804473398352471, 43.25798660799035389 ) ) ;
#19849 = EDGE_LOOP ( 'NONE', ( #1113, #18609, #24473, #21304 ) ) ;
#19850 = VERTEX_POINT ( 'NONE', #8702 ) ;
#19851 = CARTESIAN_POINT ( 'NONE',  ( -198.0356074513804572, 55.37879056874818673, -40.00000000000002132 ) ) ;
#19852 = CARTESIAN_POINT ( 'NONE',  ( 146.6084372240433993, 24.48358557860341733, -24.48358557860313311 ) ) ;
#19853 = CARTESIAN_POINT ( 'NONE',  ( 14.38125909742180930, 39.99999999999982947, 55.17850393971022527 ) ) ;
#19854 = CARTESIAN_POINT ( 'NONE',  ( -89.91498783735231370, -20.17141720490575452, -8.733585467941317404 ) ) ;
#19855 = EDGE_CURVE ( 'NONE', #567, #1760, #6017, .T. ) ;
#19856 = CARTESIAN_POINT ( 'NONE',  ( 19.06497207195981147, 38.31983398719673772, -38.31983398719579981 ) ) ;
#19857 = CARTESIAN_POINT ( 'NONE',  ( 4.995406935893290878, 1.606505379428369110E-13, -15.24977328854832592 ) ) ;
#19858 = CARTESIAN_POINT ( 'NONE',  ( 200.0000000000002558, -14.49689853580991539, 12.29876589910006857 ) ) ;
#19859 = CARTESIAN_POINT ( 'NONE',  ( -121.8281105897340382, 10.16551987017660252, 22.46071553381061037 ) ) ;
#19860 = CARTESIAN_POINT ( 'NONE',  ( -4.201409602818432454, -13.81669219312479058, -46.93439176590607786 ) ) ;
#19861 = EDGE_CURVE ( 'NONE', #18917, #19457, #25988, .T. ) ;
#19862 = CARTESIAN_POINT ( 'NONE',  ( -105.3755690713226585, 15.38646221621820764, -41.18208027870583265 ) ) ;
#19863 = CARTESIAN_POINT ( 'NONE',  ( -77.55640685876514340, -22.13135000837104371, 0.6996548653676145646 ) ) ;
#19864 = CARTESIAN_POINT ( 'NONE',  ( 192.4448373802101173, -42.42640687116490028, -14.14213562375904942 ) ) ;
#19865 = CARTESIAN_POINT ( 'NONE',  ( 184.8905102610680444, -40.00000000000021316, 20.92133201514402430 ) ) ;
#19866 = DIRECTION ( 'NONE',  ( 0.000000000000000000, 0.000000000000000000, 1.000000000000000000 ) ) ;
#19867 = CARTESIAN_POINT ( 'NONE',  ( 146.6084372240433993, 34.62501878078308692, 0.000000000000000000 ) ) ;
#19868 =( REPRESENTATION_RELATIONSHIP ('NONE','NONE', #23888, #21040 ) REPRESENTATION_RELATIONSHIP_WITH_TRANSFORMATION ( #12219 )SHAPE_REPRESENTATION_RELATIONSHIP( ) );
#19869 = CARTESIAN_POINT ( 'NONE',  ( -208.1127848780264742, -15.00245453012673202, 40.00000000000002132 ) ) ;
#19870 = EDGE_CURVE ( 'NONE', #8765, #13305, #16207, .T. ) ;
#19871 = EDGE_CURVE ( 'NONE', #162, #19333, #6358, .T. ) ;
#19872 = CARTESIAN_POINT ( 'NONE',  ( -135.8532207217289738, 34.75652343174594705, 21.81201906317792449 ) ) ;
#19873 = CARTESIAN_POINT ( 'NONE',  ( -91.56559293963834989, -17.32597176626812896, -2.449293598294708485E-15 ) ) ;
#19874 = CARTESIAN_POINT ( 'NONE',  ( 21.98945382326337139, -43.25809532770868060, -23.63684424402663709 ) ) ;
#19875 = CARTESIAN_POINT ( 'NONE',  ( -114.4098922876147384, 20.15198150140922451, 8.347224046571190215 ) ) ;
#19876 = CARTESIAN_POINT ( 'NONE',  ( -259.2033419157646676, 49.83842185052027673, -6.730120644403441155 ) ) ;
#19877 = CARTESIAN_POINT ( 'NONE',  ( -198.0356074513804572, 55.37879056874818673, -40.00000000000002132 ) ) ;
#19878 = ORIENTED_EDGE ( 'NONE', *, *, #19169, .T. ) ;
#19879 = CARTESIAN_POINT ( 'NONE',  ( -77.92915424793434909, 20.15198149301296482, 8.347224043097730473 ) ) ;
#19880 = CARTESIAN_POINT ( 'NONE',  ( -280.0000000000000000, -5.143516556418885058E-14, -6.902532920683853297E-30 ) ) ;
#19881 = B_SPLINE_CURVE_WITH_KNOTS ( 'NONE', 3,
 ( #7735, #11736, #15989, #21724, #1380, #3499 ),
 .UNSPECIFIED., .F., .F.,
 ( 4, 2, 4 ),
 ( 0.0003134494097674369825, 0.004478637758889606260, 0.008643826108011775158 ),
 .UNSPECIFIED. ) ;
#19882 = CARTESIAN_POINT ( 'NONE',  ( -56.48582580120559982, 50.09629031063966664, -6.472252184284094767 ) ) ;
#19883 = CARTESIAN_POINT ( 'NONE',  ( 192.4448373802101173, -39.99999999999991473, -20.00000000003956302 ) ) ;
#19884 = CARTESIAN_POINT ( 'NONE',  ( -100.7734535825088358, -16.03295912088728770, 16.03295912088687913 ) ) ;
#19885 = DIRECTION ( 'NONE',  ( 0.000000000000000000, 1.000000000000000000, 0.000000000000000000 ) ) ;
#19886 = CARTESIAN_POINT ( 'NONE',  ( 170.2234770963711128, 15.44714144992819627, -40.00000000000002132 ) ) ;
#19887 = EDGE_CURVE ( 'NONE', #7420, #9502, #18303, .T. ) ;
#19888 = DIRECTION ( 'NONE',  ( -1.836970198721030427E-16, 1.000000000000000000, -1.682156097916904327E-16 ) ) ;
#19889 = CARTESIAN_POINT ( 'NONE',  ( 199.9999999999996305, 13.20330696038688068, 13.67115712520468840 ) ) ;
#19890 = CARTESIAN_POINT ( 'NONE',  ( 199.9999999999998863, -14.89105141260043119, -11.81423002201253603 ) ) ;
#19891 = CARTESIAN_POINT ( 'NONE',  ( -280.0000000000000568, 42.42640687119265408, 14.14213562373147504 ) ) ;
#19892 = CARTESIAN_POINT ( 'NONE',  ( 14.38125909742180752, 17.55144818341503665, -39.01709431150898411 ) ) ;
#19893 = CARTESIAN_POINT ( 'NONE',  ( -265.6482238768269326, 0.000000000000000000, 0.000000000000000000 ) ) ;
#19894 = CARTESIAN_POINT ( 'NONE',  ( -280.0000000000000000, -2.609240458947769655E-13, 20.00000000000001421 ) ) ;
#19895 = CARTESIAN_POINT ( 'NONE',  ( -280.0000000000000000, -14.14213562373088706, -14.14213562373108424 ) ) ;
#19897 = CARTESIAN_POINT ( 'NONE',  ( -56.48582580120559271, -6.472252184284276844, 6.472252184284108978 ) ) ;
#19896 = CARTESIAN_POINT ( 'NONE',  ( 0.2972598230769923355, 18.14793986248751168, -38.42060263243650553 ) ) ;
#19898 = CARTESIAN_POINT ( 'NONE',  ( 14.38125909742181463, 10.73282306403652875, -67.30136555895941797 ) ) ;
#19899 = EDGE_CURVE ( 'NONE', #14022, #4265, #3900, .T. ) ;
#19900 = CARTESIAN_POINT ( 'NONE',  ( -4.039451493210490796, 46.99046209229823745, -13.82811171175438147 ) ) ;
#19901 = FACE_BOUND ( 'NONE', #11270, .T. ) ;
#19902 = CIRCLE ( 'NONE', #8494, 20.00000000000001421 ) ;
#19904 = CARTESIAN_POINT ( 'NONE',  ( 199.9999999999999432, 1.065690307512836407E-13, -20.00000000000010303 ) ) ;
#19903 = CARTESIAN_POINT ( 'NONE',  ( 130.8568914410475088, 4.207082182989012153, 52.36146031193425188 ) ) ;
#19905 = CARTESIAN_POINT ( 'NONE',  ( 130.8568914410475088, 24.07718906446891793, 32.49135343045489321 ) ) ;
#19906 = CARTESIAN_POINT ( 'NONE',  ( 146.6084372240433993, -24.48358557860353457, 24.48358557860296258 ) ) ;
#19907 = CARTESIAN_POINT ( 'NONE',  ( 163.1118516004056573, -27.26290988616869626, 40.00000000000002132 ) ) ;
#19908 = VERTEX_POINT ( 'NONE', #13989 ) ;
#19909 = CARTESIAN_POINT ( 'NONE',  ( 14.38125909742180397, 67.30136555895953165, 10.73282306403583242 ) ) ;
#19910 = LINE ( 'NONE', #16044, #18434 ) ;
#19911 = CARTESIAN_POINT ( 'NONE',  ( 27.55177309533993579, 13.49150912997473029, 45.29548561695333575 ) ) ;
#19912 = CARTESIAN_POINT ( 'NONE',  ( -91.56559293963834989, -22.67402823373193499, 40.00000000000002132 ) ) ;
#19913 = EDGE_LOOP ( 'NONE', ( #19389, #22910, #24778, #15209 ) ) ;
#19914 = CARTESIAN_POINT ( 'NONE',  ( -188.4265004370476504, -43.04236487214783580, 23.47686928852971278 ) ) ;
#19915 = CARTESIAN_POINT ( 'NONE',  ( 199.9999999999997442, -19.00693066143141152, -0.3125757794583984839 ) ) ;
#19916 = CARTESIAN_POINT ( 'NONE',  ( -4.022465846214261731, -13.82902411340761617, 46.99661175925233891 ) ) ;
#19917 = AXIS2_PLACEMENT_3D ( 'NONE', #6423, #22933, #13206 ) ;
#19918 = CARTESIAN_POINT ( 'NONE',  ( 23.72853009152652248, 23.26754081577798061, -42.74808902029882773 ) ) ;
#19919 = CARTESIAN_POINT ( 'NONE',  ( 199.0073291892102247, 3.255542347464756681, -19.72957075196997323 ) ) ;
#19920 = CARTESIAN_POINT ( 'NONE',  ( -210.0000000000000284, 66.50000000000009948, -66.50000000000005684 ) ) ;
#19921 = CARTESIAN_POINT ( 'NONE',  ( 192.4448373802100889, 1.051811698935164031E-13, -20.00000000003942091 ) ) ;
#19922 = CARTESIAN_POINT ( 'NONE',  ( -100.7734535825088500, -16.03295912088659492, -40.53558337403696044 ) ) ;
#19923 = CARTESIAN_POINT ( 'NONE',  ( -198.0356074513804572, -55.37879056874826489, 40.00000000000002132 ) ) ;
#19925 = CARTESIAN_POINT ( 'NONE',  ( -596.9804635992022668, 40.00314282705044633, -1.996769250129288187 ) ) ;
#19924 = CARTESIAN_POINT ( 'NONE',  ( -173.7925586250955803, 20.60916590995285702, -38.69493321937137154 ) ) ;
#19926 = CARTESIAN_POINT ( 'NONE',  ( -56.48582580120559271, 9.153146818113576444, -0.000000000000000000 ) ) ;
#19927 = CARTESIAN_POINT ( 'NONE',  ( 200.0000000000000000, 20.00000000000013856, -40.00000000000002132 ) ) ;
#19928 = CARTESIAN_POINT ( 'NONE',  ( -135.8532207217289738, -9.153146818113595984, 0.000000000000000000 ) ) ;
#19929 = CARTESIAN_POINT ( 'NONE',  ( 170.2234770963711128, -39.99999999999982947, -15.44714144992858529 ) ) ;
#19930 = CARTESIAN_POINT ( 'NONE',  ( 57.59792236341147031, -1.493297263419786540E-14, 2.435789363418160658 ) ) ;
#19931 = CARTESIAN_POINT ( 'NONE',  ( 199.9999999999999432, 14.14213562373093680, 14.14213562373114641 ) ) ;
#19932 = EDGE_LOOP ( 'NONE', ( #20087, #7815, #20821, #3551 ) ) ;
#19933 = CARTESIAN_POINT ( 'NONE',  ( -65.65550967573776120, 24.04430752631801482, -11.16467289560278786 ) ) ;
#19934 = CARTESIAN_POINT ( 'NONE',  ( 199.9999999999999432, 20.00000000000013856, 0.000000000000000000 ) ) ;
#19935 = CARTESIAN_POINT ( 'NONE',  ( -99.31364972222458221, -8.164808577129251788, 20.79869444140758361 ) ) ;
#19936 = VERTEX_POINT ( 'NONE', #17841 ) ;
#19937 = VERTEX_POINT ( 'NONE', #22121 ) ;
#19938 = CARTESIAN_POINT ( 'NONE',  ( -162.0762913951020892, -57.76657433524000851, 1.198031840315820329 ) ) ;
#19939 = CARTESIAN_POINT ( 'NONE',  ( 25.88393124179782134, -42.08451360835658761, -22.82896322160914693 ) ) ;
#19940 = VERTEX_POINT ( 'NONE', #18111 ) ;
#19941 = CARTESIAN_POINT ( 'NONE',  ( -86.96347745069644475, 18.24025645688350750, -40.00000000000002132 ) ) ;
#19942 = CARTESIAN_POINT ( 'NONE',  ( -96.94449363885364335, -20.74048850981448666, 8.590991630952846236 ) ) ;
#19943 = AXIS2_PLACEMENT_3D ( 'NONE', #553, #20907, #10387 ) ;
#19944 = EDGE_LOOP ( 'NONE', ( #1083, #17900, #3485, #20285, #16604, #3608, #5975, #15214, #13551, #6016 ) ) ;
#19945 = CARTESIAN_POINT ( 'NONE',  ( 200.0000000000001705, 18.83917254958691601, 2.502331228272203223 ) ) ;
#19946 = LINE ( 'NONE', #1730, #7697 ) ;
#19947 = CARTESIAN_POINT ( 'NONE',  ( -192.9588430854689989, 38.51493924976929861, 38.51493924976947625 ) ) ;
#19948 = CARTESIAN_POINT ( 'NONE',  ( -188.6890294954709759, -47.12920239600229166, -13.84869711777369616 ) ) ;
#19949 = CARTESIAN_POINT ( 'NONE',  ( 14.38125909742182529, -40.00000000000021316, 55.17850393974251944 ) ) ;
#19950 = CARTESIAN_POINT ( 'NONE',  ( -162.0762913951021176, 41.69427287672986182, 40.00000000000002132 ) ) ;
#19951 = CARTESIAN_POINT ( 'NONE',  ( 163.1118516004056573, 9.006482792069759213, -9.006482792069505194 ) ) ;
#19952 = DIRECTION ( 'NONE',  ( 1.000000000000000000, 0.000000000000000000, 0.000000000000000000 ) ) ;
#19953 = EDGE_CURVE ( 'NONE', #16073, #7987, #160, .T. ) ;
#19954 = CARTESIAN_POINT ( 'NONE',  ( -259.2033419157646676, -40.00000000000003553, -9.517827891722768996 ) ) ;
#19955 = VECTOR ( 'NONE', #11599, 1000.000000000000000 ) ;
#19956 = CARTESIAN_POINT ( 'NONE',  ( 184.8905102610680444, -39.99999999999978684, -19.07866798485600768 ) ) ;
#19957 = CARTESIAN_POINT ( 'NONE',  ( -199.9999999999999147, -49.28189405767606956, -14.17215463606684267 ) ) ;
#19958 = CARTESIAN_POINT ( 'NONE',  ( -238.4067589809705794, -0.6820004458488042598, 57.25054294077229855 ) ) ;
#19959 = CARTESIAN_POINT ( 'NONE',  ( 184.8905102610680444, 20.92133201514447549, 0.000000000000000000 ) ) ;
#19960 = EDGE_CURVE ( 'NONE', #87, #1721, #12132, .T. ) ;
#19961 = CARTESIAN_POINT ( 'NONE',  ( 19.06497207195982924, -66.60410523465823474, 10.03556273973400081 ) ) ;
#19962 = FACE_BOUND ( 'NONE', #11304, .T. ) ;
#19963 = CIRCLE ( 'NONE', #5952, 5.000000000000004441 ) ;
#19964 = EDGE_CURVE ( 'NONE', #23087, #1338, #22581, .T. ) ;
#19965 = FACE_OUTER_BOUND ( 'NONE', #25469, .T. ) ;
#19966 = CARTESIAN_POINT ( 'NONE',  ( -30.26275506840324070, 1.218738420030236455E-14, -1.694272468446259783 ) ) ;
#19967 = CARTESIAN_POINT ( 'NONE',  ( 4.995406935893297984, -40.00000000000007816, 15.24977328854818914 ) ) ;
#19968 = CARTESIAN_POINT ( 'NONE',  ( -213.1075012329537230, 37.98287015391236565, -18.58567234101138510 ) ) ;
#19969 = CARTESIAN_POINT ( 'NONE',  ( -114.6128314109029134, 10.93000550580449470, 19.07544683981866029 ) ) ;
#19970 = CARTESIAN_POINT ( 'NONE',  ( -188.8384220655410957, -17.93083973458429270, -43.28887647197308297 ) ) ;
#19971 = CARTESIAN_POINT ( 'NONE',  ( 146.6084372240433993, 24.48358557860341733, -24.48358557860313311 ) ) ;
#19972 = ORIENTED_EDGE ( 'NONE', *, *, #16296, .T. ) ;
#19973 = CARTESIAN_POINT ( 'NONE',  ( -213.1075012329537230, -18.58567234101102272, -37.98287015391260013 ) ) ;
#19974 = CARTESIAN_POINT ( 'NONE',  ( -114.7827960788993380, 0.6714470530296268169, 22.13220202243102719 ) ) ;
#19975 = CARTESIAN_POINT ( 'NONE',  ( -91.56559293963836410, 22.67402823373189946, -0.000000000000000000 ) ) ;
#19976 = CARTESIAN_POINT ( 'NONE',  ( 160.9163046357249129, -135.7889608577475542, 49.61140153332247138 ) ) ;
#19977 = CARTESIAN_POINT ( 'NONE',  ( 151.7948205124836250, 4.785054706301759886, -4.785054706301612448 ) ) ;
#19978 = CARTESIAN_POINT ( 'NONE',  ( -82.24289765308560618, 2.209159509541283040, 20.07413437147899771 ) ) ;
#19979 = ORIENTED_EDGE ( 'NONE', *, *, #10379, .T. ) ;
#19980 = CARTESIAN_POINT ( 'NONE',  ( 199.9999999999999432, 10.02849973080021684, 16.14841691778726940 ) ) ;
#19981 = CARTESIAN_POINT ( 'NONE',  ( -105.2054292635175585, -15.19799821370250825, 15.19799821370211923 ) ) ;
#19982 = CARTESIAN_POINT ( 'NONE',  ( -3.977426076245963671, 17.87762021094844656, 43.16039317622611549 ) ) ;
#19983 = ORIENTED_EDGE ( 'NONE', *, *, #14445, .T. ) ;
#19984 = EDGE_LOOP ( 'NONE', ( #14213, #7695, #10468, #2253, #18642 ) ) ;
#19985 = CARTESIAN_POINT ( 'NONE',  ( 0.2972598230769938343, 10.13633138497472252, 10.13633138497475628 ) ) ;
#19986 = CARTESIAN_POINT ( 'NONE',  ( 199.0058097323984327, 9.278912463403225175, -17.71230630396810213 ) ) ;
#19987 = LINE ( 'NONE', #14262, #23832 ) ;
#19988 = CARTESIAN_POINT ( 'NONE',  ( -96.94475454971986039, -20.58449551006464162, -9.001119816733867296 ) ) ;
#19989 = CIRCLE ( 'NONE', #464, 9.999999999999996447 ) ;
#19990 = CARTESIAN_POINT ( 'NONE',  ( -626.9846540392142060, 90.00000000000000000, 34.99999999999999289 ) ) ;
#19991 = CARTESIAN_POINT ( 'NONE',  ( 130.8568914410475372, -3.326198072800416995E-13, 34.05028731879788495 ) ) ;
#19992 = LINE ( 'NONE', #4043, #24469 ) ;
#19993 = CARTESIAN_POINT ( 'NONE',  ( -77.55640685891414421, -22.13135000830937926, -1.385220247072852517 ) ) ;
#19994 = DIRECTION ( 'NONE',  ( 0.000000000000000000, 1.000000000000000000, 0.000000000000000000 ) ) ;
#19995 = CARTESIAN_POINT ( 'NONE',  ( 199.0193391886810446, 8.833261569310058903, 17.94623560139499574 ) ) ;
#19996 = CARTESIAN_POINT ( 'NONE',  ( -144.0562564040095879, 14.68019406005356586, 29.54282788278102956 ) ) ;
#19997 = CARTESIAN_POINT ( 'NONE',  ( 1.925538622596224103, -24.44644315488275055, -44.35335385591496049 ) ) ;
#19998 = CARTESIAN_POINT ( 'NONE',  ( -91.56559293963834989, -40.53558337403692491, 16.03295912088671571 ) ) ;
#19999 = CARTESIAN_POINT ( 'NONE',  ( -87.13361725327074225, -16.16366093424068495, 14.23233549117614416 ) ) ;
#20000 = CARTESIAN_POINT ( 'NONE',  ( 146.6084372240433709, -3.800685668858344801, -52.76785682606520567 ) ) ;
#20001 = CARTESIAN_POINT ( 'NONE',  ( -30.26275506840324070, -40.00000000000001421, -1.694272468446678559 ) ) ;
#20002 = CARTESIAN_POINT ( 'NONE',  ( -259.2033419157646676, -6.730120644403663199, 6.730120644403451813 ) ) ;
#20003 = CARTESIAN_POINT ( 'NONE',  ( -280.0000000000000568, 42.42640687119294540, -14.14213562373059041 ) ) ;
#20004 = CARTESIAN_POINT ( 'NONE',  ( -91.56559293963834989, -17.32597176626812896, 40.00000000000002132 ) ) ;
#20005 = CARTESIAN_POINT ( 'NONE',  ( -238.4067589809705794, 0.6820004457912851592, -0.6820004457913123597 ) ) ;
#20006 = AXIS2_PLACEMENT_3D ( 'NONE', #13707, #25972, #7328 ) ;
#20007 = CARTESIAN_POINT ( 'NONE',  ( 130.8568914410475372, -5.949712681206667853, -2.449293598294708485E-15 ) ) ;
#20008 = CARTESIAN_POINT ( 'NONE',  ( -114.6863919488549470, 12.18775077807936569, 18.37411471036764965 ) ) ;
#20009 = CARTESIAN_POINT ( 'NONE',  ( 184.8905102610680444, 39.99999999999983658, 20.92133201514485563 ) ) ;
#20010 = CARTESIAN_POINT ( 'NONE',  ( -198.0356074513804572, 10.87444709759714989, 10.87444709759722450 ) ) ;
#20011 = CARTESIAN_POINT ( 'NONE',  ( -86.96347745069644475, -21.75974354311652093, -40.00000000000002132 ) ) ;
#20012 = VERTEX_POINT ( 'NONE', #26120 ) ;
#20013 = EDGE_CURVE ( 'NONE', #22947, #1902, #26144, .T. ) ;
#20014 =( BOUNDED_SURFACE ( )  B_SPLINE_SURFACE ( 3, 3, ( 
 ( #21852, #5621, #7223, #23975, #15714, #1637, #23586, #5751, #21346, #13727, #23711, #11222, #5491, #1124, #13591, #11464, #9478, #3624, #3116, #3240, #11734, #21722, #5238, #19852, #19459, #17846, #17584, #25996, #19335, #9229 ),
 ( #3497, #15339, #19591, #11596, #23467, #13343, #1247, #9351, #17461, #5365, #13470, #21591, #1378, #15857, #24537, #5765, #12152, #13874, #13737, #24400, #21863, #3639, #1917, #20000, #20275, #12283, #16004, #10022, #23986, #24130 ),
 ( #6040, #22277, #24266, #3777, #7745, #2053, #10293, #18132, #8158, #26009, #6166, #9890, #16271, #8020, #22413, #10160, #11746, #26281, #5902, #4189, #26139, #18263, #14010, #45, #14276, #20410, #2184, #17858, #19864, #18400 ),
 ( #177, #4051, #14145, #8283, #16409, #1649, #22139, #9758, #22007, #3920, #12019, #11880, #1786, #17993, #7883, #20139, #16136, #452, #14802, #20672, #18665, #10960, #8555, #849, #22934, #20941, #6293, #8824, #10693, #14666 ),
 ( #18937, #21066, #4445, #10553, #6554, #4714, #12818, #2852, #16671, #6424, #10824, #12678, #14542, #585, #20808, #22804, #24802, #4581, #23073, #8692, #24940, #22672, #2719, #12411, #19067, #2579, #16538, #16801, #8958, #719 ),
 ( #18805, #6688, #16934, #22541, #12538, #25069, #2441, #17067, #6820, #14937, #4844, #14411, #2308, #12950, #4321, #20537, #10416, #18534, #316, #8417, #24668, #13326, #2973, #19570, #13454, #7206, #1361, #25582, #25704, #5102 ),
 ( #11447, #13574, #9460, #21201, #11576, #5345, #5474, #19318, #19696, #25201, #21573, #3221, #15066, #11327, #4977, #17444, #15321, #21447, #17567, #1484, #25326, #3347, #19443, #9084, #7455, #7085, #15570, #1231, #23694, #21701 ) ),
 .UNSPECIFIED., .T., .F., .T. ) 
 B_SPLINE_SURFACE_WITH_KNOTS ( ( 4, 3, 4 ),
 ( 4, 2, 2, 2, 2, 2, 2, 2, 2, 2, 2, 2, 2, 2, 4 ),
 ( 0.000000000000000000, 0.5000000000000000000, 1.000000000000000000 ),
 ( 0.000000000000000000, 0.1357259735107005372, 0.1651108541090157700, 0.1944957347073310028, 0.3598804999793158710, 0.3867117631979620773, 0.4135430264166082281, 0.5789277916885930964, 0.6062785021374117456, 0.6336292125862302838, 0.8508620842112317728, 0.8814014469398914198, 0.9119408096685510667, 0.9559704048342755334, 1.000000000000000000 ),
 .UNSPECIFIED. ) 
 GEOMETRIC_REPRESENTATION_ITEM ( )  RATIONAL_B_SPLINE_SURFACE ( (
 ( 1.000000000000000000, 1.000000000000000000, 1.000000000000000000, 1.000000000000000000, 1.000000000000000000, 1.000000000000000000, 1.000000000000000000, 1.000000000000000000, 1.000000000000000000, 1.000000000000000000, 1.000000000000000000, 1.000000000000000000, 1.000000000000000000, 1.000000000000000000, 1.000000000000000000, 1.000000000000000000, 1.000000000000000000, 1.000000000000000000, 1.000000000000000000, 1.000000000000000000, 1.000000000000000000, 1.000000000000000000, 1.000000000000000000, 1.000000000000000000, 1.000000000000000000, 1.000000000000000000, 1.000000000000000000, 1.000000000000000000, 1.000000000000000000, 1.000000000000000000),
 ( 0.3333333333333333703, 0.3333333333333333703, 0.3333333333333333703, 0.3333333333333333703, 0.3333333333333333703, 0.3333333333333333703, 0.3333333333333333703, 0.3333333333333333703, 0.3333333333333333703, 0.3333333333333333703, 0.3333333333333333703, 0.3333333333333333703, 0.3333333333333333703, 0.3333333333333333703, 0.3333333333333333703, 0.3333333333333333703, 0.3333333333333333703, 0.3333333333333333703, 0.3333333333333333703, 0.3333333333333333703, 0.3333333333333333703, 0.3333333333333333703, 0.3333333333333333703, 0.3333333333333333703, 0.3333333333333333703, 0.3333333333333333703, 0.3333333333333333703, 0.3333333333333333703, 0.3333333333333333703, 0.3333333333333333703),
 ( 0.3333333333333333703, 0.3333333333333333703, 0.3333333333333333703, 0.3333333333333333703, 0.3333333333333333703, 0.3333333333333333703, 0.3333333333333333703, 0.3333333333333333703, 0.3333333333333333703, 0.3333333333333333703, 0.3333333333333333703, 0.3333333333333333703, 0.3333333333333333703, 0.3333333333333333703, 0.3333333333333333703, 0.3333333333333333703, 0.3333333333333333703, 0.3333333333333333703, 0.3333333333333333703, 0.3333333333333333703, 0.3333333333333333703, 0.3333333333333333703, 0.3333333333333333703, 0.3333333333333333703, 0.3333333333333333703, 0.3333333333333333703, 0.3333333333333333703, 0.3333333333333333703, 0.3333333333333333703, 0.3333333333333333703),
 ( 1.000000000000000000, 1.000000000000000000, 1.000000000000000000, 1.000000000000000000, 1.000000000000000000, 1.000000000000000000, 1.000000000000000000, 1.000000000000000000, 1.000000000000000000, 1.000000000000000000, 1.000000000000000000, 1.000000000000000000, 1.000000000000000000, 1.000000000000000000, 1.000000000000000000, 1.000000000000000000, 1.000000000000000000, 1.000000000000000000, 1.000000000000000000, 1.000000000000000000, 1.000000000000000000, 1.000000000000000000, 1.000000000000000000, 1.000000000000000000, 1.000000000000000000, 1.000000000000000000, 1.000000000000000000, 1.000000000000000000, 1.000000000000000000, 1.000000000000000000),
 ( 0.3333333333333333703, 0.3333333333333333703, 0.3333333333333333703, 0.3333333333333333703, 0.3333333333333333703, 0.3333333333333333703, 0.3333333333333333703, 0.3333333333333333703, 0.3333333333333333703, 0.3333333333333333703, 0.3333333333333333703, 0.3333333333333333703, 0.3333333333333333703, 0.3333333333333333703, 0.3333333333333333703, 0.3333333333333333703, 0.3333333333333333703, 0.3333333333333333703, 0.3333333333333333703, 0.3333333333333333703, 0.3333333333333333703, 0.3333333333333333703, 0.3333333333333333703, 0.3333333333333333703, 0.3333333333333333703, 0.3333333333333333703, 0.3333333333333333703, 0.3333333333333333703, 0.3333333333333333703, 0.3333333333333333703),
 ( 0.3333333333333333703, 0.3333333333333333703, 0.3333333333333333703, 0.3333333333333333703, 0.3333333333333333703, 0.3333333333333333703, 0.3333333333333333703, 0.3333333333333333703, 0.3333333333333333703, 0.3333333333333333703, 0.3333333333333333703, 0.3333333333333333703, 0.3333333333333333703, 0.3333333333333333703, 0.3333333333333333703, 0.3333333333333333703, 0.3333333333333333703, 0.3333333333333333703, 0.3333333333333333703, 0.3333333333333333703, 0.3333333333333333703, 0.3333333333333333703, 0.3333333333333333703, 0.3333333333333333703, 0.3333333333333333703, 0.3333333333333333703, 0.3333333333333333703, 0.3333333333333333703, 0.3333333333333333703, 0.3333333333333333703),
 ( 1.000000000000000000, 1.000000000000000000, 1.000000000000000000, 1.000000000000000000, 1.000000000000000000, 1.000000000000000000, 1.000000000000000000, 1.000000000000000000, 1.000000000000000000, 1.000000000000000000, 1.000000000000000000, 1.000000000000000000, 1.000000000000000000, 1.000000000000000000, 1.000000000000000000, 1.000000000000000000, 1.000000000000000000, 1.000000000000000000, 1.000000000000000000, 1.000000000000000000, 1.000000000000000000, 1.000000000000000000, 1.000000000000000000, 1.000000000000000000, 1.000000000000000000, 1.000000000000000000, 1.000000000000000000, 1.000000000000000000, 1.000000000000000000, 1.000000000000000000) ) ) 
 REPRESENTATION_ITEM ( '' )  SURFACE ( )  );
#20015 = CARTESIAN_POINT ( 'NONE',  ( 37.15749683988774876, -41.79699086507135775, 12.76981037570783606 ) ) ;
#20016 = AXIS2_PLACEMENT_3D ( 'NONE', #11000, #893, #9003 ) ;
#20017 = CARTESIAN_POINT ( 'NONE',  ( 137.0939645874031214, 12.56330697291228837, 30.33050608226204048 ) ) ;
#20018 = B_SPLINE_CURVE_WITH_KNOTS ( 'NONE', 3,
 ( #20590, #14199, #4108, #6345, #24725, #10479 ),
 .UNSPECIFIED., .F., .F.,
 ( 4, 2, 4 ),
 ( 0.3689590070116581244, 0.3867117631979620773, 0.4044645193949217843 ),
 .UNSPECIFIED. ) ;
#20019 = EDGE_CURVE ( 'NONE', #24743, #12221, #2007, .T. ) ;
#20020 = CARTESIAN_POINT ( 'NONE',  ( 57.59792236341147031, 54.84617931850881689, -1.722363176414946073 ) ) ;
#20021 = CARTESIAN_POINT ( 'NONE',  ( -238.4067589809705794, -1.892706720741712928E-13, 40.96449427998260973 ) ) ;
#20022 = VECTOR ( 'NONE', #2163, 1000.000000000000000 ) ;
#20023 = CARTESIAN_POINT ( 'NONE',  ( -192.9588430854690273, 38.51493924976913519, 18.05360324515490333 ) ) ;
#20024 = EDGE_CURVE ( 'NONE', #24679, #433, #22522, .T. ) ;
#20025 = DIRECTION ( 'NONE',  ( 1.000000000000000000, 1.836970198721030181E-16, 0.000000000000000000 ) ) ;
#20026 = CONICAL_SURFACE ( 'NONE', #16624, 75.00000000000000000, 0.4944367829892072352 ) ;
#20027 = CARTESIAN_POINT ( 'NONE',  ( -280.0000000000000000, -20.00000000000006750, 0.000000000000000000 ) ) ;
#20028 = CARTESIAN_POINT ( 'NONE',  ( 170.0000000000000000, 24.95097643317003744, 0.000000000000000000 ) ) ;
#20029 = CARTESIAN_POINT ( 'NONE',  ( 199.9999999999998863, 17.10417011681778732, 8.282922153951966848 ) ) ;
#20030 = CARTESIAN_POINT ( 'NONE',  ( 199.9999999999999716, -14.89501297105162969, 11.81655986308013873 ) ) ;
#20031 = CARTESIAN_POINT ( 'NONE',  ( -208.1127848780265026, 38.89260858015777700, -38.89260858015687461 ) ) ;
#20032 = CARTESIAN_POINT ( 'NONE',  ( -208.1127848780264742, -38.89260858015753541, 17.67593391476614784 ) ) ;
#20033 = CARTESIAN_POINT ( 'NONE',  ( -198.0012279766650636, -14.15883993157157583, 49.19397028317943210 ) ) ;
#20034 = CARTESIAN_POINT ( 'NONE',  ( -82.25678930352327711, 16.86921253968387191, -11.09265870502121309 ) ) ;
#20035 = CARTESIAN_POINT ( 'NONE',  ( -105.3755690713226585, -41.18208027870611687, 15.38646221621750954 ) ) ;
#20037 = LINE ( 'NONE', #24427, #5349 ) ;
#20036 = CARTESIAN_POINT ( 'NONE',  ( 91.82158438592159655, -16.11829626346125011, -16.11829626346154853 ) ) ;
#20038 = CARTESIAN_POINT ( 'NONE',  ( 170.2234770963711128, -17.36149277826940462, -39.20704971665412586 ) ) ;
#20039 = CYLINDRICAL_SURFACE ( 'NONE', #15113, 29.99999999999999645 ) ;
#20040 = CARTESIAN_POINT ( 'NONE',  ( 199.0198855237646569, 7.818582849054650730, 18.41067656382650597 ) ) ;
#20042 = CARTESIAN_POINT ( 'NONE',  ( -135.8532207217289738, -40.00000000000014921, 30.84685318188631697 ) ) ;
#20041 = CARTESIAN_POINT ( 'NONE',  ( -192.9588430854690273, 38.51493924976913519, 18.05360324515490333 ) ) ;
#20043 = CARTESIAN_POINT ( 'NONE',  ( -208.1127848780265026, -10.60833733269551971, 10.60833733269537049 ) ) ;
#20044 = CARTESIAN_POINT ( 'NONE',  ( 170.2234770963711128, 17.36149277826980253, 17.36149277827007253 ) ) ;
#20045 = VECTOR ( 'NONE', #1601, 1000.000000000000000 ) ;
#20046 = CARTESIAN_POINT ( 'NONE',  ( -135.8532207217289738, -9.153146818113595984, 40.00000000000002132 ) ) ;
#20047 = ORIENTED_EDGE ( 'NONE', *, *, #11565, .F. ) ;
#20048 = FACE_OUTER_BOUND ( 'NONE', #3233, .T. ) ;
#20049 = EDGE_CURVE ( 'NONE', #13332, #14842, #20096, .T. ) ;
#20050 = CARTESIAN_POINT ( 'NONE',  ( 80.42747805147106988, 24.86641259896651945, 10.30000534605719942 ) ) ;
#20051 = CARTESIAN_POINT ( 'NONE',  ( 90.68848816912746713, 8.337973097143857260, 21.47805809253356557 ) ) ;
#20052 = CARTESIAN_POINT ( 'NONE',  ( 199.9999999999999432, -20.00000000000006750, 0.000000000000000000 ) ) ;
#20053 = EDGE_LOOP ( 'NONE', ( #21216, #17938 ) ) ;
#20054 = CARTESIAN_POINT ( 'NONE',  ( -199.0731274800660628, -44.83667511839421849, 18.57195892574306484 ) ) ;
#20055 = CARTESIAN_POINT ( 'NONE',  ( 200.0000000000000853, -18.97025941512468705, -1.247367644282773691 ) ) ;
#20056 = CARTESIAN_POINT ( 'NONE',  ( 22.37977766477492381, -23.55755712319357542, 43.15105302556570166 ) ) ;
#20057 = ADVANCED_FACE ( 'NONE', ( #15981 ), #16116, .F. ) ;
#20058 = EDGE_CURVE ( 'NONE', #6112, #6279, #22912, .T. ) ;
#20059 = CARTESIAN_POINT ( 'NONE',  ( 13.08024833509950824, 18.54957993046981812, -44.78264744455110957 ) ) ;
#20060 = CARTESIAN_POINT ( 'NONE',  ( 199.0179304339989415, -16.54579169021749863, -11.23843401478282544 ) ) ;
#20061 = AXIS2_PLACEMENT_3D ( 'NONE', #5836, #1716, #14476 ) ;
#20062 = CARTESIAN_POINT ( 'NONE',  ( 156.5537079553356250, -27.23618587942440783, 11.28159757857190826 ) ) ;
#20063 = CARTESIAN_POINT ( 'NONE',  ( -184.9730489280364338, -22.80026000646345352, 42.02334742177978200 ) ) ;
#20064 = CARTESIAN_POINT ( 'NONE',  ( 19.06497207195980792, 66.60410523465830579, -10.03556273973354251 ) ) ;
#20065 = CARTESIAN_POINT ( 'NONE',  ( -91.56559293963834989, -17.32597176626812896, 40.00000000000002132 ) ) ;
#20067 = CARTESIAN_POINT ( 'NONE',  ( -56.48582580120559982, 21.81201906317729922, 34.75652343174635917 ) ) ;
#20066 = CARTESIAN_POINT ( 'NONE',  ( -188.3066136396869297, 23.45085387054259485, -43.00728998844432027 ) ) ;
#20068 = CARTESIAN_POINT ( 'NONE',  ( 19.06497207195981503, -14.19242893257840166, 0.000000000000000000 ) ) ;
#20069 = CARTESIAN_POINT ( 'NONE',  ( -198.0356074513804572, -15.37879056873074290, -40.00000000000002132 ) ) ;
#20070 = CARTESIAN_POINT ( 'NONE',  ( -280.0000000000000568, 19.99999999999995737, 40.00000000000002132 ) ) ;
#20071 = CARTESIAN_POINT ( 'NONE',  ( 136.1360204305621266, 7.947488714877270288E-14, -4.966164525587064560 ) ) ;
#20072 = CARTESIAN_POINT ( 'NONE',  ( 170.2234770963711128, 10.92277846919201068, 10.92277846919202133 ) ) ;
#20073 = CARTESIAN_POINT ( 'NONE',  ( 151.7948205124836250, -3.202120068677277203E-13, 33.23291073765553705 ) ) ;
#20074 = CARTESIAN_POINT ( 'NONE',  ( 136.1360204305621266, 53.05693388239320285, -3.511608612530223716 ) ) ;
#20075 = ORIENTED_EDGE ( 'NONE', *, *, #20172, .T. ) ;
#20076 = CARTESIAN_POINT ( 'NONE',  ( -135.8532207217289738, -6.472252184284190690, -6.472252184284188914 ) ) ;
#20077 = DIRECTION ( 'NONE',  ( 0.000000000000000000, 1.000000000000000000, 0.000000000000000000 ) ) ;
#20078 = CARTESIAN_POINT ( 'NONE',  ( -93.01741312764214342, -8.169811846330309990, 20.82169463875505500 ) ) ;
#20079 = PRODUCT_CONTEXT ( 'NONE', #21093, 'mechanical' ) ;
#20080 = ORIENTED_EDGE ( 'NONE', *, *, #4556, .F. ) ;
#20081 = ORIENTED_EDGE ( 'NONE', *, *, #4263, .F. ) ;
#20082 = CARTESIAN_POINT ( 'NONE',  ( 130.8568914410475088, -32.49135343045460900, -24.07718906446924478 ) ) ;
#20083 = CARTESIAN_POINT ( 'NONE',  ( 23.36927571439214901, -46.80992244775434585, -13.80130822340160002 ) ) ;
#20084 = ORIENTED_EDGE ( 'NONE', *, *, #5807, .T. ) ;
#20085 = CARTESIAN_POINT ( 'NONE',  ( -280.0000000000000568, -20.00000000000006750, -40.00000000000002132 ) ) ;
#20086 = LINE ( 'NONE', #6111, #10459 ) ;
#20087 = ORIENTED_EDGE ( 'NONE', *, *, #23231, .F. ) ;
#20088 = CARTESIAN_POINT ( 'NONE',  ( 200.0000000000000284, 7.828075510571024687, 17.32306842307162142 ) ) ;
#20089 = DIRECTION ( 'NONE',  ( -1.000000000000000000, -1.836970198721030181E-16, 0.000000000000000000 ) ) ;
#20090 = CARTESIAN_POINT ( 'NONE',  ( 151.7948205124836534, 4.785054706298574878, -51.78348778862537927 ) ) ;
#20091 = CARTESIAN_POINT ( 'NONE',  ( -188.3509229510420937, -43.15764231844811150, -17.87648076834712185 ) ) ;
#20092 = CARTESIAN_POINT ( 'NONE',  ( -238.4067589809705794, -1.892706720741712928E-13, 40.96449427998260973 ) ) ;
#20093 = CARTESIAN_POINT ( 'NONE',  ( 57.59792236341147031, -2.435789363418150444, 0.000000000000000000 ) ) ;
#20094 = CARTESIAN_POINT ( 'NONE',  ( -56.48582580120559271, 21.81201906317798489, -21.81201906317746619 ) ) ;
#20095 = CARTESIAN_POINT ( 'NONE',  ( 199.0241407150285227, -2.291925048877014870, 19.87495682421008425 ) ) ;
#20096 = B_SPLINE_CURVE_WITH_KNOTS ( 'NONE', 3,
 ( #1632, #11861, #1763, #7998, #9871, #7862 ),
 .UNSPECIFIED., .F., .F.,
 ( 4, 2, 4 ),
 ( -6.000000000418191541E-08, 0.04016968421219337809, 0.08033942842438676624 ),
 .UNSPECIFIED. ) ;
#20097 = CARTESIAN_POINT ( 'NONE',  ( -162.0762913951021176, -40.00000000000019895, 41.69427287672974813 ) ) ;
#20098 = CARTESIAN_POINT ( 'NONE',  ( 19.06497207195981858, -39.99999999999987210, -14.19242893257882621 ) ) ;
#20099 = CARTESIAN_POINT ( 'NONE',  ( -105.2109270643165218, -16.13380223201193076, 14.21138704488140192 ) ) ;
#20100 = CARTESIAN_POINT ( 'NONE',  ( 192.4448373802100889, -14.14213562370313682, 14.14213562370301958 ) ) ;
#20101 = CARTESIAN_POINT ( 'NONE',  ( -162.0762913951020892, -1.694272876828353702, 0.000000000000000000 ) ) ;
#20102 = CARTESIAN_POINT ( 'NONE',  ( -238.4067589809705794, -57.25054294065807881, 0.6820004457338858517 ) ) ;
#20103 = CARTESIAN_POINT ( 'NONE',  ( -362.0709805440841365, -4.734761052820324716E-14, -9.999999999999998224 ) ) ;
#20104 = DIRECTION ( 'NONE',  ( -1.000000000000000000, 0.000000000000000000, 0.000000000000000000 ) ) ;
#20105 = CARTESIAN_POINT ( 'NONE',  ( 170.2234770963711128, -2.259079968736224833E-13, 24.55285855007187124 ) ) ;
#20106 = CARTESIAN_POINT ( 'NONE',  ( -198.0356074513804572, -9.007331120208026888E-14, 15.37879056873070560 ) ) ;
#20107 = CARTESIAN_POINT ( 'NONE',  ( -30.26275506840325136, 29.48230279907798135, -27.08623969584585112 ) ) ;
#20108 = FACE_BOUND ( 'NONE', #21334, .T. ) ;
#20109 = CARTESIAN_POINT ( 'NONE',  ( -189.2667921706123479, -17.97629039507333104, -43.39860407294602851 ) ) ;
#20110 = DIRECTION ( 'NONE',  ( 1.000000000000000000, -0.000000000000000000, -0.000000000000000000 ) ) ;
#20111 = ORIENTED_EDGE ( 'NONE', *, *, #4779, .F. ) ;
#20112 = CARTESIAN_POINT ( 'NONE',  ( 192.4448373802101173, -14.14213562375826605, -42.42640687116518450 ) ) ;
#20113 = CARTESIAN_POINT ( 'NONE',  ( -105.4741150117390021, -8.366608964578313490, 19.60045294983322961 ) ) ;
#20114 = CARTESIAN_POINT ( 'NONE',  ( -114.5523123854244005, 6.807555700458402193, 20.89198064830843649 ) ) ;
#20115 = CARTESIAN_POINT ( 'NONE',  ( -83.21262154144247347, -33.12752917118416462, -13.72187187061500069 ) ) ;
#20116 = CARTESIAN_POINT ( 'NONE',  ( 184.8905102610680444, 13.49065550809826952, -13.49065550809790359 ) ) ;
#20117 = CARTESIAN_POINT ( 'NONE',  ( -198.9233928135560916, -24.80620717269025732, -44.84148042516699917 ) ) ;
#20118 = CARTESIAN_POINT ( 'NONE',  ( -87.10437264496880516, 2.718829733098547585, 21.30276644673244490 ) ) ;
#20119 = ORIENTED_EDGE ( 'NONE', *, *, #18722, .F. ) ;
#20120 = CARTESIAN_POINT ( 'NONE',  ( 199.9999999999999432, 12.51862865053690577, 14.30364628684430706 ) ) ;
#20121 = CARTESIAN_POINT ( 'NONE',  ( -105.4741150117382915, -19.60045294982753461, 8.366608964593266862 ) ) ;
#20122 = CARTESIAN_POINT ( 'NONE',  ( -3.993758944537799671, 23.45926997169888040, 43.01863922058791445 ) ) ;
#20123 = ORIENTED_EDGE ( 'NONE', *, *, #25999, .T. ) ;
#20124 = ORIENTED_EDGE ( 'NONE', *, *, #7510, .T. ) ;
#20125 = CARTESIAN_POINT ( 'NONE',  ( 163.1118516004056573, -27.26290988616869626, 0.000000000000000000 ) ) ;
#20126 = CARTESIAN_POINT ( 'NONE',  ( 199.0076473327615645, 2.278485796641462446, -19.86629856447459375 ) ) ;
#20127 = DIRECTION ( 'NONE',  ( -1.000000000000000000, 0.000000000000000000, 0.000000000000000000 ) ) ;
#20128 = ADVANCED_FACE ( 'NONE', ( #18512 ), #10804, .T. ) ;
#20129 = CARTESIAN_POINT ( 'NONE',  ( -103.9663809733204118, -8.574562931466585880, -19.92521373417671526 ) ) ;
#20130 = CARTESIAN_POINT ( 'NONE',  ( -213.1075012329537230, 1.045191102001431893E-13, -13.71589010951911902 ) ) ;
#20131 = CARTESIAN_POINT ( 'NONE',  ( -362.0709805440841365, -4.857225732735059864E-14, 0.000000000000000000 ) ) ;
#20132 = CARTESIAN_POINT ( 'NONE',  ( -640.4516436576406022, 29.67861829237677540, -26.82428473879609143 ) ) ;
#20133 = DIRECTION ( 'NONE',  ( 1.000000000000000000, 0.000000000000000000, 0.000000000000000000 ) ) ;
#20134 = CARTESIAN_POINT ( 'NONE',  ( 199.0164010208656009, 13.53619804287660777, 14.72436343555392035 ) ) ;
#20135 = CARTESIAN_POINT ( 'NONE',  ( -188.3485952524935669, 42.24825774596409644, 17.49980134501263507 ) ) ;
#20136 = CARTESIAN_POINT ( 'NONE',  ( -4.558244102846323642, -23.34817229225983581, -42.85231560262757711 ) ) ;
#20137 = CARTESIAN_POINT ( 'NONE',  ( 146.6084372240433709, 24.48358557860356655, -32.08495691632035118 ) ) ;
#20138 = CARTESIAN_POINT ( 'NONE',  ( -200.0000000000000284, 17.28402242884629914, 46.84854965773176616 ) ) ;
#20139 = CARTESIAN_POINT ( 'NONE',  ( 0.2972598230770100991, -38.42060263243686791, 38.42060263243645579 ) ) ;
#20140 = CARTESIAN_POINT ( 'NONE',  ( 4.995406935893297984, -39.99999999999986500, -15.24977328854874870 ) ) ;
#20141 = FACE_OUTER_BOUND ( 'NONE', #6801, .T. ) ;
#20142 = CARTESIAN_POINT ( 'NONE',  ( 14.38125909742182884, -55.17850393971007605, 40.00000000000002132 ) ) ;
#20143 = CARTESIAN_POINT ( 'NONE',  ( 170.2234770963711128, 17.36149277827004411, -17.36149277826983095 ) ) ;
#20144 = CARTESIAN_POINT ( 'NONE',  ( -259.2033419157646676, -30.48217210827744950, 40.00000000000002132 ) ) ;
#20145 = CARTESIAN_POINT ( 'NONE',  ( -110.0692149585521946, 10.04884809978941185, 17.50500459063693626 ) ) ;
#20146 = CARTESIAN_POINT ( 'NONE',  ( -86.96347745069645896, 40.00000000000019895, -18.24025645688310249 ) ) ;
#20147 = CARTESIAN_POINT ( 'NONE',  ( 200.0000000000000000, 14.14213562373100608, -42.42640687119291698 ) ) ;
#20148 = CARTESIAN_POINT ( 'NONE',  ( -238.4067589809705794, 0.9644942799825386714, 0.000000000000000000 ) ) ;
#20149 = ORIENTED_EDGE ( 'NONE', *, *, #25230, .F. ) ;
#20150 = CARTESIAN_POINT ( 'NONE',  ( -105.3755690713226585, -21.75974354311652448, 40.00000000000002132 ) ) ;
#20151 = CARTESIAN_POINT ( 'NONE',  ( -199.9999999999999716, -35.57044988732110369, -42.45148791631905283 ) ) ;
#20152 = CARTESIAN_POINT ( 'NONE',  ( -100.7734535825088500, -40.00000000000009948, 17.32597176626796909 ) ) ;
#20153 = CARTESIAN_POINT ( 'NONE',  ( 4.995406935893283773, 39.06748935135171052, 17.50105314357239195 ) ) ;
#20154 = CARTESIAN_POINT ( 'NONE',  ( 19.06497207195980792, 14.19242893257840876, 0.000000000000000000 ) ) ;
#20155 = CARTESIAN_POINT ( 'NONE',  ( -189.2428623074474103, -43.27185639470908285, -23.64699222226066766 ) ) ;
#20156 = PRODUCT_DEFINITION_SHAPE ( 'NONE', 'NONE',  #17991 ) ;
#20157 = FACE_OUTER_BOUND ( 'NONE', #26223, .T. ) ;
#20158 = CARTESIAN_POINT ( 'NONE',  ( 200.0000000000001421, 16.91347576093571803, -8.662591770200990027 ) ) ;
#20159 = CARTESIAN_POINT ( 'NONE',  ( 199.9999999999999432, -15.45674197124598592, 11.06829513483084426 ) ) ;
#20160 = CARTESIAN_POINT ( 'NONE',  ( -91.56559293963834989, 12.25131212657497848, -12.25131212657469426 ) ) ;
#20161 = CARTESIAN_POINT ( 'NONE',  ( -213.1075012329537230, -37.98287015391257881, 18.58567234101111509 ) ) ;
#20162 = CARTESIAN_POINT ( 'NONE',  ( -105.2080558454215407, 21.47607500789820278, 1.614329345468047183 ) ) ;
#20163 = CARTESIAN_POINT ( 'NONE',  ( -198.0356074513804572, 1.247057299367198800E-13, -15.37879056873070560 ) ) ;
#20164 = CARTESIAN_POINT ( 'NONE',  ( -30.26275506840322294, -57.76657404653985139, -1.198031551616531853 ) ) ;
#20165 = CARTESIAN_POINT ( 'NONE',  ( -87.13361725327075646, 14.71749760136616558, -15.67849882405064932 ) ) ;
#20166 = CARTESIAN_POINT ( 'NONE',  ( 136.1360204305621551, -24.77266263493081766, -31.79587985999290112 ) ) ;
#20167 = CARTESIAN_POINT ( 'NONE',  ( -100.7734535825088500, 16.03295912088713848, -16.03295912088698927 ) ) ;
#20168 = CARTESIAN_POINT ( 'NONE',  ( 199.0199585884774649, 7.679342959448028694, 18.46907803347260213 ) ) ;
#20170 = CARTESIAN_POINT ( 'NONE',  ( -30.26275506840323359, -40.00000000000017053, 41.69427246844613677 ) ) ;
#20169 = CARTESIAN_POINT ( 'NONE',  ( 4.995406935893297984, 10.78321810390233892, -67.35176059882522281 ) ) ;
#20171 = CARTESIAN_POINT ( 'NONE',  ( 19.06497207195981147, -10.03556273973425483, -10.03556273973443247 ) ) ;
#20172 = EDGE_CURVE ( 'NONE', #21778, #2862, #23431, .T. ) ;
#20173 = CARTESIAN_POINT ( 'NONE',  ( 23.64688638900461015, 42.77321027809668408, -23.28414885118040445 ) ) ;
#20174 = CARTESIAN_POINT ( 'NONE',  ( 0.2972598230769930572, 54.33493731733936016, 2.449293598294708485E-15 ) ) ;
#20175 = EDGE_LOOP ( 'NONE', ( #8531, #19206, #10965, #14845 ) ) ;
#20176 = CARTESIAN_POINT ( 'NONE',  ( 7.340276910564544011, -24.82763627182848154, -44.87059041559408001 ) ) ;
#20177 = CARTESIAN_POINT ( 'NONE',  ( 20.31814284189117004, 42.80521382620615611, 17.73050010709527768 ) ) ;
#20178 = LINE ( 'NONE', #9931, #19216 ) ;
#20179 = CARTESIAN_POINT ( 'NONE',  ( 184.8905102610680444, -20.92133201514440799, 0.000000000000000000 ) ) ;
#20180 = ORIENTED_EDGE ( 'NONE', *, *, #536, .T. ) ;
#20181 = CARTESIAN_POINT ( 'NONE',  ( -189.1288337602814238, -47.28029723722803368, 13.87115233298298733 ) ) ;
#20182 = CARTESIAN_POINT ( 'NONE',  ( 199.9999999999996589, -18.97053056118941328, 1.250588282361275283 ) ) ;
#20183 = CARTESIAN_POINT ( 'NONE',  ( 9.345847406360801912, -24.85453859511385488, 44.90706793518310036 ) ) ;
#20184 =( GEOMETRIC_REPRESENTATION_CONTEXT ( 3 ) GLOBAL_UNCERTAINTY_ASSIGNED_CONTEXT ( ( #19213 ) ) GLOBAL_UNIT_ASSIGNED_CONTEXT ( ( #10268, #14387, #2695 ) ) REPRESENTATION_CONTEXT ( 'NONE', 'WORKASPACE' ) );
#20185 = CARTESIAN_POINT ( 'NONE',  ( 21.80484139881497185, 17.98806631651988397, -43.42703366220747085 ) ) ;
#20186 = CARTESIAN_POINT ( 'NONE',  ( 199.0200497209392267, -18.54142962866078648, -7.504851164020625021 ) ) ;
#20187 = CARTESIAN_POINT ( 'NONE',  ( 164.1122551457365546, -24.38379312608502403, 10.10009781492401082 ) ) ;
#20188 = CARTESIAN_POINT ( 'NONE',  ( -188.3509229510694638, -17.87648076834458521, 43.15764231845329846 ) ) ;
#20189 = ADVANCED_FACE ( 'NONE', ( #18914 ), #24215, .T. ) ;
#20190 = CARTESIAN_POINT ( 'NONE',  ( -100.7734535825088358, 12.25131212657497848, -12.25131212657469604 ) ) ;
#20191 = CARTESIAN_POINT ( 'NONE',  ( -213.1075012329537230, -13.71589010951915810, 0.000000000000000000 ) ) ;
#20192 = COLOUR_RGB ( '',0.7921568627450980005, 0.8196078431372548767, 0.9333333333333333481 ) ;
#20193 = CIRCLE ( 'NONE', #13791, 4.999999999999962697 ) ;
#20195 = CARTESIAN_POINT ( 'NONE',  ( 130.8568914410475372, -24.07718906447255947, 24.07718906447199458 ) ) ;
#20194 = CARTESIAN_POINT ( 'NONE',  ( -188.4702232936889459, 13.83721295434279774, -47.05182887786761370 ) ) ;
#20196 = CARTESIAN_POINT ( 'NONE',  ( -114.4364955367327070, 8.644468109209567430, -20.04994829327642947 ) ) ;
#20197 = B_SPLINE_CURVE_WITH_KNOTS ( 'NONE', 3,
 ( #22033, #25896, #16028, #26034, #20033, #9515 ),
 .UNSPECIFIED., .F., .F.,
 ( 4, 2, 4 ),
 ( -5.998616628085171876E-08, 0.005995031700373180950, 0.01199012338691264265 ),
 .UNSPECIFIED. ) ;
#20198 = CARTESIAN_POINT ( 'NONE',  ( 0.2972598230769983307, -14.33493731733933352, -40.00000000000002132 ) ) ;
#20199 = CARTESIAN_POINT ( 'NONE',  ( 199.9999999999999432, 19.99999999999996092, 2.449293598294708485E-15 ) ) ;
#20200 = CARTESIAN_POINT ( 'NONE',  ( -91.56559293963834989, 1.671088883502053755E-13, -17.32597176626811120 ) ) ;
#20201 = CARTESIAN_POINT ( 'NONE',  ( -259.2033419157646676, 49.83842185052027673, -6.730120644403441155 ) ) ;
#20202 = CARTESIAN_POINT ( 'NONE',  ( 98.29820294267166503, -13.21553301705472627, 15.06873823041648031 ) ) ;
#20203 = CARTESIAN_POINT ( 'NONE',  ( 192.4448373802100889, 14.14213562375873678, 14.14213562375894817 ) ) ;
#20204 = EDGE_CURVE ( 'NONE', #10094, #23960, #16917, .T. ) ;
#20205 = EDGE_CURVE ( 'NONE', #4362, #23332, #22322, .T. ) ;
#20206 = ORIENTED_EDGE ( 'NONE', *, *, #12873, .T. ) ;
#20207 = CARTESIAN_POINT ( 'NONE',  ( 151.7948205124836250, -23.49921654116339553, -23.49921654116350211 ) ) ;
#20208 = CARTESIAN_POINT ( 'NONE',  ( -96.94449363882321791, -8.590991630976864357, 20.74048850979724534 ) ) ;
#20209 = APPLICATION_PROTOCOL_DEFINITION ( 'draft international standard', 'automotive_design', 1998, #19366 ) ;
#20210 = ORIENTED_EDGE ( 'NONE', *, *, #8633, .F. ) ;
#20211 = ORIENTED_EDGE ( 'NONE', *, *, #14818, .T. ) ;
#20212 = CARTESIAN_POINT ( 'NONE',  ( 136.1360204305621551, -31.79587985999244282, -24.77266263493140386 ) ) ;
#20213 = CARTESIAN_POINT ( 'NONE',  ( 37.37129771729572525, -38.51719860174896581, -20.48130208320684531 ) ) ;
#20214 = EDGE_LOOP ( 'NONE', ( #11122, #11430, #12477, #11549 ) ) ;
#20215 = CARTESIAN_POINT ( 'NONE',  ( 192.4448373802101173, -20.00000000003938538, -40.00000000000002132 ) ) ;
#20216 = CARTESIAN_POINT ( 'NONE',  ( -103.9650464694730374, -20.03380587394293144, 8.298274102034335797 ) ) ;
#20217 = EDGE_LOOP ( 'NONE', ( #23336, #26227, #12723, #9311 ) ) ;
#20218 = CARTESIAN_POINT ( 'NONE',  ( 199.9999999999999716, 8.673909288817675645, 16.91296503504769078 ) ) ;
#20219 = AXIS2_PLACEMENT_3D ( 'NONE', #9749, #11869, #23471 ) ;
#20220 = VECTOR ( 'NONE', #983, 1000.000000000000000 ) ;
#20221 = CARTESIAN_POINT ( 'NONE',  ( -105.3841539895568786, 20.33898584361668682, -6.698820788730287745 ) ) ;
#20222 = CARTESIAN_POINT ( 'NONE',  ( -56.48582580120559271, -6.472252184284187138, -6.472252184284199572 ) ) ;
#20223 = CARTESIAN_POINT ( 'NONE',  ( -188.2652746676488960, -42.99511404081843580, -23.44263257803740785 ) ) ;
#20224 = CARTESIAN_POINT ( 'NONE',  ( -86.96347745069643054, -39.99999999999995737, -21.75974354311664527 ) ) ;
#20225 = CARTESIAN_POINT ( 'NONE',  ( -91.56559293963834989, -22.67402823373193499, 0.000000000000000000 ) ) ;
#20226 = CARTESIAN_POINT ( 'NONE',  ( 146.6084372240433709, -24.48358557860284179, -32.08495691632087699 ) ) ;
#20227 = CARTESIAN_POINT ( 'NONE',  ( 199.0214920807345322, 4.534629261753806873, 19.48466678343157454 ) ) ;
#20228 = VECTOR ( 'NONE', #18794, 1000.000000000000000 ) ;
#20229 = CARTESIAN_POINT ( 'NONE',  ( 57.59792236341147031, 1.908507979671054758E-14, -2.435789363418160658 ) ) ;
#20230 = CARTESIAN_POINT ( 'NONE',  ( 146.6084372240433993, 5.715592784339989804E-15, 5.374981219216972583 ) ) ;
#20231 = CARTESIAN_POINT ( 'NONE',  ( -105.3755690713226727, -2.472783935621397949E-13, 21.75974354311649961 ) ) ;
#20232 = CARTESIAN_POINT ( 'NONE',  ( 163.1118516004056573, 40.00000000000014921, -27.26290988616858968 ) ) ;
#20233 = CARTESIAN_POINT ( 'NONE',  ( -208.1127848780265026, -15.00245453012673202, 0.000000000000000000 ) ) ;
#20234 = CARTESIAN_POINT ( 'NONE',  ( 199.9999999999999432, -14.14213562373093680, 14.14213562373082311 ) ) ;
#20235 = CARTESIAN_POINT ( 'NONE',  ( -280.0000000000000000, 19.99999999999996092, -0.000000000000000000 ) ) ;
#20236 = CARTESIAN_POINT ( 'NONE',  ( -259.2033419157646676, -21.55415060305824326, -35.01439189186556433 ) ) ;
#20237 = CARTESIAN_POINT ( 'NONE',  ( -97.72675010090208048, -8.987772175319811652, 20.56394680065903202 ) ) ;
#20238 = CARTESIAN_POINT ( 'NONE',  ( 23.09931156284630305, -46.91113948292957758, 13.81622350327238458 ) ) ;
#20239 = CARTESIAN_POINT ( 'NONE',  ( -30.26275506840325136, 40.00000000000003553, -1.694272468445841007 ) ) ;
#20240 = CARTESIAN_POINT ( 'NONE',  ( -56.48582580120558561, -1.205267837095813407E-13, 30.84685318188644132 ) ) ;
#20241 = CARTESIAN_POINT ( 'NONE',  ( 163.1118516004056573, 9.006482792069629539, 9.006482792069634868 ) ) ;
#20242 = AXIS2_PLACEMENT_3D ( 'NONE', #14251, #10000, #23966 ) ;
#20243 = CARTESIAN_POINT ( 'NONE',  ( -114.6329851429147482, 11.24672612388742543, 18.91064981619980756 ) ) ;
#20244 = CARTESIAN_POINT ( 'NONE',  ( -189.0115661350361336, -17.94954792649098607, -43.33404204260301640 ) ) ;
#20245 = CARTESIAN_POINT ( 'NONE',  ( -56.48582580120559271, 6.472252184284211118, -6.472252184284153387 ) ) ;
#20246 = ORIENTED_EDGE ( 'NONE', *, *, #14530, .F. ) ;
#20247 = CARTESIAN_POINT ( 'NONE',  ( 4.995406935893289102, 10.78321810389013002, -10.78321810388986712 ) ) ;
#20248 = CARTESIAN_POINT ( 'NONE',  ( -678.9461782662789346, 75.00000000000000000, -29.99999999999836220 ) ) ;
#20249 = CARTESIAN_POINT ( 'NONE',  ( -213.1075012329537230, -13.71589010951915810, -40.00000000000002132 ) ) ;
#20250 = CARTESIAN_POINT ( 'NONE',  ( 151.7948205124836534, -23.49921654115981084, -33.06932595376387951 ) ) ;
#20251 = CARTESIAN_POINT ( 'NONE',  ( -77.78745312868143458, 6.815361097864228945, 20.88824371463043761 ) ) ;
#20252 = EDGE_LOOP ( 'NONE', ( #15048, #15421, #21584, #19359, #21428, #15302, #16283, #24550 ) ) ;
#20253 = CARTESIAN_POINT ( 'NONE',  ( 199.9999999999999716, 17.67195306284541090, 6.994325408928051324 ) ) ;
#20254 = CARTESIAN_POINT ( 'NONE',  ( -16.41594856591132157, -21.03672847018052394, -39.35878123509505855 ) ) ;
#20255 = CARTESIAN_POINT ( 'NONE',  ( -4.037857402786209526, 23.44963359339744002, 43.00569567200292198 ) ) ;
#20256 = AXIS2_PLACEMENT_3D ( 'NONE', #9323, #25443, #5091 ) ;
#20257 = ORIENTED_EDGE ( 'NONE', *, *, #11744, .T. ) ;
#20258 = CIRCLE ( 'NONE', #23639, 15.00000000000000000 ) ;
#20259 = VERTEX_POINT ( 'NONE', #9065 ) ;
#20260 = CARTESIAN_POINT ( 'NONE',  ( 192.4448373802101173, -20.00000000003938538, -40.00000000000002132 ) ) ;
#20261 = CARTESIAN_POINT ( 'NONE',  ( 199.0058919196228260, 8.838798596736017643, -17.93603902042922726 ) ) ;
#20262 = LINE ( 'NONE', #2041, #5559 ) ;
#20263 = CARTESIAN_POINT ( 'NONE',  ( 98.29820294270297154, 18.47759065022021474, -7.653668647299666894 ) ) ;
#20264 = CARTESIAN_POINT ( 'NONE',  ( -105.4732637872235443, -8.153770687239559223, -19.68494377761379610 ) ) ;
#20265 = CARTESIAN_POINT ( 'NONE',  ( -30.26275506840325136, 40.00000000000003553, -1.694272468445841007 ) ) ;
#20266 = CARTESIAN_POINT ( 'NONE',  ( 200.0000000000000853, -18.00470042792477798, 6.107801588486966082 ) ) ;
#20267 = CARTESIAN_POINT ( 'NONE',  ( -77.90255099906771363, -20.29001641120656174, -8.064892378658559124 ) ) ;
#20268 = CARTESIAN_POINT ( 'NONE',  ( -114.7826396787322665, -15.64922767586156915, -15.64922767586183383 ) ) ;
#20269 = CARTESIAN_POINT ( 'NONE',  ( 199.0219179450577371, 3.573952992290374109, 19.68174087806957573 ) ) ;
#20270 = FACE_OUTER_BOUND ( 'NONE', #13216, .T. ) ;
#20271 = CARTESIAN_POINT ( 'NONE',  ( 8.209392600928307360, -24.84362085272598364, -44.89226883836247595 ) ) ;
#20272 = CARTESIAN_POINT ( 'NONE',  ( 146.6084372240433993, -3.800685668858596156, -3.800685668858692967 ) ) ;
#20273 = AXIS2_PLACEMENT_3D ( 'NONE', #23849, #24126, #13733 ) ;
#20274 = CARTESIAN_POINT ( 'NONE',  ( -114.7544849858170721, 2.764938904914928219, -21.97700360082519566 ) ) ;
#20275 = CARTESIAN_POINT ( 'NONE',  ( 151.7948205124835681, -4.785054706298153882, -51.78348778862540058 ) ) ;
#20276 = CARTESIAN_POINT ( 'NONE',  ( -192.9588430854690273, -39.99999999999991473, -14.46834944100011633 ) ) ;
#20277 = FACE_BOUND ( 'NONE', #3172, .T. ) ;
#20278 = CARTESIAN_POINT ( 'NONE',  ( -259.2033419157646676, 9.517827891722582478, 40.00000000000002132 ) ) ;
#20279 = FACE_OUTER_BOUND ( 'NONE', #4957, .T. ) ;
#20280 = CARTESIAN_POINT ( 'NONE',  ( 4.995406935893307754, -55.24977328853207581, -40.00000000000002132 ) ) ;
#20281 = CARTESIAN_POINT ( 'NONE',  ( -110.0568454066791730, 9.184575013437996205, 17.97667584252678807 ) ) ;
#20282 = CARTESIAN_POINT ( 'NONE',  ( -208.1127848780265026, 5.403397259664334602E-13, -55.00245453012672670 ) ) ;
#20283 = CARTESIAN_POINT ( 'NONE',  ( -91.56559293963834989, 12.25131212657490209, -44.31723036834897300 ) ) ;
#20284 = CARTESIAN_POINT ( 'NONE',  ( -213.1075012329537230, 13.71589010951907994, 0.000000000000000000 ) ) ;
#20285 = ORIENTED_EDGE ( 'NONE', *, *, #8162, .T. ) ;
#20286 = ORIENTED_EDGE ( 'NONE', *, *, #22352, .F. ) ;
#20287 = CARTESIAN_POINT ( 'NONE',  ( 192.4448373802101173, -20.00000000003938538, 40.00000000000002132 ) ) ;
#20288 = CARTESIAN_POINT ( 'NONE',  ( -102.4068193528146651, -8.088405365068982888, -20.44188272012847918 ) ) ;
#20289 = CARTESIAN_POINT ( 'NONE',  ( 151.7948205124836534, -40.00000000000001421, 6.767089262348889633 ) ) ;
#20290 = CARTESIAN_POINT ( 'NONE',  ( -192.9588430854690273, 66.79921049724377724, -10.23066800231904239 ) ) ;
#20291 = CARTESIAN_POINT ( 'NONE',  ( 192.4448373802100889, -20.00000000003938538, 0.000000000000000000 ) ) ;
#20292 = EDGE_CURVE ( 'NONE', #21913, #9180, #11939, .T. ) ;
#20293 = DIRECTION ( 'NONE',  ( 1.000000000000000000, 1.836970198721030181E-16, -0.000000000000000000 ) ) ;
#20294 = CARTESIAN_POINT ( 'NONE',  ( -188.2995950289365226, 23.44932284465886241, 43.00522595870971543 ) ) ;
#20295 = CARTESIAN_POINT ( 'NONE',  ( 200.0000000000001137, 17.30391983412833667, 7.856783789979721710 ) ) ;
#20296 = UNCERTAINTY_MEASURE_WITH_UNIT (LENGTH_MEASURE( 1.000000000000000082E-05 ), #22388, 'distance_accuracy_value', 'NONE');
#20297 = CARTESIAN_POINT ( 'NONE',  ( 199.9999999999999147, -12.54514294966348409, -14.28960723841028546 ) ) ;
#20298 = CARTESIAN_POINT ( 'NONE',  ( -280.0000000000000568, -14.14213562373049449, -42.42640687119305198 ) ) ;
#20299 = CARTESIAN_POINT ( 'NONE',  ( -105.3755690713226585, -41.18208027870611687, 15.38646221621750954 ) ) ;
#20300 = CARTESIAN_POINT ( 'NONE',  ( -114.7464620073225348, 21.93325705637180079, 3.051371648169525663 ) ) ;
#20301 = CARTESIAN_POINT ( 'NONE',  ( 0.2972598230769957217, 1.502051041545559470E-13, -14.33493731733933352 ) ) ;
#20302 = CARTESIAN_POINT ( 'NONE',  ( -238.4067589809705794, -57.25054294077233408, -0.6820004458489551391 ) ) ;
#20303 = CARTESIAN_POINT ( 'NONE',  ( 130.8568914410475372, -24.07718906447255947, 24.07718906447199458 ) ) ;
#20304 = CARTESIAN_POINT ( 'NONE',  ( 184.8905102610680444, -14.79361573936379415, -14.79361573936387941 ) ) ;
#20305 = CARTESIAN_POINT ( 'NONE',  ( -56.48582580120559982, -21.81201906317755501, -34.75652343174621706 ) ) ;
#20306 = CARTESIAN_POINT ( 'NONE',  ( 199.0213085020154153, 4.963412175948412219, 19.42123122998796703 ) ) ;
#20307 = EDGE_CURVE ( 'NONE', #12520, #3292, #11494, .T. ) ;
#20309 = CARTESIAN_POINT ( 'NONE',  ( 163.1118516004056573, -1.695744499706194789E-14, 12.73709011382475254 ) ) ;
#20308 = CARTESIAN_POINT ( 'NONE',  ( 170.2234770963711128, 10.92277846919216522, -10.92277846919186501 ) ) ;
#20310 = CARTESIAN_POINT ( 'NONE',  ( 57.59792236341147031, 26.56190807104652052, 30.00663442387728708 ) ) ;
#20311 = CARTESIAN_POINT ( 'NONE',  ( 23.49666234703892442, 46.76389514419409466, -13.79192166426290633 ) ) ;
#20312 = CARTESIAN_POINT ( 'NONE',  ( -86.96347745069644475, 18.24025645688350750, -40.00000000000002132 ) ) ;
#20313 = EDGE_LOOP ( 'NONE', ( #8999, #1866, #10737, #17161 ) ) ;
#20314 = CYLINDRICAL_SURFACE ( 'NONE', #4795, 5.000000000000011546 ) ;
#20315 = B_SPLINE_CURVE_WITH_KNOTS ( 'NONE', 3,
 ( #15138, #10899, #25398, #19392, #25267, #1046 ),
 .UNSPECIFIED., .F., .F.,
 ( 4, 2, 4 ),
 ( 3.836816584462350783E-15, 0.03937634048171193696, 0.07875268096342002977 ),
 .UNSPECIFIED. ) ;
#20316 = CARTESIAN_POINT ( 'NONE',  ( -8.197988474474012577, -42.01088836872121135, 17.40147972967339385 ) ) ;
#20317 = CARTESIAN_POINT ( 'NONE',  ( -238.4067589809705794, 0.9644942799825385604, 40.00000000000002132 ) ) ;
#20318 = ORIENTED_EDGE ( 'NONE', *, *, #10475, .T. ) ;
#20319 = DIRECTION ( 'NONE',  ( -1.000000000000000000, -1.836970198721030427E-16, 0.000000000000000000 ) ) ;
#20320 = DIRECTION ( 'NONE',  ( -1.000000000000000000, -0.000000000000000000, -0.000000000000000000 ) ) ;
#20321 = CARTESIAN_POINT ( 'NONE',  ( 22.01478053667031176, -23.63228119973013008, 43.25192662397473953 ) ) ;
#20322 = CARTESIAN_POINT ( 'NONE',  ( 19.66474694218035424, 18.18658454059308482, -43.90629905111418196 ) ) ;
#20323 = CARTESIAN_POINT ( 'NONE',  ( 199.0120775374408311, -7.960707704260069129, -18.34818886981279462 ) ) ;
#20324 = CARTESIAN_POINT ( 'NONE',  ( -90.07798792367799479, -15.74993999324200011, 15.74993999324160399 ) ) ;
#20325 = CARTESIAN_POINT ( 'NONE',  ( -626.9846540392142060, 95.00000000000000000, 34.99999999999999289 ) ) ;
#20326 = CARTESIAN_POINT ( 'NONE',  ( -129.2303573020127772, -9.309001178986628489, 25.82247248359045599 ) ) ;
#20327 = CARTESIAN_POINT ( 'NONE',  ( -56.48582580120559982, 50.09629031063956717, 6.472252184284792875 ) ) ;
#20328 = CARTESIAN_POINT ( 'NONE',  ( 170.0000000000000000, 24.95097643317003744, 0.000000000000000000 ) ) ;
#20330 = CARTESIAN_POINT ( 'NONE',  ( -213.1075012329537230, 37.98287015391211696, 18.58567234101190735 ) ) ;
#20329 = CARTESIAN_POINT ( 'NONE',  ( -189.1816166312696623, 17.96744819725043385, -43.37725711903431858 ) ) ;
#20331 = CARTESIAN_POINT ( 'NONE',  ( 136.1360204305621266, 35.03383547441298873, 0.000000000000000000 ) ) ;
#20332 = CARTESIAN_POINT ( 'NONE',  ( 130.8568914410475372, -5.949712681206667853, -2.449293598294708485E-15 ) ) ;
#20333 = CARTESIAN_POINT ( 'NONE',  ( -280.0000000000000568, 19.99999999999996447, -40.00000000000002132 ) ) ;
#20334 = CARTESIAN_POINT ( 'NONE',  ( -208.1127848780264742, -39.99999999999948841, -55.00245453010965235 ) ) ;
#20335 = CARTESIAN_POINT ( 'NONE',  ( -280.0000000000000000, 14.14213562373088351, 14.14213562373098654 ) ) ;
#20336 = CARTESIAN_POINT ( 'NONE',  ( -99.31364972220157483, 20.48028939131803128, -8.933506367388797997 ) ) ;
#20337 = CARTESIAN_POINT ( 'NONE',  ( 163.1118516004056573, 47.56205970284970164, -9.006482792073828847 ) ) ;
#20338 = ORIENTED_EDGE ( 'NONE', *, *, #10442, .F. ) ;
#20339 = CARTESIAN_POINT ( 'NONE',  ( -56.48582580120559982, -34.75652343174615311, 21.81201906317766870 ) ) ;
#20340 = CARTESIAN_POINT ( 'NONE',  ( -100.0957100001695608, 8.517115559328161112, 20.56213589534488406 ) ) ;
#20341 = SHAPE_DEFINITION_REPRESENTATION ( #20600, #23888 ) ;
#20342 = ORIENTED_EDGE ( 'NONE', *, *, #17291, .F. ) ;
#20343 = ORIENTED_EDGE ( 'NONE', *, *, #12467, .F. ) ;
#20344 = CARTESIAN_POINT ( 'NONE',  ( 136.1360204305621266, -3.511608612530379592, -53.05693388239318153 ) ) ;
#20345 = CARTESIAN_POINT ( 'NONE',  ( 67.90397382963038808, -30.27708616532465413, -10.29861769453878040 ) ) ;
#20346 = ORIENTED_EDGE ( 'NONE', *, *, #5308, .T. ) ;
#20347 = CARTESIAN_POINT ( 'NONE',  ( -192.9588430854689989, 14.46834944099965981, 0.000000000000000000 ) ) ;
#20348 = CARTESIAN_POINT ( 'NONE',  ( -99.21568817060988010, -16.03295912088706743, -16.03295912088710296 ) ) ;
#20349 = CIRCLE ( 'NONE', #13119, 5.000000000000004441 ) ;
#20350 = EDGE_CURVE ( 'NONE', #23307, #26265, #17875, .T. ) ;
#20351 = ORIENTED_EDGE ( 'NONE', *, *, #4311, .F. ) ;
#20352 = CARTESIAN_POINT ( 'NONE',  ( 199.9999999999999716, 16.82276630623001878, 8.840806072347076494 ) ) ;
#20353 = CARTESIAN_POINT ( 'NONE',  ( -190.0000000000000000, 52.50000000000007816, 52.49999999999999289 ) ) ;
#20354 = CARTESIAN_POINT ( 'NONE',  ( 4.995406935893283773, 39.06748935135195211, -17.50105314357185193 ) ) ;
#20355 = ADVANCED_FACE ( 'NONE', ( #21179 ), #15300, .F. ) ;
#20356 = CARTESIAN_POINT ( 'NONE',  ( -188.3611024622295815, -47.01268868735291306, -13.83140737835780953 ) ) ;
#20357 = CARTESIAN_POINT ( 'NONE',  ( 19.06497207195982924, -40.00000000000021316, 54.19242893257830218 ) ) ;
#20358 = CARTESIAN_POINT ( 'NONE',  ( -30.26275506840324425, 1.694272468446254232, 40.00000000000002132 ) ) ;
#20359 = CARTESIAN_POINT ( 'NONE',  ( 192.4448373802100889, 14.14213562370330379, -14.14213562370292365 ) ) ;
#20360 = CARTESIAN_POINT ( 'NONE',  ( 199.0235930299571123, -0.6679962965002699260, 20.00321896753086648 ) ) ;
#20361 = EDGE_CURVE ( 'NONE', #17033, #6362, #15546, .T. ) ;
#20362 = CARTESIAN_POINT ( 'NONE',  ( 199.9999999999999432, 1.065690307512836407E-13, -20.00000000000010303 ) ) ;
#20363 = CARTESIAN_POINT ( 'NONE',  ( -280.0000000000000568, -40.00000000000014211, 19.99999999999987210 ) ) ;
#20364 = CARTESIAN_POINT ( 'NONE',  ( -105.3755690713226727, 5.661656051307470077E-14, -21.75974354311649961 ) ) ;
#20365 = CARTESIAN_POINT ( 'NONE',  ( -91.56559293963836410, 22.67402823373189946, -0.000000000000000000 ) ) ;
#20366 = CARTESIAN_POINT ( 'NONE',  ( -192.9588430854690273, -10.23066800229550388, 66.79921049721887982 ) ) ;
#20367 = CARTESIAN_POINT ( 'NONE',  ( 200.0000000000000000, 20.00000000000013856, -40.00000000000002132 ) ) ;
#20368 = CARTESIAN_POINT ( 'NONE',  ( -280.0000000000000568, 14.14213562373067745, 42.42640687119295251 ) ) ;
#20369 = CARTESIAN_POINT ( 'NONE',  ( 150.0000000000000284, -125.7889608577475400, -82.49999999999998579 ) ) ;
#20370 = FACE_BOUND ( 'NONE', #11094, .T. ) ;
#20371 = CARTESIAN_POINT ( 'NONE',  ( -238.4067589809705794, -3.369206980223063916E-14, -0.9644942799825824142 ) ) ;
#20372 = CARTESIAN_POINT ( 'NONE',  ( -56.48582580120557850, -40.00000000000014211, 30.84685318188629921 ) ) ;
#20373 = CARTESIAN_POINT ( 'NONE',  ( 91.82158438592158234, 44.40256751092336884, -12.16597498400043342 ) ) ;
#20374 = CARTESIAN_POINT ( 'NONE',  ( 170.2234770963711128, 17.36149277826980253, 17.36149277827007253 ) ) ;
#20375 = CARTESIAN_POINT ( 'NONE',  ( -189.0540493709920611, -17.95404051684892011, -43.34488811517432794 ) ) ;
#20376 = CARTESIAN_POINT ( 'NONE',  ( 57.59792236341148453, -54.84617931850877426, -1.722363176415331099 ) ) ;
#20377 = ORIENTED_EDGE ( 'NONE', *, *, #18676, .T. ) ;
#20378 = AXIS2_PLACEMENT_3D ( 'NONE', #4252, #4510, #16733 ) ;
#20379 = CARTESIAN_POINT ( 'NONE',  ( 184.8905102610680444, -14.79361573936330565, -41.77492675556016621 ) ) ;
#20380 = CARTESIAN_POINT ( 'NONE',  ( -85.37145963729155085, 19.33814434286730588, 8.010121657944045737 ) ) ;
#20381 = CARTESIAN_POINT ( 'NONE',  ( -135.8532207217289738, 9.153146818113548022, -40.00000000000002132 ) ) ;
#20382 = SURFACE_SIDE_STYLE ('',( #18106 ) ) ;
#20383 = CARTESIAN_POINT ( 'NONE',  ( 0.2972598230769938343, 10.13633138497486286, -10.13633138497461594 ) ) ;
#20384 = B_SPLINE_CURVE_WITH_KNOTS ( 'NONE', 3,
 ( #26244, #7979, #1745, #24228, #4013, #20237, #1615, #2018, #6128, #22376, #8651, #16502 ),
 .UNSPECIFIED., .F., .F.,
 ( 4, 2, 2, 2, 2, 4 ),
 ( 1.597743418105305181E-15, 0.004698945756008282397, 0.007048418634011624322, 0.009397891512014965379, 0.01409683726802164923, 0.01879578302402833134 ),
 .UNSPECIFIED. ) ;
#20385 = ORIENTED_EDGE ( 'NONE', *, *, #13513, .F. ) ;
#20386 = EDGE_LOOP ( 'NONE', ( #5695, #17483, #9226, #15707 ) ) ;
#20387 = CARTESIAN_POINT ( 'NONE',  ( 199.9999999999999147, 11.56246421534694413, 15.09700933887624963 ) ) ;
#20388 = B_SPLINE_CURVE_WITH_KNOTS ( 'NONE', 3,
 ( #6952, #13088, #23699, #11581, #1236, #3104 ),
 .UNSPECIFIED., .F., .F.,
 ( 4, 2, 4 ),
 ( 0.0003134736701598289828, 0.004478999675054296317, 0.008644525679948764085 ),
 .UNSPECIFIED. ) ;
#20389 = CARTESIAN_POINT ( 'NONE',  ( -215.0000000000000284, 57.47694228411666728, -64.52066607436458412 ) ) ;
#20390 = CARTESIAN_POINT ( 'NONE',  ( -2.557884977177247610, 13.90734923101136111, 47.52441970261063631 ) ) ;
#20391 = EDGE_LOOP ( 'NONE', ( #1585, #11028, #7819, #25649 ) ) ;
#20392 = PRODUCT_RELATED_PRODUCT_CATEGORY ( 'part', '', ( #12748 ) ) ;
#20393 = ORIENTED_EDGE ( 'NONE', *, *, #18990, .T. ) ;
#20394 = CARTESIAN_POINT ( 'NONE',  ( 190.0000000000000000, 52.49999999999987210, -82.49999999999998579 ) ) ;
#20395 = CARTESIAN_POINT ( 'NONE',  ( 199.0104473268430922, -4.709499629590884417, -19.43548647772360383 ) ) ;
#20396 = CARTESIAN_POINT ( 'NONE',  ( -114.6380899717675987, -5.502349596714755542, -21.35059266670068467 ) ) ;
#20397 =( NAMED_UNIT ( * ) PLANE_ANGLE_UNIT ( ) SI_UNIT ( $, .RADIAN. ) );
#20398 = EDGE_CURVE ( 'NONE', #17794, #24064, #11552, .T. ) ;
#20399 = DIRECTION ( 'NONE',  ( 0.000000000000000000, -0.000000000000000000, 1.000000000000000000 ) ) ;
#20400 = AXIS2_PLACEMENT_3D ( 'NONE', #11265, #21264, #23134 ) ;
#20401 = CARTESIAN_POINT ( 'NONE',  ( -238.4067589809705794, 3.877349844572403567E-13, -40.96449427998260973 ) ) ;
#20402 = CARTESIAN_POINT ( 'NONE',  ( 199.9999999999999432, -13.87586802671829211, 12.99819774096606118 ) ) ;
#20403 = CARTESIAN_POINT ( 'NONE',  ( 169.9999999999999432, 6.285860131565304876, -24.25569233607180308 ) ) ;
#20404 = CARTESIAN_POINT ( 'NONE',  ( 23.37394308801977871, -42.85717664514601921, 23.33966569535066071 ) ) ;
#20405 = CARTESIAN_POINT ( 'NONE',  ( 199.0238195103507053, -1.318470765087343954, 19.97100952642404437 ) ) ;
#20406 = FACE_OUTER_BOUND ( 'NONE', #693, .T. ) ;
#20407 = CARTESIAN_POINT ( 'NONE',  ( -4.260882601031172889, -23.40615483283773557, -42.93997571557876114 ) ) ;
#20408 = CARTESIAN_POINT ( 'NONE',  ( -56.48582580120558561, -50.09629031063971638, 6.472252184283745713 ) ) ;
#20409 = CARTESIAN_POINT ( 'NONE',  ( -199.9999999999999432, 14.17215463606929227, 49.28189405767592746 ) ) ;
#20410 = CARTESIAN_POINT ( 'NONE',  ( 163.1118516004056573, -37.29075403953139300, -19.27778845539249630 ) ) ;
#20411 = CARTESIAN_POINT ( 'NONE',  ( 98.29820294270304259, -18.47759065022024672, 7.653668647299475047 ) ) ;
#20412 = CYLINDRICAL_SURFACE ( 'NONE', #24536, 6.000000000000019540 ) ;
#20413 = CARTESIAN_POINT ( 'NONE',  ( 163.1118516004056573, -12.73709011382472589, 40.00000000000002132 ) ) ;
#20414 = CARTESIAN_POINT ( 'NONE',  ( 170.0000000000428315, 17.64300463311351308, -17.64300463311329992 ) ) ;
#20415 = CARTESIAN_POINT ( 'NONE',  ( -198.0356074513804288, -55.37879056873077133, -2.449293598294708485E-15 ) ) ;
#20416 = CARTESIAN_POINT ( 'NONE',  ( -96.93773665438794751, 20.92028269119439443, -8.190703376740675168 ) ) ;
#20417 = CARTESIAN_POINT ( 'NONE',  ( -135.8532207217289738, 39.99999999999990763, 9.153146818113990335 ) ) ;
#20418 = CARTESIAN_POINT ( 'NONE',  ( 57.59792236341147031, 26.56190807104693619, -30.00663442387692115 ) ) ;
#20419 = CARTESIAN_POINT ( 'NONE',  ( 4.995406935893288214, 15.24977328854832770, -40.00000000000002132 ) ) ;
#20420 = EDGE_LOOP ( 'NONE', ( #21983, #9526, #12751, #15669 ) ) ;
#20421 = EDGE_LOOP ( 'NONE', ( #6235, #21590, #5070, #16712 ) ) ;
#20422 = CARTESIAN_POINT ( 'NONE',  ( 151.7948205124836250, -33.23291073765550863, 0.000000000000000000 ) ) ;
#20423 = CARTESIAN_POINT ( 'NONE',  ( -100.7734535825088358, 12.25131212657497848, -12.25131212657469604 ) ) ;
#20424 = CARTESIAN_POINT ( 'NONE',  ( 136.1360204305621266, -35.03383547441293899, 0.000000000000000000 ) ) ;
#20425 = CARTESIAN_POINT ( 'NONE',  ( 180.0000000000000000, -35.78896085774750446, -82.49999999999998579 ) ) ;
#20426 = CARTESIAN_POINT ( 'NONE',  ( -188.2995950289364373, 13.82811170417284075, -46.99046209955416487 ) ) ;
#20427 = CARTESIAN_POINT ( 'NONE',  ( 199.9999999999998863, 18.47321080301961160, -4.449129010553737551 ) ) ;
#20428 = CARTESIAN_POINT ( 'NONE',  ( 199.9999999999999716, -18.93198117488135779, -1.711693323776216191 ) ) ;
#20429 = CARTESIAN_POINT ( 'NONE',  ( -208.1127848780264742, 67.17687982763172272, -10.60833733270698254 ) ) ;
#20430 = CARTESIAN_POINT ( 'NONE',  ( 184.8905102610680444, -13.49065550809791603, -13.49065550809818781 ) ) ;
#20431 = LINE ( 'NONE', #20702, #5890 ) ;
#20432 = CARTESIAN_POINT ( 'NONE',  ( 0.2972598230769956662, 40.00000000000058975, -54.33493731733894094 ) ) ;
#20433 = CARTESIAN_POINT ( 'NONE',  ( 184.8905102610680444, -41.77492675556007384, 14.79361573936348684 ) ) ;
#20434 = B_SPLINE_CURVE_WITH_KNOTS ( 'NONE', 3,
 ( #23080, #24809, #9092, #8966, #24675, #14549, #12828, #4588, #4852, #23205, #592, #20948, #8564, #18947, #14676, #8699, #16810, #22679, #24948, #4453, #21210, #2982, #2726, #19076, #10560, #17075, #20815, #857, #11089, #6696, #728, #22941, #13092, #20680, #25209, #6957, #12548, #2449, #18673, #22812, #12685, #19205, #2587, #10831, #10702, #18812, #8832, #16941, #14946, #4986, #21076, #2861, #10968, #15074, #987, #15331, #21710, #21337, #9470, #1240, #1494, #3108, #19707, #11212, #25336, #23579, #5483, #19327, #7592, #11457, #9600, #15704 ),
 .UNSPECIFIED., .F., .F.,
 ( 4, 2, 2, 2, 2, 2, 2, 2, 2, 2, 2, 2, 2, 2, 2, 2, 2, 2, 2, 2, 2, 2, 2, 2, 2, 2, 2, 2, 2, 2, 2, 2, 2, 2, 2, 4 ),
 ( 0.000000000000000000, 0.007188645765836454600, 0.008985807207295486501, 0.01078296864875452274, 0.01437729153167258654, 0.01797161441459064340, 0.02156593729750870547, 0.02875458306334482614, 0.03234890594626276678, 0.03414606738772174577, 0.03594322882918072476, 0.04313187459501699461, 0.04672619747793507056, 0.05032052036085313956, 0.05391484324377122245, 0.05571200468523027083, 0.05750916612668933309, 0.06110348900960745067, 0.06290065045106651986, 0.06469781189252560294, 0.07188645765836203239, 0.07548078054128025405, 0.07907510342419847571, 0.08266942630711668349, 0.08446658774857578045, 0.08626374919003489128, 0.09345239495587108480, 0.09524955639733019563, 0.09704671783878932034, 0.1006410407217078057, 0.1042353636046263049, 0.1060325250460855406, 0.1078296864875447902, 0.1114240093704632756, 0.1132211708119225391, 0.1150183322533817887 ),
 .UNSPECIFIED. ) ;
#20435 = CARTESIAN_POINT ( 'NONE',  ( -317.0000000000000568, -4.467814962633844109E-14, 31.79780246617542616 ) ) ;
#20436 = CARTESIAN_POINT ( 'NONE',  ( -175.9235640290363563, -21.03681942415335726, -39.35891869721508840 ) ) ;
#20437 = CARTESIAN_POINT ( 'NONE',  ( -135.8532207217289738, -50.09629031063965243, -6.472252184284438492 ) ) ;
#20438 = CARTESIAN_POINT ( 'NONE',  ( 199.0159431193063710, 14.16346371809618709, 14.12086452993616525 ) ) ;
#20440 = CARTESIAN_POINT ( 'NONE',  ( 200.0000000000000000, -40.00000000000005684, 19.99999999999978328 ) ) ;
#20439 = CARTESIAN_POINT ( 'NONE',  ( -135.8532207217289738, -6.472252184283586729, -50.09629031063973770 ) ) ;
#20441 =( BOUNDED_SURFACE ( )  B_SPLINE_SURFACE ( 3, 3, ( 
 ( #19410, #26064, #21928, #3841, #21931, #11808, #15531, #7945, #19928, #9821, #5566, #23659, #11538, #25799, #7806, #22205, #26209, #24189, #3566, #11412, #17532, #5439, #7416, #17790, #13540, #9425, #1846, #21666, #3440, #9949 ),
 ( #16063, #9549, #18058, #25670, #11945, #3705, #5963, #24055, #11670, #14074, #13934, #19662, #5831, #19534, #13672, #1449, #19794, #1711, #1319, #17658, #21794, #1581, #15922, #15659, #7547, #17924, #25935, #5691, #26068, #23785 ),
 ( #20070, #22069, #9684, #7677, #15789, #23916, #13796, #24594, #10349, #22729, #6487, #18730, #12211, #12339, #14204, #18188, #14599, #16730, #1978, #8081, #514, #6616, #22602, #6350, #14469, #4507, #4378, #12469, #16200, #8619 ),
 ( #20596, #24861, #2372, #4113, #24731, #16598, #24333, #20467, #10084, #12608, #6097, #2242, #16470, #14338, #20737, #14733, #26339, #3980, #10484, #18459, #22338, #18598, #376, #237, #8480, #2506, #10617, #12077, #6226, #20199 ),
 ( #20333, #2110, #10219, #18326, #107, #8214, #22470, #16332, #24461, #4249, #8349, #19128, #17127, #11143, #15130, #2779, #6882, #7009, #910, #23132, #23260, #11018, #14866, #9023, #25390, #18866, #10891, #4904, #780, #12881 ),
 ( #7266, #2648, #8753, #647, #2910, #25001, #20864, #13267, #16869, #23387, #6754, #4642, #1038, #25258, #12744, #5161, #5036, #3161, #23000, #11263, #19003, #1169, #13143, #20997, #4777, #21262, #8886, #17380, #25132, #3034 ),
 ( #19382, #19258, #9138, #17254, #7142, #16997, #14997, #15258, #21389, #13014, #9272, #25519, #21135, #22865, #10755, #11383, #21635, #15629, #19637, #5410, #9397, #5799, #21896, #1817, #11781, #11639, #9657, #7777, #17891, #13511 ) ),
 .UNSPECIFIED., .T., .F., .F. ) 
 B_SPLINE_SURFACE_WITH_KNOTS ( ( 4, 3, 4 ),
 ( 4, 2, 2, 2, 2, 2, 2, 2, 2, 2, 2, 2, 2, 2, 4 ),
 ( 0.000000000000000000, 0.5000000000000000000, 1.000000000000000000 ),
 ( 0.000000000000000000, 0.1357259735107005372, 0.1651108541090157700, 0.1944957347073310028, 0.3598804999793158710, 0.3867117631979620773, 0.4135430264166082281, 0.5789277916885930964, 0.6062785021374117456, 0.6336292125862302838, 0.8508620842112317728, 0.8814014469398914198, 0.9119408096685510667, 0.9559704048342755334, 1.000000000000000000 ),
 .UNSPECIFIED. ) 
 GEOMETRIC_REPRESENTATION_ITEM ( )  RATIONAL_B_SPLINE_SURFACE ( (
 ( 1.000000000000000000, 1.000000000000000000, 1.000000000000000000, 1.000000000000000000, 1.000000000000000000, 1.000000000000000000, 1.000000000000000000, 1.000000000000000000, 1.000000000000000000, 1.000000000000000000, 1.000000000000000000, 1.000000000000000000, 1.000000000000000000, 1.000000000000000000, 1.000000000000000000, 1.000000000000000000, 1.000000000000000000, 1.000000000000000000, 1.000000000000000000, 1.000000000000000000, 1.000000000000000000, 1.000000000000000000, 1.000000000000000000, 1.000000000000000000, 1.000000000000000000, 1.000000000000000000, 1.000000000000000000, 1.000000000000000000, 1.000000000000000000, 1.000000000000000000),
 ( 0.3333333333333333703, 0.3333333333333333703, 0.3333333333333333703, 0.3333333333333333703, 0.3333333333333333703, 0.3333333333333333703, 0.3333333333333333703, 0.3333333333333333703, 0.3333333333333333703, 0.3333333333333333703, 0.3333333333333333703, 0.3333333333333333703, 0.3333333333333333703, 0.3333333333333333703, 0.3333333333333333703, 0.3333333333333333703, 0.3333333333333333703, 0.3333333333333333703, 0.3333333333333333703, 0.3333333333333333703, 0.3333333333333333703, 0.3333333333333333703, 0.3333333333333333703, 0.3333333333333333703, 0.3333333333333333703, 0.3333333333333333703, 0.3333333333333333703, 0.3333333333333333703, 0.3333333333333333703, 0.3333333333333333703),
 ( 0.3333333333333333703, 0.3333333333333333703, 0.3333333333333333703, 0.3333333333333333703, 0.3333333333333333703, 0.3333333333333333703, 0.3333333333333333703, 0.3333333333333333703, 0.3333333333333333703, 0.3333333333333333703, 0.3333333333333333703, 0.3333333333333333703, 0.3333333333333333703, 0.3333333333333333703, 0.3333333333333333703, 0.3333333333333333703, 0.3333333333333333703, 0.3333333333333333703, 0.3333333333333333703, 0.3333333333333333703, 0.3333333333333333703, 0.3333333333333333703, 0.3333333333333333703, 0.3333333333333333703, 0.3333333333333333703, 0.3333333333333333703, 0.3333333333333333703, 0.3333333333333333703, 0.3333333333333333703, 0.3333333333333333703),
 ( 1.000000000000000000, 1.000000000000000000, 1.000000000000000000, 1.000000000000000000, 1.000000000000000000, 1.000000000000000000, 1.000000000000000000, 1.000000000000000000, 1.000000000000000000, 1.000000000000000000, 1.000000000000000000, 1.000000000000000000, 1.000000000000000000, 1.000000000000000000, 1.000000000000000000, 1.000000000000000000, 1.000000000000000000, 1.000000000000000000, 1.000000000000000000, 1.000000000000000000, 1.000000000000000000, 1.000000000000000000, 1.000000000000000000, 1.000000000000000000, 1.000000000000000000, 1.000000000000000000, 1.000000000000000000, 1.000000000000000000, 1.000000000000000000, 1.000000000000000000),
 ( 0.3333333333333333703, 0.3333333333333333703, 0.3333333333333333703, 0.3333333333333333703, 0.3333333333333333703, 0.3333333333333333703, 0.3333333333333333703, 0.3333333333333333703, 0.3333333333333333703, 0.3333333333333333703, 0.3333333333333333703, 0.3333333333333333703, 0.3333333333333333703, 0.3333333333333333703, 0.3333333333333333703, 0.3333333333333333703, 0.3333333333333333703, 0.3333333333333333703, 0.3333333333333333703, 0.3333333333333333703, 0.3333333333333333703, 0.3333333333333333703, 0.3333333333333333703, 0.3333333333333333703, 0.3333333333333333703, 0.3333333333333333703, 0.3333333333333333703, 0.3333333333333333703, 0.3333333333333333703, 0.3333333333333333703),
 ( 0.3333333333333333703, 0.3333333333333333703, 0.3333333333333333703, 0.3333333333333333703, 0.3333333333333333703, 0.3333333333333333703, 0.3333333333333333703, 0.3333333333333333703, 0.3333333333333333703, 0.3333333333333333703, 0.3333333333333333703, 0.3333333333333333703, 0.3333333333333333703, 0.3333333333333333703, 0.3333333333333333703, 0.3333333333333333703, 0.3333333333333333703, 0.3333333333333333703, 0.3333333333333333703, 0.3333333333333333703, 0.3333333333333333703, 0.3333333333333333703, 0.3333333333333333703, 0.3333333333333333703, 0.3333333333333333703, 0.3333333333333333703, 0.3333333333333333703, 0.3333333333333333703, 0.3333333333333333703, 0.3333333333333333703),
 ( 1.000000000000000000, 1.000000000000000000, 1.000000000000000000, 1.000000000000000000, 1.000000000000000000, 1.000000000000000000, 1.000000000000000000, 1.000000000000000000, 1.000000000000000000, 1.000000000000000000, 1.000000000000000000, 1.000000000000000000, 1.000000000000000000, 1.000000000000000000, 1.000000000000000000, 1.000000000000000000, 1.000000000000000000, 1.000000000000000000, 1.000000000000000000, 1.000000000000000000, 1.000000000000000000, 1.000000000000000000, 1.000000000000000000, 1.000000000000000000, 1.000000000000000000, 1.000000000000000000, 1.000000000000000000, 1.000000000000000000, 1.000000000000000000, 1.000000000000000000) ) ) 
 REPRESENTATION_ITEM ( '' )  SURFACE ( )  );
#20442 = CARTESIAN_POINT ( 'NONE',  ( 163.1118516004056573, 9.006482792073693844, 47.56205970284970164 ) ) ;
#20443 = CARTESIAN_POINT ( 'NONE',  ( 16.10036699862805420, 48.79524671500497845, -14.09853761975148068 ) ) ;
#20444 = CARTESIAN_POINT ( 'NONE',  ( -198.0356074513804572, 15.37879056873066830, -40.00000000000002132 ) ) ;
#20445 = CARTESIAN_POINT ( 'NONE',  ( 57.59792236341147031, -1.722363176415032004, -1.722363176415048880 ) ) ;
#20446 = CARTESIAN_POINT ( 'NONE',  ( -4.112199523540587265, -46.96527782736856693, 13.82298295336165950 ) ) ;
#20447 = AXIS2_PLACEMENT_3D ( 'NONE', #18246, #6280, #13856 ) ;
#20448 = CARTESIAN_POINT ( 'NONE',  ( -86.96347745069644475, 18.24025645688351105, 2.449293598294708485E-15 ) ) ;
#20449 = VERTEX_POINT ( 'NONE', #17672 ) ;
#20450 = LINE ( 'NONE', #8464, #18582 ) ;
#20451 = VECTOR ( 'NONE', #21163, 1000.000000000000000 ) ;
#20452 = AXIS2_PLACEMENT_3D ( 'NONE', #5462, #23559, #11437 ) ;
#20453 = CARTESIAN_POINT ( 'NONE',  ( 57.59792236341147031, -30.00663442387700641, 26.56190807104681895 ) ) ;
#20454 = CARTESIAN_POINT ( 'NONE',  ( -4.810655158399423925, -17.78437748360810744, 42.93528531928082970 ) ) ;
#20455 = EDGE_CURVE ( 'NONE', #1338, #3113, #15672, .T. ) ;
#20456 = CARTESIAN_POINT ( 'NONE',  ( -3.488770945845315552, 17.93216134257417238, -43.29206711590411061 ) ) ;
#20457 = CARTESIAN_POINT ( 'NONE',  ( 199.0171635947087907, -15.67013318013508716, -12.42972081464992407 ) ) ;
#20458 = DIRECTION ( 'NONE',  ( 0.000000000000000000, 1.000000000000000000, 0.000000000000000000 ) ) ;
#20459 = CARTESIAN_POINT ( 'NONE',  ( -190.0000000000000000, 66.50000000000009948, 66.50000000000005684 ) ) ;
#20460 = CARTESIAN_POINT ( 'NONE',  ( -173.7925586247448564, -20.60916590994201059, 38.69493321926378826 ) ) ;
#20461 = CARTESIAN_POINT ( 'NONE',  ( 200.0000000000000000, -42.42640687119272513, -14.14213562373140753 ) ) ;
#20462 = CARTESIAN_POINT ( 'NONE',  ( -87.11144460433696679, -2.726859767319054662, 21.34775726304732402 ) ) ;
#20464 = CARTESIAN_POINT ( 'NONE',  ( -135.8532207217289738, 21.81201906317729566, 34.75652343174635917 ) ) ;
#20463 = CARTESIAN_POINT ( 'NONE',  ( -192.1964066538403983, 14.00508515770237850, -48.17614796926574172 ) ) ;
#20465 = CARTESIAN_POINT ( 'NONE',  ( -162.0762913951021176, 29.48230308784730980, 27.08623940707652622 ) ) ;
#20466 = CARTESIAN_POINT ( 'NONE',  ( 199.9999999999999432, -19.99999999999988987, -2.449293598294708485E-15 ) ) ;
#20467 = CARTESIAN_POINT ( 'NONE',  ( -162.0762913951020892, 41.69427287682832173, 2.449293598294708485E-15 ) ) ;
#20468 = CARTESIAN_POINT ( 'NONE',  ( -259.2033419157646676, -40.00000000000017053, 9.517827891722212996 ) ) ;
#20469 = CARTESIAN_POINT ( 'NONE',  ( 4.995406935893297096, 10.78321810387837232, 67.35176059880234334 ) ) ;
#20470 = CARTESIAN_POINT ( 'NONE',  ( -102.4309680866695658, 20.43798635339614123, -8.087567261645812522 ) ) ;
#20471 = APPLICATION_CONTEXT ( 'automotive_design' ) ;
#20472 = CARTESIAN_POINT ( 'NONE',  ( -238.4067589809705794, -28.96627169325303797, -28.96627169325349627 ) ) ;
#20473 = ORIENTED_EDGE ( 'NONE', *, *, #11099, .F. ) ;
#20474 = CARTESIAN_POINT ( 'NONE',  ( 192.4448373802100889, -14.14213562375876698, -14.14213562375885047 ) ) ;
#20475 = CARTESIAN_POINT ( 'NONE',  ( -103.9663809734228010, 8.574562933000146714, 19.92521373354193059 ) ) ;
#20476 = EDGE_LOOP ( 'NONE', ( #12423, #17933 ) ) ;
#20477 = CARTESIAN_POINT ( 'NONE',  ( 14.38125909742182529, -39.01709431150933938, 39.01709431150894147 ) ) ;
#20478 = CARTESIAN_POINT ( 'NONE',  ( -3.696864809820963771, -47.11278487914724877, -13.84627154338573440 ) ) ;
#20479 = ORIENTED_EDGE ( 'NONE', *, *, #4597, .T. ) ;
#20480 = CARTESIAN_POINT ( 'NONE',  ( 21.15358250000286944, -47.58740525741999505, -13.91686544622497479 ) ) ;
#20481 = FACE_OUTER_BOUND ( 'NONE', #12756, .T. ) ;
#20482 = ORIENTED_EDGE ( 'NONE', *, *, #11404, .F. ) ;
#20483 = CARTESIAN_POINT ( 'NONE',  ( 199.9999999999998863, 15.61930985130600291, 10.83040361559445230 ) ) ;
#20484 = CIRCLE ( 'NONE', #4772, 5.000000000000004441 ) ;
#20485 = CARTESIAN_POINT ( 'NONE',  ( 210.0000000000000284, 60.27431767988573341, -73.32453023895050137 ) ) ;
#20486 = CARTESIAN_POINT ( 'NONE',  ( 170.2234770963711128, 10.92277846919210660, -45.64576402573182889 ) ) ;
#20487 = CARTESIAN_POINT ( 'NONE',  ( -188.2957210513760913, -43.00408675155287597, -23.44847782072231368 ) ) ;
#20488 =( BOUNDED_SURFACE ( )  B_SPLINE_SURFACE ( 3, 2, ( 
 ( #21731, #15467, #23223 ),
 ( #11352, #21356, #11106 ),
 ( #5128, #9105, #13602 ),
 ( #15351, #17215, #25732 ),
 ( #25354, #1255, #3125 ),
 ( #1135, #7109, #7354 ),
 ( #9359, #5375, #15220 ),
 ( #13479, #11228, #25482 ),
 ( #21601, #3374, #11606 ),
 ( #5247, #11473, #13351 ),
 ( #19729, #19601, #1387 ),
 ( #9488, #17592, #7483 ),
 ( #1516, #9621, #1914 ),
 ( #20136, #21860, #12016 ),
 ( #23850, #14273, #8017 ),
 ( #20407, #3917, #5762 ),
 ( #14006, #15853, #19860 ),
 ( #13870, #7879, #3636 ),
 ( #10019, #18397, #22136 ),
 ( #14142, #11877, #7610 ),
 ( #26006, #18128, #26278 ),
 ( #22409, #22003, #22274 ),
 ( #13734, #4185, #16132 ),
 ( #1646, #24262, #6036 ),
 ( #12280, #15725, #3773 ),
 ( #19997, #5628, #24127 ),
 ( #4048, #9754, #12149 ),
 ( #1783, #11741, #5898 ),
 ( #17855, #7742, #9887 ),
 ( #20271, #2050, #26136 ),
 ( #10157, #23983, #17989 ),
 ( #16000, #2181, #18260 ),
 ( #41, #8154, #16268 ),
 ( #10289, #24397, #6163 ),
 ( #22538, #2805, #13289 ),
 ( #13165, #21158, #8912 ),
 ( #11289, #21410, #25413 ),
 ( #15280, #9167, #4668 ),
 ( #12770, #25284, #20897 ),
 ( #7040, #4805, #12907 ),
 ( #21022, #15156, #25025 ),
 ( #13040, #6908, #6290 ),
 ( #4929, #10780, #2675 ),
 ( #9045, #23283, #23410 ),
 ( #8280, #10916, #3059 ),
 ( #174, #14890, #11162 ),
 ( #16406, #17021, #24534 ),
 ( #18892, #17150, #17281 ),
 ( #14408, #25157, #671 ),
 ( #8780, #23030, #2932 ),
 ( #936, #19027, #19151 ),
 ( #5059, #21285, #3183 ),
 ( #19278, #6778, #16893 ),
 ( #806, #5187, #15025 ),
 ( #23155, #11041, #1061 ),
 ( #7164, #5302, #3311 ),
 ( #21927, #26063, #23911 ),
 ( #1192, #5687, #25931 ),
 ( #17653, #17402, #15406 ),
 ( #17786, #23531, #5560 ),
 ( #23655, #5435, #13929 ),
 ( #9545, #7543, #25795 ) ),
 .UNSPECIFIED., .F., .F., .F. ) 
 B_SPLINE_SURFACE_WITH_KNOTS ( ( 4, 2, 2, 2, 2, 2, 2, 2, 2, 2, 2, 2, 2, 2, 2, 2, 2, 2, 2, 2, 2, 2, 2, 2, 2, 2, 2, 2, 2, 2, 4 ),
 ( 3, 3 ),
 ( 0.005118828937694972631, 0.02956064127319301543, 0.05400245360869105476, 0.07844426594418910104, 0.08149949248612635422, 0.08302710575709498775, 0.08379091239257929757, 0.08417281571032145249, 0.08436376736919252994, 0.08445924319862807561, 0.08450698111334584151, 0.08455471902806360740, 0.09066517211193811376, 0.09677562519581262013, 0.09983085173774988719, 0.1028860782796871404, 0.1089965313635616606, 0.1151069844474361670, 0.1181622109893734202, 0.1196898242603420537, 0.1204536308958263635, 0.1208355342135685184, 0.1208594031709274014, 0.1208832721282862843, 0.1209310100430040502, 0.1210264858724395959, 0.1212174375313106733, 0.1273278906151851797, 0.1517697029506832329, 0.1762115152861812861, 0.2006533276216793116 ),
 ( 0.000000000000000000, 1.000000000000000000 ),
 .UNSPECIFIED. ) 
 GEOMETRIC_REPRESENTATION_ITEM ( )  RATIONAL_B_SPLINE_SURFACE ( (
 ( 1.000000000000000000, 0.9997813423572989855, 1.000000000000000000),
 ( 1.000000000000000000, 0.9990919206318849000, 1.000000000000000000),
 ( 1.000000000000000000, 0.9967874177841468120, 1.000000000000000000),
 ( 1.000000000000000000, 0.9887544623280423162, 1.000000000000000000),
 ( 1.000000000000000000, 0.9830290792194826821, 1.000000000000000000),
 ( 1.000000000000000000, 0.9678345454226084943, 1.000000000000000000),
 ( 1.000000000000000000, 0.9583650305405041481, 1.000000000000000000),
 ( 1.000000000000000000, 0.9453335293271442064, 1.000000000000000000),
 ( 1.000000000000000000, 0.9438523872746331644, 1.000000000000000000),
 ( 1.000000000000000000, 0.9415799504611004345, 1.000000000000000000),
 ( 1.000000000000000000, 0.9408140170423924253, 1.000000000000000000),
 ( 1.000000000000000000, 0.9396523143999068184, 1.000000000000000000),
 ( 1.000000000000000000, 0.9392629463989446981, 1.000000000000000000),
 ( 1.000000000000000000, 0.9386756783046028563, 1.000000000000000000),
 ( 1.000000000000000000, 0.9384793862554876576, 1.000000000000000000),
 ( 1.000000000000000000, 0.9381841422086912852, 1.000000000000000000),
 ( 1.000000000000000000, 0.9380855931974644291, 1.000000000000000000),
 ( 1.000000000000000000, 0.9379375679425655532, 1.000000000000000000),
 ( 1.000000000000000000, 0.9378881925679135589, 1.000000000000000000),
 ( 1.000000000000000000, 0.9378140790407650806, 1.000000000000000000),
 ( 1.000000000000000000, 0.9377896949153100570, 1.000000000000000000),
 ( 1.000000000000000000, 0.9377409313168981742, 1.000000000000000000),
 ( 1.000000000000000000, 0.9377165729686738338, 1.000000000000000000),
 ( 1.000000000000000000, 0.9345773786263239513, 1.000000000000000000),
 ( 1.000000000000000000, 0.9318492984271956603, 1.000000000000000000),
 ( 1.000000000000000000, 0.9273872927432106339, 1.000000000000000000),
 ( 1.000000000000000000, 0.9256532593469934955, 1.000000000000000000),
 ( 1.000000000000000000, 0.9239357372751176856, 1.000000000000000000),
 ( 1.000000000000000000, 0.9235102113428155235, 1.000000000000000000),
 ( 1.000000000000000000, 0.9229728558028649221, 1.000000000000000000),
 ( 1.000000000000000000, 0.9228633126626060168, 1.000000000000000000),
 ( 1.000000000000000000, 0.9230139704737757578, 1.000000000000000000),
 ( 1.000000000000000000, 0.9237531682200380567, 1.000000000000000000),
 ( 1.000000000000000000, 0.9264156051934421265, 1.000000000000000000),
 ( 1.000000000000000000, 0.9283388455997357847, 1.000000000000000000),
 ( 1.000000000000000000, 0.9320050037532509046, 1.000000000000000000),
 ( 1.000000000000000000, 0.9333574575349512514, 1.000000000000000000),
 ( 1.000000000000000000, 0.9355411998008567043, 1.000000000000000000),
 ( 1.000000000000000000, 0.9362956009275962277, 1.000000000000000000),
 ( 1.000000000000000000, 0.9374637148016307098, 1.000000000000000000),
 ( 1.000000000000000000, 0.9378591705544923052, 1.000000000000000000),
 ( 1.000000000000000000, 0.9384610703419788980, 1.000000000000000000),
 ( 1.000000000000000000, 0.9386631562400657991, 1.000000000000000000),
 ( 1.000000000000000000, 0.9388793792114339398, 1.000000000000000000),
 ( 1.000000000000000000, 0.9388921037490453037, 1.000000000000000000),
 ( 1.000000000000000000, 0.9389175638858661133, 1.000000000000000000),
 ( 1.000000000000000000, 0.9389305010154688214, 1.000000000000000000),
 ( 1.000000000000000000, 0.9389691441648042591, 1.000000000000000000),
 ( 1.000000000000000000, 0.9389948969011616686, 1.000000000000000000),
 ( 1.000000000000000000, 0.9390721270299958734, 1.000000000000000000),
 ( 1.000000000000000000, 0.9391235763422339788, 1.000000000000000000),
 ( 1.000000000000000000, 0.9392778120326576996, 1.000000000000000000),
 ( 1.000000000000000000, 0.9393804861645823623, 1.000000000000000000),
 ( 1.000000000000000000, 0.9427638002345609669, 1.000000000000000000),
 ( 1.000000000000000000, 0.9458915987233159628, 1.000000000000000000),
 ( 1.000000000000000000, 0.9607963039206450784, 1.000000000000000000),
 ( 1.000000000000000000, 0.9703812854709533697, 1.000000000000000000),
 ( 1.000000000000000000, 0.9854660764533723638, 1.000000000000000000),
 ( 1.000000000000000000, 0.9909632567906727640, 1.000000000000000000),
 ( 1.000000000000000000, 0.9982308762622302822, 1.000000000000000000),
 ( 1.000000000000000000, 0.9999976772054812724, 1.000000000000000000),
 ( 1.000000000000000000, 1.000000000000000000, 1.000000000000000000) ) ) 
 REPRESENTATION_ITEM ( '' )  SURFACE ( )  );
#20489 = CARTESIAN_POINT ( 'NONE',  ( 146.6084372240433709, -40.00000000000001421, 5.374981219216829587 ) ) ;
#20490 = CARTESIAN_POINT ( 'NONE',  ( -192.9588430854690273, 54.46834944101718889, 40.00000000000002132 ) ) ;
#20491 = CARTESIAN_POINT ( 'NONE',  ( -280.0000000000000000, -14.14213562373118549, 14.14213562373078936 ) ) ;
#20492 = CARTESIAN_POINT ( 'NONE',  ( 199.0260264921024316, -10.00558763687667962, 17.32375098348098419 ) ) ;
#20493 = CARTESIAN_POINT ( 'NONE',  ( -213.1075012329537230, -40.00000000000025580, 53.71589010953650956 ) ) ;
#20494 = CARTESIAN_POINT ( 'NONE',  ( 151.7948205124836534, -40.00000000000001421, 6.767089262348889633 ) ) ;
#20495 = CARTESIAN_POINT ( 'NONE',  ( -30.26275506840324070, -1.147469862568086380E-14, 1.694272468446259783 ) ) ;
#20496 = CARTESIAN_POINT ( 'NONE',  ( -100.7734535825088500, 22.67402823373189591, -0.000000000000000000 ) ) ;
#20497 = CARTESIAN_POINT ( 'NONE',  ( 91.82158438592159655, -16.11829626346147393, 16.11829626346132116 ) ) ;
#20498 = CARTESIAN_POINT ( 'NONE',  ( 146.6084372240433709, -5.374981219216942385, -40.00000000000002132 ) ) ;
#20499 = CARTESIAN_POINT ( 'NONE',  ( 151.7948205124836250, -4.785054706301671068, 4.785054706301645311 ) ) ;
#20500 = CARTESIAN_POINT ( 'NONE',  ( 156.5537079553355966, -11.28159757857204326, -27.23618587942440783 ) ) ;
#20501 = DIRECTION ( 'NONE',  ( 0.000000000000000000, -1.000000000000000000, 0.000000000000000000 ) ) ;
#20502 = CARTESIAN_POINT ( 'NONE',  ( 57.59792236341147742, 4.064940816252731242E-13, -37.56421063658186199 ) ) ;
#20503 = CARTESIAN_POINT ( 'NONE',  ( 136.1360204305621266, 5.219216885335291329E-15, 4.966164525587064560 ) ) ;
#20504 = CARTESIAN_POINT ( 'NONE',  ( 4.995406935893290878, 39.06748935135185263, 39.06748935135198764 ) ) ;
#20505 = DIRECTION ( 'NONE',  ( 1.303213150798907793E-16, -1.000000000000000000, 2.775557561562890858E-16 ) ) ;
#20506 = CARTESIAN_POINT ( 'NONE',  ( -192.9588430854689989, 10.23066800230756712, -10.23066800230735396 ) ) ;
#20507 = CARTESIAN_POINT ( 'NONE',  ( -86.96347745069643054, -41.18208027870589660, -15.38646221621809040 ) ) ;
#20508 = ORIENTED_EDGE ( 'NONE', *, *, #19169, .F. ) ;
#20509 = CARTESIAN_POINT ( 'NONE',  ( 163.1118516004056573, -47.56205970284945295, -9.006482792074823607 ) ) ;
#20510 = CARTESIAN_POINT ( 'NONE',  ( 132.4338126186517002, 29.78211700502426496, -12.33615677966331248 ) ) ;
#20511 = CARTESIAN_POINT ( 'NONE',  ( -198.0356074513804288, -55.37879056873077133, -2.449293598294708485E-15 ) ) ;
#20512 = CARTESIAN_POINT ( 'NONE',  ( 170.0000000000000000, -2.301191124287261779E-13, 24.95097643317000546 ) ) ;
#20513 = LINE ( 'NONE', #16910, #24025 ) ;
#20514 = VERTEX_POINT ( 'NONE', #13186 ) ;
#20515 = ORIENTED_EDGE ( 'NONE', *, *, #22985, .F. ) ;
#20516 = CARTESIAN_POINT ( 'NONE',  ( 199.9999999999999716, 17.24217208250532352, 8.000691389023806721 ) ) ;
#20517 = CARTESIAN_POINT ( 'NONE',  ( 104.1600437297061745, 8.548029201969624680, -20.63676802892751994 ) ) ;
#20518 = CARTESIAN_POINT ( 'NONE',  ( 23.35901252181126964, 13.80180065670255907, 46.81387818480148866 ) ) ;
#20519 = ORIENTED_EDGE ( 'NONE', *, *, #15144, .F. ) ;
#20520 = ORIENTED_EDGE ( 'NONE', *, *, #6382, .T. ) ;
#20521 = DIRECTION ( 'NONE',  ( 1.000000000000000000, 1.836970198721030427E-16, -0.000000000000000000 ) ) ;
#20522 = CARTESIAN_POINT ( 'NONE',  ( 199.0139917666041924, -11.25641580849352685, -16.53121693397544689 ) ) ;
#20523 = CARTESIAN_POINT ( 'NONE',  ( -110.0961829990539655, -2.516385845105195251, -20.07657727077722853 ) ) ;
#20524 = CARTESIAN_POINT ( 'NONE',  ( 19.06497207195980792, 10.03556273973433299, 10.03556273973436319 ) ) ;
#20525 = CARTESIAN_POINT ( 'NONE',  ( 199.9999999999999432, 14.14213562373090838, 14.14213562373092437 ) ) ;
#20526 = CARTESIAN_POINT ( 'NONE',  ( -200.0000000000000284, -17.27712336974170881, 46.88040655664276102 ) ) ;
#20527 = CARTESIAN_POINT ( 'NONE',  ( -94.58360650938202241, -9.000712009885686982, -20.58386743642789440 ) ) ;
#20528 = CARTESIAN_POINT ( 'NONE',  ( 91.82158438592156813, 40.00000000000027711, -22.79471317813428044 ) ) ;
#20529 = CARTESIAN_POINT ( 'NONE',  ( 151.7948205124836250, -3.202120068677277203E-13, 33.23291073765553705 ) ) ;
#20530 = CARTESIAN_POINT ( 'NONE',  ( 190.0000000000000000, -71.50000000000002842, -66.50000000000005684 ) ) ;
#20531 = CARTESIAN_POINT ( 'NONE',  ( 190.0000000000000284, -125.7889608577475684, -82.49999999999998579 ) ) ;
#20532 = CARTESIAN_POINT ( 'NONE',  ( 199.0168302869249999, 12.92424399662411005, 15.26720349029574564 ) ) ;
#20533 = CARTESIAN_POINT ( 'NONE',  ( -190.7345856381493263, 23.92884448222178406, 43.65254615102011115 ) ) ;
#20534 = CARTESIAN_POINT ( 'NONE',  ( 146.6084372240433993, 24.48358557860307272, 24.48358557860347418 ) ) ;
#20535 = ADVANCED_FACE ( 'NONE', ( #3083 ), #23218, .T. ) ;
#20536 = FACE_OUTER_BOUND ( 'NONE', #8394, .T. ) ;
#20537 = CARTESIAN_POINT ( 'NONE',  ( 0.2972598230769923355, 18.14793986248697166, 38.42060263243675422 ) ) ;
#20538 = DIRECTION ( 'NONE',  ( 0.000000000000000000, -1.000000000000000000, 0.000000000000000000 ) ) ;
#20539 = CARTESIAN_POINT ( 'NONE',  ( 170.2234770963711128, 45.64576402573196390, -10.92277846919159856 ) ) ;
#20540 = CARTESIAN_POINT ( 'NONE',  ( -659.3259227587273017, 42.96433640846947100, 13.39333494796945878 ) ) ;
#20541 = CARTESIAN_POINT ( 'NONE',  ( -259.2033419157646676, 9.517827891722584255, -0.000000000000000000 ) ) ;
#20542 = EDGE_CURVE ( 'NONE', #18174, #13223, #14399, .T. ) ;
#20543 = B_SPLINE_CURVE_WITH_KNOTS ( 'NONE', 3,
 ( #9757, #19863, #3250, #5630, #11354, #19731, #13736, #11475 ),
 .UNSPECIFIED., .F., .F.,
 ( 4, 2, 2, 4 ),
 ( 0.000000000000000000, 0.002089226651538985107, 0.004178453303077970214, 0.008356906606155938694 ),
 .UNSPECIFIED. ) ;
#20544 = CARTESIAN_POINT ( 'NONE',  ( 116.7964245048381713, 19.78678521258536449, -19.78678521258513356 ) ) ;
#20545 = CARTESIAN_POINT ( 'NONE',  ( -213.1075012329537230, -13.71589010951915810, 40.00000000000002132 ) ) ;
#20546 = CARTESIAN_POINT ( 'NONE',  ( -114.7810454938858982, 16.28728334995616933, 14.99889064788714066 ) ) ;
#20547 = CARTESIAN_POINT ( 'NONE',  ( 136.1360204305621551, 39.99999999999968026, 35.03383547441337953 ) ) ;
#20548 = ADVANCED_FACE ( 'NONE', ( #25528 ), #7277, .T. ) ;
#20549 = CARTESIAN_POINT ( 'NONE',  ( -100.7734535825088500, 12.25131212657490209, -44.31723036834897300 ) ) ;
#20550 = EDGE_CURVE ( 'NONE', #15800, #16510, #4913, .T. ) ;
#20551 = CARTESIAN_POINT ( 'NONE',  ( 127.8236149080042026, -11.91256696755882771, 28.75948073575737141 ) ) ;
#20552 = ORIENTED_EDGE ( 'NONE', *, *, #5121, .T. ) ;
#20553 = ORIENTED_EDGE ( 'NONE', *, *, #2831, .F. ) ;
#20554 = CARTESIAN_POINT ( 'NONE',  ( -198.0356074513804572, 15.37879056873067007, 0.000000000000000000 ) ) ;
#20555 = DIRECTION ( 'NONE',  ( -1.836970198721030181E-16, 1.000000000000000000, 0.000000000000000000 ) ) ;
#20556 = CARTESIAN_POINT ( 'NONE',  ( -135.8532207217289738, 21.81201906317798134, -21.81201906317747685 ) ) ;
#20557 = CARTESIAN_POINT ( 'NONE',  ( -114.4364955367318970, -20.29001642038926789, -8.064892380839017605 ) ) ;
#20558 = CARTESIAN_POINT ( 'NONE',  ( -138.9613193423055861, -10.11110876497707523, -29.42718875716579774 ) ) ;
#20559 = CARTESIAN_POINT ( 'NONE',  ( -138.9613198122422375, 13.65853124629189352, 27.95779845120234697 ) ) ;
#20560 = CARTESIAN_POINT ( 'NONE',  ( 199.9999999999998579, 15.71915069317562264, -10.67410001769982308 ) ) ;
#20561 = CARTESIAN_POINT ( 'NONE',  ( 199.9999999999999147, 10.80962424009062239, -15.62854876372556490 ) ) ;
#20562 = CARTESIAN_POINT ( 'NONE',  ( 151.7948205124836534, -51.78348778862529400, -4.785054706299085581 ) ) ;
#20563 = CARTESIAN_POINT ( 'NONE',  ( 4.995406935893297984, -39.06748935135205869, 17.50105314357158193 ) ) ;
#20564 = CARTESIAN_POINT ( 'NONE',  ( -110.0513613218576410, 19.08113875878609988, 6.582668557813116550 ) ) ;
#20565 = CARTESIAN_POINT ( 'NONE',  ( 130.8568914410475088, 40.00000000000011369, -5.949712681206269949 ) ) ;
#20566 = CARTESIAN_POINT ( 'NONE',  ( 14.38125909742183062, -67.30136555895943218, -10.73282306403629605 ) ) ;
#20567 = CARTESIAN_POINT ( 'NONE',  ( 91.82158438592158234, 17.20528682183301683, 0.000000000000000000 ) ) ;
#20568 = CARTESIAN_POINT ( 'NONE',  ( -100.7734535825088358, -16.03295912088706743, -16.03295912088710296 ) ) ;
#20569 = CARTESIAN_POINT ( 'NONE',  ( -259.2033419157646676, -21.55415060305824326, -35.01439189186556433 ) ) ;
#20570 = CARTESIAN_POINT ( 'NONE',  ( 199.0157676419877646, 14.39733183096338998, 13.88287279058362067 ) ) ;
#20571 = VECTOR ( 'NONE', #18874, 1000.000000000000000 ) ;
#20573 = CARTESIAN_POINT ( 'NONE',  ( 163.1118516004056573, 40.00000000000000711, 12.73709011382489642 ) ) ;
#20572 = CARTESIAN_POINT ( 'NONE',  ( -105.3755690713226585, -15.38646221621738164, -41.18208027870615240 ) ) ;
#20574 = CARTESIAN_POINT ( 'NONE',  ( -208.1127848780264742, 38.89260858015707356, 17.67593391476696141 ) ) ;
#20575 = CARTESIAN_POINT ( 'NONE',  ( 23.40652632867980643, 46.79646383233858131, -13.79856377312498417 ) ) ;
#20576 = CARTESIAN_POINT ( 'NONE',  ( -30.26275506840324070, 41.69427246844628598, 2.449293598294708485E-15 ) ) ;
#20577 = CARTESIAN_POINT ( 'NONE',  ( 200.0000000000000000, 71.50000000000009948, -66.50000000000005684 ) ) ;
#20578 = CARTESIAN_POINT ( 'NONE',  ( -4.004886986945003891, -43.01537795656786045, 23.45685150724386148 ) ) ;
#20579 = CARTESIAN_POINT ( 'NONE',  ( 19.06497207195980792, 54.19242893257843718, 2.449293598294708485E-15 ) ) ;
#20580 = EDGE_LOOP ( 'NONE', ( #19671, #25307, #6177, #3758 ) ) ;
#20581 = CARTESIAN_POINT ( 'NONE',  ( -199.9999999999999432, 39.01096890182041221, 39.01096890182058985 ) ) ;
#20582 = CARTESIAN_POINT ( 'NONE',  ( -238.4067589809705794, -27.60227080167069147, 28.96627169325319429 ) ) ;
#20583 = CARTESIAN_POINT ( 'NONE',  ( -4.121597284766306046, -23.43330939486645903, 42.98102224344803801 ) ) ;
#20584 = CARTESIAN_POINT ( 'NONE',  ( -3.564770973659279640, 17.92368662243745092, -43.27160733161120021 ) ) ;
#20585 = CARTESIAN_POINT ( 'NONE',  ( 199.0083412756643497, 0.3136196654984919618, -19.99640146592421175 ) ) ;
#20586 = CARTESIAN_POINT ( 'NONE',  ( -28.75791583366071791, -38.33181286256370157, -12.03523584680476866 ) ) ;
#20587 = FACE_BOUND ( 'NONE', #20476, .T. ) ;
#20588 = CARTESIAN_POINT ( 'NONE',  ( -195.1685814578364386, -14.09692187700269095, 48.78510996053616822 ) ) ;
#20589 = CARTESIAN_POINT ( 'NONE',  ( -91.56559293963834989, -44.31723036834885932, -12.25131212657538171 ) ) ;
#20590 = CARTESIAN_POINT ( 'NONE',  ( -105.2054292635175585, -21.49321519473986442, -7.030298963786045751E-29 ) ) ;
#20591 =( BOUNDED_SURFACE ( )  B_SPLINE_SURFACE ( 3, 3, ( 
 ( #2532, #22629, #12108, #6644, #20233, #4404, #4148, #12241, #12368, #8242, #20496, #20365, #12498, #18759, #10511, #10250, #3, #541, #10377, #2012, #4538, #18488, #8377, #16499, #24624, #14368, #8511, #8646, #18217, #22234 ),
 ( #18625, #16628, #12635, #24360, #4278, #16755, #24759, #6124, #22499, #14623, #20762, #14232, #24889, #18359, #138, #24494, #15024, #2931, #8911, #14758, #6907, #9044, #11161, #935, #19150, #17149, #7163, #17280, #4804, #4928 ),
 ( #805, #9296, #21157, #17401, #13288, #17020, #14889, #23154, #7039, #11288, #25540, #25156, #13039, #19277, #25283, #21021, #21409, #11040, #15155, #5058, #2804, #23409, #10915, #23282, #18891, #19408, #22888, #13164, #4667, #21284 ),
 ( #3058, #1060, #3182, #23029, #9166, #25024, #2674, #25412, #1191, #12769, #15279, #5186, #20896, #10779, #670, #8779, #16892, #6777, #12906, #19026, #3836, #7670, #5686, #1444, #19528, #7411, #25665, #7291, #23910, #1312 ),
 ( #3561, #11665, #5558, #19789, #17652, #19923, #22064, #3310, #15405, #1576, #5826, #20065, #23530, #1706, #11406, #13666, #1841, #9420, #13928, #9544, #11938, #9943, #21789, #5301, #17527, #9814, #25930, #17919, #18051, #13411 ),
 ( #26062, #15655, #9679, #25794, #7542, #21535, #13790, #23779, #17785, #15783, #15525, #21926, #23654, #5434, #13535, #3698, #21660, #3432, #11803, #19657, #7800, #11533, #15915, #24049, #18454, #6092, #3975, #22723, #16327, #16058 ),
 ( #22200, #12463, #12072, #20191, #6220, #1973, #24184, #16593, #10079, #371, #230, #4244, #8475, #18184, #8209, #6482, #12334, #26334, #8075, #14594, #22331, #4500, #10344, #24328, #16194, #16465, #2236, #24589, #24455, #8344 ) ),
 .UNSPECIFIED., .T., .F., .F. ) 
 B_SPLINE_SURFACE_WITH_KNOTS ( ( 4, 3, 4 ),
 ( 4, 2, 2, 2, 2, 2, 2, 2, 2, 2, 2, 2, 2, 2, 4 ),
 ( 0.000000000000000000, 0.5000000000000000000, 1.000000000000000000 ),
 ( 0.000000000000000000, 0.1357259735107005372, 0.1651108541090157700, 0.1944957347073310028, 0.3598804999793158710, 0.3867117631979620773, 0.4135430264166082281, 0.5789277916885930964, 0.6062785021374117456, 0.6336292125862302838, 0.8508620842112317728, 0.8814014469398914198, 0.9119408096685510667, 0.9559704048342755334, 1.000000000000000000 ),
 .UNSPECIFIED. ) 
 GEOMETRIC_REPRESENTATION_ITEM ( )  RATIONAL_B_SPLINE_SURFACE ( (
 ( 1.000000000000000000, 1.000000000000000000, 1.000000000000000000, 1.000000000000000000, 1.000000000000000000, 1.000000000000000000, 1.000000000000000000, 1.000000000000000000, 1.000000000000000000, 1.000000000000000000, 1.000000000000000000, 1.000000000000000000, 1.000000000000000000, 1.000000000000000000, 1.000000000000000000, 1.000000000000000000, 1.000000000000000000, 1.000000000000000000, 1.000000000000000000, 1.000000000000000000, 1.000000000000000000, 1.000000000000000000, 1.000000000000000000, 1.000000000000000000, 1.000000000000000000, 1.000000000000000000, 1.000000000000000000, 1.000000000000000000, 1.000000000000000000, 1.000000000000000000),
 ( 0.3333333333333333703, 0.3333333333333333703, 0.3333333333333333703, 0.3333333333333333703, 0.3333333333333333703, 0.3333333333333333703, 0.3333333333333333703, 0.3333333333333333703, 0.3333333333333333703, 0.3333333333333333703, 0.3333333333333333703, 0.3333333333333333703, 0.3333333333333333703, 0.3333333333333333703, 0.3333333333333333703, 0.3333333333333333703, 0.3333333333333333703, 0.3333333333333333703, 0.3333333333333333703, 0.3333333333333333703, 0.3333333333333333703, 0.3333333333333333703, 0.3333333333333333703, 0.3333333333333333703, 0.3333333333333333703, 0.3333333333333333703, 0.3333333333333333703, 0.3333333333333333703, 0.3333333333333333703, 0.3333333333333333703),
 ( 0.3333333333333333703, 0.3333333333333333703, 0.3333333333333333703, 0.3333333333333333703, 0.3333333333333333703, 0.3333333333333333703, 0.3333333333333333703, 0.3333333333333333703, 0.3333333333333333703, 0.3333333333333333703, 0.3333333333333333703, 0.3333333333333333703, 0.3333333333333333703, 0.3333333333333333703, 0.3333333333333333703, 0.3333333333333333703, 0.3333333333333333703, 0.3333333333333333703, 0.3333333333333333703, 0.3333333333333333703, 0.3333333333333333703, 0.3333333333333333703, 0.3333333333333333703, 0.3333333333333333703, 0.3333333333333333703, 0.3333333333333333703, 0.3333333333333333703, 0.3333333333333333703, 0.3333333333333333703, 0.3333333333333333703),
 ( 1.000000000000000000, 1.000000000000000000, 1.000000000000000000, 1.000000000000000000, 1.000000000000000000, 1.000000000000000000, 1.000000000000000000, 1.000000000000000000, 1.000000000000000000, 1.000000000000000000, 1.000000000000000000, 1.000000000000000000, 1.000000000000000000, 1.000000000000000000, 1.000000000000000000, 1.000000000000000000, 1.000000000000000000, 1.000000000000000000, 1.000000000000000000, 1.000000000000000000, 1.000000000000000000, 1.000000000000000000, 1.000000000000000000, 1.000000000000000000, 1.000000000000000000, 1.000000000000000000, 1.000000000000000000, 1.000000000000000000, 1.000000000000000000, 1.000000000000000000),
 ( 0.3333333333333333703, 0.3333333333333333703, 0.3333333333333333703, 0.3333333333333333703, 0.3333333333333333703, 0.3333333333333333703, 0.3333333333333333703, 0.3333333333333333703, 0.3333333333333333703, 0.3333333333333333703, 0.3333333333333333703, 0.3333333333333333703, 0.3333333333333333703, 0.3333333333333333703, 0.3333333333333333703, 0.3333333333333333703, 0.3333333333333333703, 0.3333333333333333703, 0.3333333333333333703, 0.3333333333333333703, 0.3333333333333333703, 0.3333333333333333703, 0.3333333333333333703, 0.3333333333333333703, 0.3333333333333333703, 0.3333333333333333703, 0.3333333333333333703, 0.3333333333333333703, 0.3333333333333333703, 0.3333333333333333703),
 ( 0.3333333333333333703, 0.3333333333333333703, 0.3333333333333333703, 0.3333333333333333703, 0.3333333333333333703, 0.3333333333333333703, 0.3333333333333333703, 0.3333333333333333703, 0.3333333333333333703, 0.3333333333333333703, 0.3333333333333333703, 0.3333333333333333703, 0.3333333333333333703, 0.3333333333333333703, 0.3333333333333333703, 0.3333333333333333703, 0.3333333333333333703, 0.3333333333333333703, 0.3333333333333333703, 0.3333333333333333703, 0.3333333333333333703, 0.3333333333333333703, 0.3333333333333333703, 0.3333333333333333703, 0.3333333333333333703, 0.3333333333333333703, 0.3333333333333333703, 0.3333333333333333703, 0.3333333333333333703, 0.3333333333333333703),
 ( 1.000000000000000000, 1.000000000000000000, 1.000000000000000000, 1.000000000000000000, 1.000000000000000000, 1.000000000000000000, 1.000000000000000000, 1.000000000000000000, 1.000000000000000000, 1.000000000000000000, 1.000000000000000000, 1.000000000000000000, 1.000000000000000000, 1.000000000000000000, 1.000000000000000000, 1.000000000000000000, 1.000000000000000000, 1.000000000000000000, 1.000000000000000000, 1.000000000000000000, 1.000000000000000000, 1.000000000000000000, 1.000000000000000000, 1.000000000000000000, 1.000000000000000000, 1.000000000000000000, 1.000000000000000000, 1.000000000000000000, 1.000000000000000000, 1.000000000000000000) ) ) 
 REPRESENTATION_ITEM ( '' )  SURFACE ( )  );
#20593 = CARTESIAN_POINT ( 'NONE',  ( 163.1118516004056573, -19.27778845538787422, 19.27778845538743724 ) ) ;
#20592 = CARTESIAN_POINT ( 'NONE',  ( -189.5227851116837314, 18.00253723945986550, -43.46196956062437522 ) ) ;
#20594 = CARTESIAN_POINT ( 'NONE',  ( 130.8568914410475088, 4.207082182989012153, 52.36146031193425188 ) ) ;
#20595 = CARTESIAN_POINT ( 'NONE',  ( -135.8532207217289738, -30.84685318188647685, -2.449293598294708485E-15 ) ) ;
#20596 = CARTESIAN_POINT ( 'NONE',  ( -280.0000000000000000, 19.99999999999996092, 2.449293598294708485E-15 ) ) ;
#20597 = CARTESIAN_POINT ( 'NONE',  ( -86.96347745069643054, -40.00000000000026290, 21.75974354311608749 ) ) ;
#20598 = CARTESIAN_POINT ( 'NONE',  ( 14.38125909742181463, 10.73282306405862485, 67.30136555898259587 ) ) ;
#20599 = CARTESIAN_POINT ( 'NONE',  ( -190.0000000000000000, 61.50000000000009948, 66.50000000000005684 ) ) ;
#20600 = PRODUCT_DEFINITION_SHAPE ( 'NONE', 'NONE',  #10140 ) ;
#20601 = CARTESIAN_POINT ( 'NONE',  ( -56.48582580120558561, -21.81201906317755146, -21.81201906317792449 ) ) ;
#20602 = CARTESIAN_POINT ( 'NONE',  ( 146.6084372240433993, 24.48358557860341733, -24.48358557860313311 ) ) ;
#20603 = ORIENTED_EDGE ( 'NONE', *, *, #1674, .T. ) ;
#20604 = CARTESIAN_POINT ( 'NONE',  ( 130.8568914410475088, -52.36146031193419503, 4.207082182989537955 ) ) ;
#20605 = CARTESIAN_POINT ( 'NONE',  ( -97.73860346103491281, 8.185503821092320109, 20.89580782302881445 ) ) ;
#20606 = EDGE_CURVE ( 'NONE', #3292, #19647, #19748, .T. ) ;
#20607 = CARTESIAN_POINT ( 'NONE',  ( -213.1075012329536946, -37.98287015391263566, 37.98287015391218802 ) ) ;
#20608 = CARTESIAN_POINT ( 'NONE',  ( 6.371015797558896132, -44.80452650039788409, -18.55864253217484361 ) ) ;
#20609 = ORIENTED_EDGE ( 'NONE', *, *, #17433, .F. ) ;
#20610 = CARTESIAN_POINT ( 'NONE',  ( -103.9474983245026039, -20.15710290851505349, 8.027156558344394455 ) ) ;
#20611 = CARTESIAN_POINT ( 'NONE',  ( -82.23726319248024197, -13.38816524724604307, -15.17212319098400997 ) ) ;
#20612 = VERTEX_POINT ( 'NONE', #21777 ) ;
#20613 = CARTESIAN_POINT ( 'NONE',  ( 200.0000000000000284, 15.35911892145054303, -11.18589804280325772 ) ) ;
#20614 = DIRECTION ( 'NONE',  ( -1.000000000000000000, -0.000000000000000000, -0.000000000000000000 ) ) ;
#20615 = CARTESIAN_POINT ( 'NONE',  ( -189.6939645179714375, -43.50328570201185840, -18.01965094556654989 ) ) ;
#20616 = CARTESIAN_POINT ( 'NONE',  ( -162.0762913951020892, -1.777970010055771463E-13, 41.69427287682835015 ) ) ;
#20617 = CARTESIAN_POINT ( 'NONE',  ( 0.2972598230769930572, 54.33493731733936016, 2.449293598294708485E-15 ) ) ;
#20618 = CARTESIAN_POINT ( 'NONE',  ( 4.995406935893289102, 10.78321810389013002, -10.78321810388986712 ) ) ;
#20619 = CARTESIAN_POINT ( 'NONE',  ( 199.0249556294982938, -5.033924301686514724, 19.36137939705603017 ) ) ;
#20620 = VECTOR ( 'NONE', #17375, 1000.000000000000000 ) ;
#20621 = EDGE_CURVE ( 'NONE', #17844, #25529, #15642, .T. ) ;
#20622 = CARTESIAN_POINT ( 'NONE',  ( -238.4067589809705794, -1.892706720741712928E-13, 40.96449427998260973 ) ) ;
#20623 = CARTESIAN_POINT ( 'NONE',  ( 163.1118516004056573, 40.00000000000000711, 12.73709011382489642 ) ) ;
#20624 = CARTESIAN_POINT ( 'NONE',  ( 163.1118516004056573, 1.251511021549353291E-13, -27.26290988616872824 ) ) ;
#20625 = PLANE ( 'NONE',  #1145 ) ;
#20626 = CARTESIAN_POINT ( 'NONE',  ( -192.9588430854689705, -54.46834944099975928, -2.449293598294708485E-15 ) ) ;
#20627 = EDGE_CURVE ( 'NONE', #3446, #2384, #15348, .T. ) ;
#20628 = CARTESIAN_POINT ( 'NONE',  ( 19.06497207195982568, -38.31983398719646061, 38.31983398719606271 ) ) ;
#20629 = CARTESIAN_POINT ( 'NONE',  ( 4.995406935893290878, 1.606505379428369110E-13, -15.24977328854832592 ) ) ;
#20630 = CARTESIAN_POINT ( 'NONE',  ( -4.039451493210483690, -13.82811171175408127, -46.99046209229819482 ) ) ;
#20631 = CARTESIAN_POINT ( 'NONE',  ( -192.9588430854690273, 40.00000000000055422, -54.46834944101679810 ) ) ;
#20632 = CARTESIAN_POINT ( 'NONE',  ( -280.0000000000000568, 39.99999999999990763, 20.00000000000015987 ) ) ;
#20633 = CARTESIAN_POINT ( 'NONE',  ( 136.1360204305621551, 3.511608612530801032, -53.05693388239316022 ) ) ;
#20634 = DIRECTION ( 'NONE',  ( -1.000000000000000000, -1.303213150798907793E-16, -2.465190328815661892E-32 ) ) ;
#20635 = CARTESIAN_POINT ( 'NONE',  ( -114.4364955367327070, -8.644468109209471507, 20.04994829327649342 ) ) ;
#20636 = CARTESIAN_POINT ( 'NONE',  ( -208.1127848780264742, -38.89260858015758515, 38.89260858015713751 ) ) ;
#20637 = ORIENTED_EDGE ( 'NONE', *, *, #25837, .T. ) ;
#20638 = CARTESIAN_POINT ( 'NONE',  ( -39.84211263212320375, 32.75097567537659415, -13.56589830566843347 ) ) ;
#20639 = CARTESIAN_POINT ( 'NONE',  ( -109.1264249741455785, -33.12752917269520481, -13.72187187123273233 ) ) ;
#20640 = CARTESIAN_POINT ( 'NONE',  ( -213.1075012329537230, -53.71589010953668719, -40.00000000000002132 ) ) ;
#20641 = ADVANCED_FACE ( 'NONE', ( #24171 ), #16043, .T. ) ;
#20642 = CARTESIAN_POINT ( 'NONE',  ( -105.3895469845263193, 9.637191077568175501, 19.08279132546278944 ) ) ;
#20643 = CARTESIAN_POINT ( 'NONE',  ( -208.1127848780265026, 10.60833733269551615, -10.60833733269529766 ) ) ;
#20644 = EDGE_LOOP ( 'NONE', ( #18915, #8602, #22481, #7955, #19510, #13310 ) ) ;
#20645 = ORIENTED_EDGE ( 'NONE', *, *, #19953, .T. ) ;
#20646 = CIRCLE ( 'NONE', #7459, 4.999999999999997335 ) ;
#20647 = LINE ( 'NONE', #19047, #24926 ) ;
#20648 = CARTESIAN_POINT ( 'NONE',  ( -99.31364972220153220, 8.933506367398260650, -20.48028939131441817 ) ) ;
#20649 = CARTESIAN_POINT ( 'NONE',  ( 9.006212071482861958, 14.17897189022315985, 49.32687279760999388 ) ) ;
#20650 = EDGE_LOOP ( 'NONE', ( #21684, #19538, #13089, #17300 ) ) ;
#20651 = VERTEX_POINT ( 'NONE', #20394 ) ;
#20652 =( BOUNDED_SURFACE ( )  B_SPLINE_SURFACE ( 3, 2, ( 
 ( #11370, #19491, #1275 ),
 ( #23616, #7249, #9380 ),
 ( #11129, #23117, #5397 ),
 ( #11248, #8870, #13253 ),
 ( #16981, #1023, #23246 ),
 ( #17111, #9124, #6867 ),
 ( #13499, #25117, #4889 ),
 ( #21621, #19365, #15371 ),
 ( #5021, #17236, #1155 ),
 ( #15488, #9259, #17489 ),
 ( #21118, #12996, #17365 ),
 ( #25377, #23494, #5268 ),
 ( #13371, #21497, #15111 ),
 ( #25631, #765, #7377 ),
 ( #14983, #3396, #2895 ),
 ( #11003, #13126, #21247 ),
 ( #3021, #19113, #7129 ),
 ( #896, #9006, #25243 ) ),
 .UNSPECIFIED., .F., .F., .F. ) 
 B_SPLINE_SURFACE_WITH_KNOTS ( ( 4, 2, 2, 2, 2, 2, 2, 2, 4 ),
 ( 3, 3 ),
 ( 0.04072677041617866339, 0.04791560368711805795, 0.04971281200485290486, 0.05151002032258775176, 0.05510443695805744557, 0.06229327022899683319, 0.06409047854673168010, 0.06588768686446652700, 0.06948210349993622081 ),
 ( 0.000000000000000000, 1.000000000000000000 ),
 .UNSPECIFIED. ) 
 GEOMETRIC_REPRESENTATION_ITEM ( )  RATIONAL_B_SPLINE_SURFACE ( (
 ( 1.000000000000000000, 0.9548354694798303344, 1.000000000000000000),
 ( 1.000000000000000000, 0.9525322275551380002, 1.000000000000000000),
 ( 1.000000000000000000, 0.9507090892362719536, 1.000000000000000000),
 ( 1.000000000000000000, 0.9491274414775124901, 1.000000000000000000),
 ( 1.000000000000000000, 0.9488458707020273053, 1.000000000000000000),
 ( 1.000000000000000000, 0.9483593263061569356, 1.000000000000000000),
 ( 1.000000000000000000, 0.9481536722360313085, 1.000000000000000000),
 ( 1.000000000000000000, 0.9476504947197553763, 1.000000000000000000),
 ( 1.000000000000000000, 0.9474672091609203095, 1.000000000000000000),
 ( 1.000000000000000000, 0.9473824175298217742, 1.000000000000000000),
 ( 1.000000000000000000, 0.9479352607974392830, 1.000000000000000000),
 ( 1.000000000000000000, 0.9493585438922157449, 1.000000000000000000),
 ( 1.000000000000000000, 0.9496800154561187979, 1.000000000000000000),
 ( 1.000000000000000000, 0.9503966251880781035, 1.000000000000000000),
 ( 1.000000000000000000, 0.9507930044150058047, 1.000000000000000000),
 ( 1.000000000000000000, 0.9520783076861127903, 1.000000000000000000),
 ( 1.000000000000000000, 0.9530652557247718537, 1.000000000000000000),
 ( 1.000000000000000000, 0.9541700779530455367, 1.000000000000000000) ) ) 
 REPRESENTATION_ITEM ( '' )  SURFACE ( )  );
#20653 = CARTESIAN_POINT ( 'NONE',  ( -30.26275506840324070, -27.08623969584595770, 29.48230279907789608 ) ) ;
#20654 = CARTESIAN_POINT ( 'NONE',  ( 199.0257179982615128, -18.22226585379655361, 8.261159732268383848 ) ) ;
#20655 = DIRECTION ( 'NONE',  ( -0.3301743741154957168, 0.9439199556516647549, 0.000000000000000000 ) ) ;
#20656 = CONICAL_SURFACE ( 'NONE', #244, 19.53474504356807273, 0.7853981633974447263 ) ;
#20657 = CARTESIAN_POINT ( 'NONE',  ( -626.9846540392142060, 75.00000000000000000, -74.99999999999991473 ) ) ;
#20658 = CARTESIAN_POINT ( 'NONE',  ( -208.1127848780264742, 67.17687982760683951, 10.60833733268317403 ) ) ;
#20659 = PRODUCT_DEFINITION_FORMATION_WITH_SPECIFIED_SOURCE ( 'ANY', '', #12840, .NOT_KNOWN. ) ;
#20660 = AXIS2_PLACEMENT_3D ( 'NONE', #25989, #19583, #15454 ) ;
#20661 = CARTESIAN_POINT ( 'NONE',  ( -199.9999999999999716, -18.59955921182013228, 46.19968414209466800 ) ) ;
#20662 = CARTESIAN_POINT ( 'NONE',  ( -100.0968563617331881, -8.149320301599320970, -20.72609133243391710 ) ) ;
#20663 = CARTESIAN_POINT ( 'NONE',  ( -208.1127848780264742, 40.00000000000055422, -55.00245453014380814 ) ) ;
#20664 = CARTESIAN_POINT ( 'NONE',  ( 14.38125909742180220, 40.00000000000017764, -15.17850393972591760 ) ) ;
#20665 = CARTESIAN_POINT ( 'NONE',  ( -656.9887313867761804, 40.00305800795492672, 2.000664094296076279 ) ) ;
#20666 = AXIS2_PLACEMENT_3D ( 'NONE', #2032, #3614, #6142 ) ;
#20667 = CARTESIAN_POINT ( 'NONE',  ( -348.0000000000001137, -4.857225732735059864E-14, 31.79780246617542616 ) ) ;
#20668 = CARTESIAN_POINT ( 'NONE',  ( 199.0075440639197666, 19.83040477280651714, -2.587228267588620234 ) ) ;
#20669 = CARTESIAN_POINT ( 'NONE',  ( -187.7698581930822854, 23.34605429454593306, 42.84913646251166597 ) ) ;
#20670 = CARTESIAN_POINT ( 'NONE',  ( 192.4448373802100889, 14.14213562375873678, 14.14213562375894817 ) ) ;
#20671 = CARTESIAN_POINT ( 'NONE',  ( -105.2272256531192625, 2.713820371751817451, -21.35019504733632090 ) ) ;
#20672 = CARTESIAN_POINT ( 'NONE',  ( 57.59792236341148453, -26.56190807104700369, 26.56190807104673723 ) ) ;
#20673 = DIRECTION ( 'NONE',  ( -1.000000000000000000, -1.836970198721030181E-16, 0.000000000000000000 ) ) ;
#20674 = CARTESIAN_POINT ( 'NONE',  ( -208.1127848780264742, -38.89260858015704514, -38.89260858015768463 ) ) ;
#20675 = CARTESIAN_POINT ( 'NONE',  ( -280.0000000000000000, -5.143516556418885058E-14, -6.902532920683853297E-30 ) ) ;
#20676 = CARTESIAN_POINT ( 'NONE',  ( 57.59792236341147031, 2.435789363418171760, 0.000000000000000000 ) ) ;
#20677 =( GEOMETRIC_REPRESENTATION_CONTEXT ( 3 ) GLOBAL_UNCERTAINTY_ASSIGNED_CONTEXT ( ( #1570 ) ) GLOBAL_UNIT_ASSIGNED_CONTEXT ( ( #17119, #16986, #22990 ) ) REPRESENTATION_CONTEXT ( 'NONE', 'WORKASPACE' ) );
#20678 = CARTESIAN_POINT ( 'NONE',  ( 4.995406935893289102, 10.78321810389013002, -10.78321810388986712 ) ) ;
#20679 = CARTESIAN_POINT ( 'NONE',  ( 14.38125909742181285, -15.17850393972633505, 40.00000000000002132 ) ) ;
#20680 = CARTESIAN_POINT ( 'NONE',  ( -591.9832520071217914, 45.00109046910024801, 1.162667027830338595 ) ) ;
#20681 = CARTESIAN_POINT ( 'NONE',  ( -280.0000000000000568, -39.99999999999987210, -20.00000000000043343 ) ) ;
#20682 = CARTESIAN_POINT ( 'NONE',  ( 199.0084359913980165, 0.06319087311583088118, -19.99616937079735379 ) ) ;
#20683 = CARTESIAN_POINT ( 'NONE',  ( 159.7744820660627454, -10.75261058663780034, 25.95909830917674199 ) ) ;
#20684 = ORIENTED_EDGE ( 'NONE', *, *, #18676, .F. ) ;
#20685 = ORIENTED_EDGE ( 'NONE', *, *, #7195, .T. ) ;
#20686 = CARTESIAN_POINT ( 'NONE',  ( -135.8532207217289738, -9.153146818113595984, 40.00000000000002132 ) ) ;
#20687 = AXIS2_PLACEMENT_3D ( 'NONE', #25127, #8614, #14728 ) ;
#20688 = CARTESIAN_POINT ( 'NONE',  ( -626.9846540392097722, 75.00000000000000000, 59.99999999999999289 ) ) ;
#20689 = EDGE_CURVE ( 'NONE', #19072, #1425, #21312, .T. ) ;
#20690 = CARTESIAN_POINT ( 'NONE',  ( 57.59792236341147031, 26.56190807104720975, -26.56190807104655249 ) ) ;
#20691 = CARTESIAN_POINT ( 'NONE',  ( -110.0822598093819806, -19.77208535310723292, -4.084357705420478268 ) ) ;
#20692 = EDGE_CURVE ( 'NONE', #19908, #7220, #10277, .T. ) ;
#20693 = CIRCLE ( 'NONE', #7926, 15.00000000000000178 ) ;
#20694 = CARTESIAN_POINT ( 'NONE',  ( -188.7701102708081180, -43.14144101424763278, -23.55033952083658022 ) ) ;
#20695 = DIRECTION ( 'NONE',  ( 1.000000000000000000, 1.836970198721030427E-16, -0.000000000000000000 ) ) ;
#20696 = CARTESIAN_POINT ( 'NONE',  ( 199.9999999999998010, 4.312122466882670757, -18.50761716938983525 ) ) ;
#20697 = ADVANCED_FACE ( 'NONE', ( #3905 ), #25928, .T. ) ;
#20698 = EDGE_CURVE ( 'NONE', #17509, #23238, #5815, .T. ) ;
#20699 = CARTESIAN_POINT ( 'NONE',  ( 199.9999999999999147, 11.56007540354647389, -15.08186119327485386 ) ) ;
#20700 = CARTESIAN_POINT ( 'NONE',  ( 136.1360204305621551, -24.77266263493081766, -31.79587985999290112 ) ) ;
#20701 = FACE_OUTER_BOUND ( 'NONE', #6789, .T. ) ;
#20702 = CARTESIAN_POINT ( 'NONE',  ( 0.000000000000000000, 0.000000000000000000, -39.99999999999994316 ) ) ;
#20703 = CARTESIAN_POINT ( 'NONE',  ( 19.06497207195980792, 40.00000000000059686, -54.19242893257802507 ) ) ;
#20704 = CARTESIAN_POINT ( 'NONE',  ( 200.0000000000000000, -14.14213562373122457, 42.42640687119282461 ) ) ;
#20705 = CARTESIAN_POINT ( 'NONE',  ( -1.818469002956046188, 13.93708913181255049, 47.72215409237453798 ) ) ;
#20706 = CARTESIAN_POINT ( 'NONE',  ( -198.0356074513804572, 10.87444709759714989, 10.87444709759722450 ) ) ;
#20707 = CARTESIAN_POINT ( 'NONE',  ( -162.0762913951021176, -29.48230308784755493, -27.08623940707632372 ) ) ;
#20708 = CARTESIAN_POINT ( 'NONE',  ( 199.0067131358059953, 19.32749934108755241, -5.289875845814065336 ) ) ;
#20710 = CARTESIAN_POINT ( 'NONE',  ( 192.4448373802100889, -3.692737725850373501E-14, 19.99999999996060751 ) ) ;
#20709 = CARTESIAN_POINT ( 'NONE',  ( 14.38125909742181285, -17.55144818341421598, -39.01709431150935359 ) ) ;
#20711 = CARTESIAN_POINT ( 'NONE',  ( -86.96347745069644475, 41.18208027870576871, 15.38646221621837107 ) ) ;
#20712 = CARTESIAN_POINT ( 'NONE',  ( 22.17571259161255171, 47.24006242886041917, -13.86510691867242251 ) ) ;
#20713 = CARTESIAN_POINT ( 'NONE',  ( -105.3755690713226585, 18.24025645688350750, -40.00000000000002132 ) ) ;
#20714 = CARTESIAN_POINT ( 'NONE',  ( 57.59792236341147031, -1.722363176415032004, -1.722363176415048880 ) ) ;
#20715 = CARTESIAN_POINT ( 'NONE',  ( -100.7734535825088500, -22.67402823373193499, 40.00000000000002132 ) ) ;
#20716 = AXIS2_PLACEMENT_3D ( 'NONE', #3801, #13629, #9909 ) ;
#20717 = CARTESIAN_POINT ( 'NONE',  ( -8.720657192106740396, -41.62108041046438700, 22.53512351408631531 ) ) ;
#20718 = B_SPLINE_CURVE_WITH_KNOTS ( 'NONE', 3,
 ( #4806, #25414, #2806, #13041, #2676, #20763, #17282, #807, #6909, #19152, #4930, #19028, #8913, #15026, #17022, #11042, #937, #25285, #22889, #7041, #15157, #7165, #23284, #21286, #3060, #12771, #11163, #2533, #18760, #542, #24890, #6645, #20898, #15785, #15656, #19925, #9681, #23656, #13793, #25932, #3184, #1193, #15527, #11408, #9298, #5688, #17654, #3700, #17403, #11805, #19530, #1708, #7544, #21537, #25542, #13668, #1315, #17921, #25667, #5561, #3312, #5436, #13537, #21662, #9422, #3435, #23411, #11535 ),
 .UNSPECIFIED., .F., .F.,
 ( 4, 2, 2, 2, 2, 2, 2, 2, 2, 2, 2, 2, 2, 2, 2, 2, 2, 2, 2, 2, 2, 2, 2, 2, 2, 2, 2, 2, 2, 2, 2, 2, 2, 4 ),
 ( 1.132231036155057011E-16, 0.006124279316953675813, 0.007655349146192144856, 0.009186418975430613032, 0.01224855863390755806, 0.01531069829238450135, 0.01837283795086144464, 0.02449711726781507795, 0.02602818709705354006, 0.02755925692629199869, 0.03062139658476872861, 0.03674567590172217457, 0.03827674573096054300, 0.03980781556019890449, 0.04286995521867562747, 0.04593209487715235045, 0.04746316470639071194, 0.04899423453562907343, 0.05511851385258251246, 0.05664958368182088783, 0.05818065351105927707, 0.06124279316953602781, 0.06277386299877434073, 0.06430493282801265365, 0.06736707248648926560, 0.07042921214496587756, 0.07349135180344250340, 0.07961563112039596324, 0.08267777077887270010, 0.08420884060811119343, 0.08573991043734968676, 0.08880205009582670117, 0.09186418975430371558, 0.09798846907125773054 ),
 .UNSPECIFIED. ) ;
#20719 = CARTESIAN_POINT ( 'NONE',  ( 91.82158438592158234, 22.79471317813471742, 40.00000000000002132 ) ) ;
#20720 = ORIENTED_EDGE ( 'NONE', *, *, #25603, .F. ) ;
#20721 = CARTESIAN_POINT ( 'NONE',  ( 200.0000000000000000, -52.49999999999972289, -82.49999999999998579 ) ) ;
#20722 = CARTESIAN_POINT ( 'NONE',  ( 170.2234770963711128, -17.36149277826985937, -17.36149277826995174 ) ) ;
#20723 = PLANE ( 'NONE',  #6769 ) ;
#20724 = CARTESIAN_POINT ( 'NONE',  ( -3.696864809823408038, 23.52297716614975442, -43.10456217110547783 ) ) ;
#20725 = CARTESIAN_POINT ( 'NONE',  ( 199.0247296274817188, -19.55681251529712128, 4.220088366773818045 ) ) ;
#20726 = CARTESIAN_POINT ( 'NONE',  ( -198.0356074513804572, 39.15871834505887250, 17.40982414986519089 ) ) ;
#20727 = EDGE_CURVE ( 'NONE', #2818, #15298, #3898, .T. ) ;
#20728 = CARTESIAN_POINT ( 'NONE',  ( -87.11136440741971398, -21.34823163554633041, 2.379156564917666916 ) ) ;
#20729 = CARTESIAN_POINT ( 'NONE',  ( -87.13361725327072804, 8.813415818526478339E-15, 21.49321519333429009 ) ) ;
#20730 = CARTESIAN_POINT ( 'NONE',  ( -189.5227851117009266, -18.00253723946349993, 43.46196956062881611 ) ) ;
#20731 = CARTESIAN_POINT ( 'NONE',  ( 0.2972598230769957217, 1.502051041545559470E-13, -14.33493731733933352 ) ) ;
#20732 = CARTESIAN_POINT ( 'NONE',  ( -30.26275506840324070, 1.198031551616724366, -57.76657404653984429 ) ) ;
#20733 = CARTESIAN_POINT ( 'NONE',  ( -105.4288953903213581, 9.009229104226067264, -19.35825399500005162 ) ) ;
#20734 = CARTESIAN_POINT ( 'NONE',  ( -213.1075012329537230, 37.98287015391280619, -37.98287015391192512 ) ) ;
#20735 = CARTESIAN_POINT ( 'NONE',  ( 170.2234770963711128, -17.36149277827010096, 17.36149277826970660 ) ) ;
#20736 = CARTESIAN_POINT ( 'NONE',  ( -238.4067589809705794, -40.96449428006345528, 40.00000000000002132 ) ) ;
#20737 = CARTESIAN_POINT ( 'NONE',  ( -30.26275506840324070, 41.69427246844628598, 2.449293598294708485E-15 ) ) ;
#20738 = CARTESIAN_POINT ( 'NONE',  ( -135.8532207217289738, -1.208299557080134822E-13, 9.153146818113572891 ) ) ;
#20739 = CARTESIAN_POINT ( 'NONE',  ( 4.995406935893289102, 10.78321810388998081, 10.78321810389001811 ) ) ;
#20740 = CARTESIAN_POINT ( 'NONE',  ( -94.58360650932068836, 20.58386743644652128, -9.000712009836508543 ) ) ;
#20741 = CARTESIAN_POINT ( 'NONE',  ( 19.06497207195981858, -10.03556273973377166, -66.60410523465827737 ) ) ;
#20742 = CARTESIAN_POINT ( 'NONE',  ( 146.6084372240433709, 52.76785682606519146, 3.800685668858932775 ) ) ;
#20743 = ORIENTED_EDGE ( 'NONE', *, *, #795, .T. ) ;
#20744 = CARTESIAN_POINT ( 'NONE',  ( 136.1360204305621266, 3.511608612530704665, 3.511608612530695339 ) ) ;
#20745 = CARTESIAN_POINT ( 'NONE',  ( -93.01741312763938652, 8.169811845848039766, 20.82169463896921968 ) ) ;
#20746 = CONTEXT_DEPENDENT_SHAPE_REPRESENTATION ( #19868, #5924 ) ;
#20747 = CARTESIAN_POINT ( 'NONE',  ( -280.0000000000000568, 42.42640687119274645, 14.14213562373118194 ) ) ;
#20748 = CARTESIAN_POINT ( 'NONE',  ( -3.966425590329220263, -47.01685867532416552, -13.83202835294317445 ) ) ;
#20749 = EDGE_LOOP ( 'NONE', ( #24955, #9097, #16454, #9471 ) ) ;
#20750 = CARTESIAN_POINT ( 'NONE',  ( 4.995406935893288214, 15.24977328854832770, 0.000000000000000000 ) ) ;
#20751 = FACE_BOUND ( 'NONE', #12858, .T. ) ;
#20752 = EDGE_LOOP ( 'NONE', ( #23585, #18239, #3238, #26214 ) ) ;
#20753 = CARTESIAN_POINT ( 'NONE',  ( 199.9999999999998863, 18.97179924413623908, -1.226483293096950700 ) ) ;
#20754 = LINE ( 'NONE', #12489, #22597 ) ;
#20755 = CARTESIAN_POINT ( 'NONE',  ( 200.0000000000000000, 19.99999999999995737, 40.00000000000002132 ) ) ;
#20756 = CARTESIAN_POINT ( 'NONE',  ( 163.1118516004056573, -47.56205970284945295, -9.006482792074823607 ) ) ;
#20757 = CARTESIAN_POINT ( 'NONE',  ( 199.0152755141893692, 15.03153897770602221, 13.19647528785794677 ) ) ;
#20758 = CARTESIAN_POINT ( 'NONE',  ( -259.2033419157646676, -49.83842185052040463, 6.730120644403092101 ) ) ;
#20759 = CARTESIAN_POINT ( 'NONE',  ( 170.2234770963711128, -40.00000000000004263, 15.44714144992801685 ) ) ;
#20760 = CARTESIAN_POINT ( 'NONE',  ( 91.82158438592156813, 39.99999999999995737, 22.79471317813484887 ) ) ;
#20761 = CARTESIAN_POINT ( 'NONE',  ( 190.0000000000000284, -82.49999999999991473, -52.49999999999977973 ) ) ;
#20762 = CARTESIAN_POINT ( 'NONE',  ( -100.7734535825088500, 22.67402823373189946, -40.00000000000002132 ) ) ;
#20763 = CARTESIAN_POINT ( 'NONE',  ( -618.9777491934191858, 27.63863534162878111, 28.91606862897691954 ) ) ;
#20764 = CARTESIAN_POINT ( 'NONE',  ( -105.3755690713226585, -18.24025645688353947, -40.00000000000002132 ) ) ;
#20765 = CARTESIAN_POINT ( 'NONE',  ( 192.4448373802100889, -14.14213562370313682, 14.14213562370301958 ) ) ;
#20766 = CARTESIAN_POINT ( 'NONE',  ( 146.5090579137181237, -12.40347562390430447, -29.94463907179419948 ) ) ;
#20767 = CARTESIAN_POINT ( 'NONE',  ( -110.1018001840233893, 14.72021915949438764, -13.84057941999019725 ) ) ;
#20768 = CARTESIAN_POINT ( 'NONE',  ( 14.38125909742180930, 40.00000000000060396, -55.17850393974224232 ) ) ;
#20769 = CARTESIAN_POINT ( 'NONE',  ( 14.38125909742181818, -1.924622159709266762E-13, 55.17850393972636880 ) ) ;
#20770 = CARTESIAN_POINT ( 'NONE',  ( 146.6084372240433709, 3.800685668858776900, -52.76785682606518435 ) ) ;
#20771 = DIRECTION ( 'NONE',  ( -0.2259624731739453551, 0.9741360072993472397, 0.000000000000000000 ) ) ;
#20772 = CARTESIAN_POINT ( 'NONE',  ( -114.6382724355127749, -18.98542650371856055, 11.21026131167369400 ) ) ;
#20773 = CARTESIAN_POINT ( 'NONE',  ( -280.0000000000000568, -42.42640687119285303, -14.14213562373118371 ) ) ;
#20774 = VERTEX_POINT ( 'NONE', #15759 ) ;
#20775 = CARTESIAN_POINT ( 'NONE',  ( 184.8905102610680444, -14.79361573936399665, 14.79361573936367158 ) ) ;
#20776 = CARTESIAN_POINT ( 'NONE',  ( 130.8888609958234213, 29.49786752803547785, -12.21841679119709312 ) ) ;
#20777 = CARTESIAN_POINT ( 'NONE',  ( -198.0356074513804572, -55.37879056871328487, -40.00000000000002132 ) ) ;
#20778 = CIRCLE ( 'NONE', #24160, 14.99999999999999822 ) ;
#20779 = DIRECTION ( 'NONE',  ( 0.000000000000000000, 0.3028247695821854046, -0.9530462522498561739 ) ) ;
#20780 = CARTESIAN_POINT ( 'NONE',  ( 192.4448373802101173, -42.42640687122053578, -14.14213562370360577 ) ) ;
#20781 = ORIENTED_EDGE ( 'NONE', *, *, #24446, .T. ) ;
#20782 = VERTEX_POINT ( 'NONE', #17762 ) ;
#20783 = CARTESIAN_POINT ( 'NONE',  ( 199.9999999999999716, -8.687076164477627316, 16.91209170048031041 ) ) ;
#20784 = CARTESIAN_POINT ( 'NONE',  ( 110.0479209278586410, 9.419601331808891587, -22.74092928740043362 ) ) ;
#20785 = EDGE_CURVE ( 'NONE', #24029, #16073, #19582, .T. ) ;
#20786 = CARTESIAN_POINT ( 'NONE',  ( 6.615221834190998962, 14.16446777328907736, 49.23097633542939633 ) ) ;
#20787 = EDGE_LOOP ( 'NONE', ( #657, #14646, #13589, #21110 ) ) ;
#20788 = ORIENTED_EDGE ( 'NONE', *, *, #7036, .T. ) ;
#20789 = CARTESIAN_POINT ( 'NONE',  ( 151.7948205124836250, -23.49921654116339553, -23.49921654116350211 ) ) ;
#20790 = CARTESIAN_POINT ( 'NONE',  ( 199.0232268534825835, -20.00153578626446915, -0.3291254421221458948 ) ) ;
#20791 = CARTESIAN_POINT ( 'NONE',  ( -114.7824662270406151, -1.403530270408209768, 22.13040512712583308 ) ) ;
#20792 = CARTESIAN_POINT ( 'NONE',  ( -162.0762913951021176, 1.198031840315997298, 57.76657433523996588 ) ) ;
#20793 = FACE_BOUND ( 'NONE', #23428, .T. ) ;
#20794 = CARTESIAN_POINT ( 'NONE',  ( 170.2234770963711128, 40.00000000000014211, -24.55285855007172913 ) ) ;
#20795 = DIRECTION ( 'NONE',  ( 5.508077988093229047E-14, -1.000000000000000000, -1.842899034348521475E-14 ) ) ;
#20796 = EDGE_CURVE ( 'NONE', #5450, #5580, #22158, .T. ) ;
#20797 = CYLINDRICAL_SURFACE ( 'NONE', #2084, 20.53474504356812247 ) ;
#20798 = ADVANCED_FACE ( 'NONE', ( #11512, #19901, #9273, #1685, #13387, #5664 ), #25772, .F. ) ;
#20799 = CARTESIAN_POINT ( 'NONE',  ( -238.4067589809705794, 40.00000000000040501, -40.96449427990138759 ) ) ;
#20800 = CARTESIAN_POINT ( 'NONE',  ( -213.1075012329537230, 40.00000000000055422, -53.71589010953623244 ) ) ;
#20801 = CARTESIAN_POINT ( 'NONE',  ( -369.0000000000000568, -4.605747634845933236E-14, -20.53474504356812247 ) ) ;
#20802 = FACE_OUTER_BOUND ( 'NONE', #23512, .T. ) ;
#20803 = CARTESIAN_POINT ( 'NONE',  ( 199.0054597862206549, 11.64633275074771035, -16.26583636099561403 ) ) ;
#20804 = VECTOR ( 'NONE', #17488, 1000.000000000000000 ) ;
#20805 = CARTESIAN_POINT ( 'NONE',  ( -188.3392535381692312, 13.83023904993428488, 47.00481007172016490 ) ) ;
#20806 = CARTESIAN_POINT ( 'NONE',  ( -192.9588430854690273, -38.51493924976957572, 18.05360324515410397 ) ) ;
#20807 = CARTESIAN_POINT ( 'NONE',  ( -77.90255099906769942, -8.064892378657791738, -20.29001641120690635 ) ) ;
#20808 = CARTESIAN_POINT ( 'NONE',  ( -30.26275506840323359, -1.198031551616339341, 57.76657404653985139 ) ) ;
#20809 = DIRECTION ( 'NONE',  ( 0.000000000000000000, 1.000000000000000000, 0.000000000000000000 ) ) ;
#20810 = CARTESIAN_POINT ( 'NONE',  ( -213.1075012329536946, -37.98287015391210275, -37.98287015391272092 ) ) ;
#20811 = CARTESIAN_POINT ( 'NONE',  ( -638.5868188162663728, 30.55430815960217217, 33.04082901047623011 ) ) ;
#20812 = CARTESIAN_POINT ( 'NONE',  ( 19.06497207195981503, -14.19242893257840166, 0.000000000000000000 ) ) ;
#20813 = CARTESIAN_POINT ( 'NONE',  ( -280.0000000000000568, 42.42640687119265408, 14.14213562373147504 ) ) ;
#20814 = CARTESIAN_POINT ( 'NONE',  ( -162.0762913951021176, -1.694272876828353702, 40.00000000000002132 ) ) ;
#20815 = CARTESIAN_POINT ( 'NONE',  ( -592.9819114055728733, 44.22852218735779672, -8.380006196786844441 ) ) ;
#20816 = ORIENTED_EDGE ( 'NONE', *, *, #8422, .T. ) ;
#20817 = CARTESIAN_POINT ( 'NONE',  ( 57.59792236341149163, -39.99999999999961631, -37.56421063658228832 ) ) ;
#20818 = CARTESIAN_POINT ( 'NONE',  ( 199.0153906436953264, -13.35702860092365363, -14.88696670886333706 ) ) ;
#20819 = CARTESIAN_POINT ( 'NONE',  ( 156.1979191798867532, -11.34289806466604311, 27.38417834433170484 ) ) ;
#20820 = VERTEX_POINT ( 'NONE', #9790 ) ;
#20821 = ORIENTED_EDGE ( 'NONE', *, *, #23937, .T. ) ;
#20822 = CARTESIAN_POINT ( 'NONE',  ( -192.9588430854689989, 54.46834944099968823, 2.449293598294708485E-15 ) ) ;
#20823 = CARTESIAN_POINT ( 'NONE',  ( 155.4809970915717088, 11.45899766888337190, 27.66446758342039658 ) ) ;
#20824 = CIRCLE ( 'NONE', #14425, 15.00000000000000178 ) ;
#20825 = CARTESIAN_POINT ( 'NONE',  ( -105.2055636156392495, -21.49233843345434991, -1.377569041468663436 ) ) ;
#20826 = CARTESIAN_POINT ( 'NONE',  ( -626.9846540392142060, -82.50099999999990530, -30.00000000000004974 ) ) ;
#20827 = CARTESIAN_POINT ( 'NONE',  ( 200.0000000000000000, 7.347880794884121511E-14, 0.000000000000000000 ) ) ;
#20828 = CARTESIAN_POINT ( 'NONE',  ( 199.9999999999999147, 0.2978356717867484682, -19.00168788844713319 ) ) ;
#20829 = DIRECTION ( 'NONE',  ( 0.000000000000000000, 1.000000000000000000, 0.000000000000000000 ) ) ;
#20830 = CARTESIAN_POINT ( 'NONE',  ( -91.56559293963834989, -16.03295912088659492, -40.53558337403696044 ) ) ;
#20831 = CARTESIAN_POINT ( 'NONE',  ( 170.2234770963711128, 17.36149277826980253, 17.36149277827007253 ) ) ;
#20832 = FACE_OUTER_BOUND ( 'NONE', #10860, .T. ) ;
#20833 = CARTESIAN_POINT ( 'NONE',  ( 151.7948205124836534, 39.99999999999970157, 33.23291073765595627 ) ) ;
#20834 = CARTESIAN_POINT ( 'NONE',  ( -105.4741150117365009, 19.60045294981777531, -8.366608964619008049 ) ) ;
#20835 = CARTESIAN_POINT ( 'NONE',  ( -200.0000000000000853, -24.82633483071228753, -44.86878812508721381 ) ) ;
#20836 = CARTESIAN_POINT ( 'NONE',  ( 163.1118516004056573, -19.27778845538787422, 19.27778845538743724 ) ) ;
#20837 = CARTESIAN_POINT ( 'NONE',  ( -280.0000000000000000, -14.14213562373108779, 14.14213562373088529 ) ) ;
#20838 = CARTESIAN_POINT ( 'NONE',  ( 199.0119115731982333, 18.47776054338839202, 7.648009306434410348 ) ) ;
#20840 = CARTESIAN_POINT ( 'NONE',  ( 130.8568914410475372, 8.154165912415230659E-16, 5.949712681206690945 ) ) ;
#20839 = CARTESIAN_POINT ( 'NONE',  ( -208.1127848780265026, 10.60833733269551615, -10.60833733269529766 ) ) ;
#20841 = CARTESIAN_POINT ( 'NONE',  ( 59.93546481429514472, 31.86477106155505012, -13.19882033590626058 ) ) ;
#20842 = CARTESIAN_POINT ( 'NONE',  ( -105.3755690713226727, -21.75974354311652093, 0.000000000000000000 ) ) ;
#20843 = CARTESIAN_POINT ( 'NONE',  ( -91.56559293963834989, -16.03295912088716335, 40.53558337403673306 ) ) ;
#20844 = CARTESIAN_POINT ( 'NONE',  ( -56.48582580120559982, -9.153146818113595984, 40.00000000000002132 ) ) ;
#20845 = CARTESIAN_POINT ( 'NONE',  ( 12.96694272558651839, -49.19577900139863402, 14.15914421028645798 ) ) ;
#20846 = CARTESIAN_POINT ( 'NONE',  ( -56.48582580120559982, 30.84685318188643421, 40.00000000000002132 ) ) ;
#20847 = VERTEX_POINT ( 'NONE', #26041 ) ;
#20848 = CARTESIAN_POINT ( 'NONE',  ( 48.46027422359919967, -18.19770396007739066, -35.02097763790794716 ) ) ;
#20849 = CARTESIAN_POINT ( 'NONE',  ( -77.58728853844743867, 17.56910682997003192, 13.48988187297745966 ) ) ;
#20850 = CARTESIAN_POINT ( 'NONE',  ( -24.15343516389543055, -15.53299357113722934, 37.49996374338925165 ) ) ;
#20851 = VECTOR ( 'NONE', #21560, 1000.000000000000000 ) ;
#20852 = CARTESIAN_POINT ( 'NONE',  ( -4.421177063217966108, 23.37490463203949886, -42.89273859401248501 ) ) ;
#20853 = CARTESIAN_POINT ( 'NONE',  ( 199.0249934254769926, -19.32713910159323589, 5.171593721336591010 ) ) ;
#20854 = CARTESIAN_POINT ( 'NONE',  ( -86.96347745069644475, -15.38646221621807442, 15.38646221621768184 ) ) ;
#20855 = CARTESIAN_POINT ( 'NONE',  ( -199.9999999999999432, 14.17215463606722636, -49.28189405767596298 ) ) ;
#20856 = CARTESIAN_POINT ( 'NONE',  ( -188.6013942375887495, -23.51434495930345037, 43.09289976588207338 ) ) ;
#20857 = CARTESIAN_POINT ( 'NONE',  ( 130.8568914410475372, -3.326198072800416995E-13, 34.05028731879788495 ) ) ;
#20858 = CARTESIAN_POINT ( 'NONE',  ( -259.2033419157646676, -35.01439189186523748, -21.55415060305881170 ) ) ;
#20859 = CARTESIAN_POINT ( 'NONE',  ( 151.7948205124836250, 23.49921654116328540, 23.49921654116366554 ) ) ;
#20861 = CARTESIAN_POINT ( 'NONE',  ( -162.0762913951021176, 57.76657433523994456, -1.198031840315424867 ) ) ;
#20860 = CARTESIAN_POINT ( 'NONE',  ( -259.2033419157646676, 35.01439189186559275, -21.55415060305807984 ) ) ;
#20862 = CARTESIAN_POINT ( 'NONE',  ( -30.26275506840324070, 1.198031551616030033, -1.198031551616006496 ) ) ;
#20863 = CARTESIAN_POINT ( 'NONE',  ( -213.1075012329537230, -53.71589010950170717, 40.00000000000002132 ) ) ;
#20864 = CARTESIAN_POINT ( 'NONE',  ( -192.9588430854690273, 14.46834944099966336, -40.00000000000002132 ) ) ;
#20865 = CARTESIAN_POINT ( 'NONE',  ( 163.1118516004056573, -40.00000000000027711, 27.26290988616830546 ) ) ;
#20866 = CARTESIAN_POINT ( 'NONE',  ( 200.0000000000000000, 14.14213562373100608, -42.42640687119291698 ) ) ;
#20867 = ADVANCED_FACE ( 'NONE', ( #15259 ), #15502, .F. ) ;
#20868 = CARTESIAN_POINT ( 'NONE',  ( -190.0000000000000000, -66.50000000000001421, 66.50000000000005684 ) ) ;
#20869 = CARTESIAN_POINT ( 'NONE',  ( -91.56559293963834989, 16.03295912088740849, -40.53558337403661938 ) ) ;
#20870 = ADVANCED_FACE ( 'NONE', ( #5162 ), #17381, .F. ) ;
#20871 = CARTESIAN_POINT ( 'NONE',  ( -183.1090696429828881, 45.18841929383577138, -13.45963186434148184 ) ) ;
#20872 = VERTEX_POINT ( 'NONE', #15386 ) ;
#20873 = CARTESIAN_POINT ( 'NONE',  ( -213.1075012329537230, 37.98287015391228749, 37.98287015391245802 ) ) ;
#20874 = VECTOR ( 'NONE', #2487, 1000.000000000000000 ) ;
#20875 = AXIS2_PLACEMENT_3D ( 'NONE', #3914, #20133, #16403 ) ;
#20876 = AXIS2_PLACEMENT_3D ( 'NONE', #7953, #3987, #12086 ) ;
#20877 = CARTESIAN_POINT ( 'NONE',  ( -188.2995950289364089, -13.82811170417104840, -46.99046209955525200 ) ) ;
#20878 = CARTESIAN_POINT ( 'NONE',  ( 130.8568914410475372, -4.207082182992846420, 4.207082182992822439 ) ) ;
#20879 = CARTESIAN_POINT ( 'NONE',  ( 13.08024833513275453, -44.78264744452988566, -18.54957993048723708 ) ) ;
#20880 = ADVANCED_FACE ( 'NONE', ( #19638, #3162, #25520 ), #3286, .F. ) ;
#20881 = EDGE_CURVE ( 'NONE', #19457, #18917, #14068, .T. ) ;
#20882 = ORIENTED_EDGE ( 'NONE', *, *, #8428, .F. ) ;
#20883 = CARTESIAN_POINT ( 'NONE',  ( -56.48582580120559271, -9.153146818113595984, 0.000000000000000000 ) ) ;
#20884 = CARTESIAN_POINT ( 'NONE',  ( -200.0000000000000000, -39.01096890182076038, 39.01096890182031274 ) ) ;
#20885 = CARTESIAN_POINT ( 'NONE',  ( 200.0000000000001990, 8.399020763088516972, -17.04381686846133803 ) ) ;
#20886 = CARTESIAN_POINT ( 'NONE',  ( 21.15358250000285878, 13.91686544622536914, -47.58740525741993821 ) ) ;
#20887 = CARTESIAN_POINT ( 'NONE',  ( 91.82158438592158234, 22.79471317813471742, 40.00000000000002132 ) ) ;
#20888 = CARTESIAN_POINT ( 'NONE',  ( -56.48582580120559271, -6.472252184284276844, 6.472252184284108978 ) ) ;
#20889 = CARTESIAN_POINT ( 'NONE',  ( 199.0124915487878923, 17.99959093953023270, 8.716253503037693307 ) ) ;
#20890 = AXIS2_PLACEMENT_3D ( 'NONE', #4724, #2864, #4855 ) ;
#20891 = AXIS2_PLACEMENT_3D ( 'NONE', #19191, #22667, #8953 ) ;
#20892 = CARTESIAN_POINT ( 'NONE',  ( -238.4067589809705794, -57.25054294077233408, -0.6820004458489551391 ) ) ;
#20893 = CARTESIAN_POINT ( 'NONE',  ( -86.96347745069643054, -40.00000000000009948, 18.24025645688337960 ) ) ;
#20894 = CARTESIAN_POINT ( 'NONE',  ( 170.2234770963711128, 40.00000000000014211, -24.55285855007172913 ) ) ;
#20895 = PLANE ( 'NONE',  #8731 ) ;
#20896 = CARTESIAN_POINT ( 'NONE',  ( -86.96347745069644475, -18.24025645688354302, -2.449293598294708485E-15 ) ) ;
#20898 = CARTESIAN_POINT ( 'NONE',  ( -597.0557355404389455, 39.94671229542147017, 2.128033897213765790 ) ) ;
#20897 = CARTESIAN_POINT ( 'NONE',  ( 22.17571259161159603, -13.86510691867019318, -47.24006242886260054 ) ) ;
#20899 = CARTESIAN_POINT ( 'NONE',  ( 19.06497207195982924, -54.19242893257843008, -40.00000000000002132 ) ) ;
#20900 = CARTESIAN_POINT ( 'NONE',  ( 130.8568914410475088, 24.07718906446891793, 32.49135343045489321 ) ) ;
#20901 = CARTESIAN_POINT ( 'NONE',  ( 144.9504669809062705, -12.48392651407822740, -30.13886470195703282 ) ) ;
#20902 = CARTESIAN_POINT ( 'NONE',  ( 210.0000000000000284, 75.52305771588345351, -68.47933392563552957 ) ) ;
#20903 = CARTESIAN_POINT ( 'NONE',  ( -56.48582580120559982, 40.00000000000034106, -30.84685318188602210 ) ) ;
#20904 = CARTESIAN_POINT ( 'NONE',  ( 4.995406935893292655, 39.99999999999982947, 55.24977328856478209 ) ) ;
#20905 = CARTESIAN_POINT ( 'NONE',  ( 19.06497207195980792, 10.03556273973433299, 10.03556273973436319 ) ) ;
#20906 = CARTESIAN_POINT ( 'NONE',  ( 23.37394308801976806, 42.85717664514618264, -23.33966569535049373 ) ) ;
#20907 = DIRECTION ( 'NONE',  ( -1.750717563385750846E-16, 0.9530462522498558409, 0.3028247695821862928 ) ) ;
#20908 = CARTESIAN_POINT ( 'NONE',  ( -213.1075012329537230, -66.26714140138676612, 9.698598906462487790 ) ) ;
#20909 = ORIENTED_EDGE ( 'NONE', *, *, #5708, .F. ) ;
#20911 = CARTESIAN_POINT ( 'NONE',  ( -24.51100708737205736, 37.39427017785519780, -15.48921386273512013 ) ) ;
#20910 = CARTESIAN_POINT ( 'NONE',  ( 192.4448373802100889, 14.14213562375873678, 14.14213562375894817 ) ) ;
#20912 = CARTESIAN_POINT ( 'NONE',  ( 153.3020327024397602, 28.42252382389430565, -11.77299484472932711 ) ) ;
#20913 = CARTESIAN_POINT ( 'NONE',  ( -213.1075012329536946, -53.71589010951918652, -2.449293598294708485E-15 ) ) ;
#20914 = CARTESIAN_POINT ( 'NONE',  ( -188.2995950289364941, -43.00522595870984333, 23.44932284465888728 ) ) ;
#20915 = FACE_BOUND ( 'NONE', #18197, .T. ) ;
#20916 = ORIENTED_EDGE ( 'NONE', *, *, #19629, .T. ) ;
#20917 = ORIENTED_EDGE ( 'NONE', *, *, #24526, .T. ) ;
#20918 = CARTESIAN_POINT ( 'NONE',  ( -99.29480781227090347, 8.934325994365451606, -20.48155342677145541 ) ) ;
#20919 = CARTESIAN_POINT ( 'NONE',  ( -93.01854144614549114, 8.553566903984137326, -20.65013722627613646 ) ) ;
#20920 = CARTESIAN_POINT ( 'NONE',  ( 22.80622392652794517, 17.87980911537470874, 43.16567765897936937 ) ) ;
#20921 = VERTEX_POINT ( 'NONE', #18386 ) ;
#20922 = B_SPLINE_SURFACE_WITH_KNOTS ( 'NONE', 1, 3, ( 
 ( #18767, #16763, #24897, #21165, #22897, #4676, #6389, #14505, #22636, #8519, #2408, #16637, #10518, #24766, #14630, #22767, #9052, #23290, #3067, #5066, #25291, #13172, #21293, #19159, #7048, #15165, #943, #17157, #26004, #2048, #8015, #26277, #39, #15998, #24532, #22001, #7739, #20405, #12147, #16130, #22134, #10155, #18258, #10017, #8152, #14140, #24125, #14406, #24260, #20269, #1912, #6288, #13868, #2179, #10287, #15851, #3771, #11875, #2303, #5896, #22536, #6034, #19995, #12278, #6161, #22272, #18395, #16266, #172, #14004, #23981, #8278, #3915, #20532, #12014, #20134, #18125, #4046, #1781, #24395, #9885, #14271, #22407, #4183, #16404, #12407, #4317, #17853, #5760, #7877, #17986, #26134, #23192, #14798, #6683, #24934, #10689, #16797, #447, #14932, #4840, #25197, #4710, #18933, #22929, #24663, #581, #20937, #12534, #8413, #2715, #23069, #4440, #25064, #8551, #311, #12814, #18660, #20668, #10820, #16667, #14538, #10549, #18801, #22800, #715, #8819, #2437, #4577, #14660, #16535, #24798, #12674, #2848, #8688, #21195, #16930, #6816, #10412, #13080, #6550, #4972, #6944, #12946, #21062, #22668, #10956, #19062, #8954, #18530, #844, #17063, #6420, #15062, #20803, #2575, #6151, #22126, #2169, #19986, #18517, #20261, #3906, #18385, #8270, #2293, #8142, #22400, #31, #1770, #4038, #24386, #15987, #11866, #14261, #165, #7867, #10278, #12004, #3761, #2040, #20126, #24115, #16258, #1905, #17979, #13995, #22261, #26268, #4175, #12269, #5887, #8004, #18117, #9876, #10009, #16121, #6281, #14132, #24652, #20395, #16391, #13857, #16524, #24251, #298, #10403, #10143, #24523, #26125, #12137, #14396, #12397, #21992, #22528, #4308, #6025, #20522, #18247, #8402, #18789, #2834, #16784, #19051, #4829, #10943, #13066, #10538, #14525, #8942, #701, #4696, #10676, #16919, #6804, #24920, #25053, #2704, #12663, #2956, #14787, #8807, #6672, #21183, #2428, #17048, #25184, #22656, #18650, #435, #17175, #4567, #11066, #20925, #8539, #833, #21050, #22917, #6933, #14916, #15051, #20790, #4430, #23180, #2561, #9068, #570, #8675, #12798, #10809, #16656, #12934, #24787, #18919, #4959, #23057, #19179, #963, #6408, #12523, #20654, #22788, #6539, #14649, #11688, #3331, #21557, #13434, #25565, #5207, #19429, #5324, #21311, #23677, #3086, #11431, #5457, #3202 ),
 ( #3459, #19552, #9193, #25819, #7187, #19678, #1339, #15678, #17677, #13691, #1215, #7565, #23803, #21430, #5584, #21685, #25438, #17306, #11185, #11311, #9445, #1600, #17550, #25688, #13190, #11557, #7436, #21813, #15550, #15303, #9702, #9568, #25308, #7068, #13559, #13311, #1467, #3585, #19301, #9318, #17425, #7312, #15183, #15426, #23430, #23553, #19813, #23308, #5085, #1084, #16218, #14357, #11963, #24211, #3860, #22088, #7963, #12096, #5982, #18076, #20088, #1867, #8231, #20218, #10103, #26088, #6113, #23933, #22486, #16082, #1729, #1996, #12354, #4135, #9970, #12228, #15115, #17808, #26228, #14090, #22221, #3997, #25954, #18205, #8099, #24349, #14221, #15940, #20483, #16349, #17942, #6244, #22357, #20352, #5848, #2128, #4266, #10236, #2258, #18346, #127, #7696, #24481, #15808, #5710, #13814, #21948, #3724, #11827, #19945, #9837, #7823, #24072, #13954, #18748, #12760, #20753, #25147, #6367, #12896, #2793, #256, #14486, #22618, #21148, #8501, #15015, #24878, #4394, #4794, #25014, #529, #21010, #10768, #10905, #16614, #8365, #19017, #24747, #13028, #14613, #6502, #4527, #16745, #12488, #8768, #20613, #22879, #16883, #22748, #12625, #4916, #2523, #14748, #10640, #396, #796, #8899, #23145, #4656, #6634, #20885, #8635, #2663, #18881, #14880, #17010, #6898, #660, #6767, #23019, #24613, #10365, #18476, #2388, #16488, #10500, #18613, #23273, #17518, #1051, #19141, #9284, #11154, #13155, #15397, #19269, #7024, #3047, #11278, #15270, #11395, #3301, #5048, #23400, #7154, #925, #21275, #5176, #21650, #3174, #13656, #21525, #19517, #2922, #5548, #9157, #15643, #25784, #17392, #23645, #15143, #19399, #25657, #1434, #11031, #11524, #7403, #9035, #23521, #21401, #19649, #13279, #15515, #1182, #5423, #1304, #13526, #9533, #17268, #17139, #3422, #5293, #25532, #7280, #13401, #9412, #17643, #7534, #25403, #23770, #25274, #93, #11930, #5677, #5950, #16319, #8066, #13920, #16186, #3966, #21780, #22055, #9935, #24039, #3829, #3553, #14060, #20055, #1834, #12065, #19915, #24443, #12198, #21916, #10205, #15907, #20182, #9804, #7791, #8201, #5816, #6212, #1966, #10072, #11654, #24319, #26195, #18041, #19779, #18176, #6084, #18311, #14189, #17775, #1566, #26324, #2096, #7933, #9671, #25918, #22323, #16049, #7662, #24174, #15773, #22191, #4098 ) ),
 .UNSPECIFIED., .F., .T., .F.,
 ( 2, 2 ),
 ( 4, 2, 2, 2, 2, 2, 2, 2, 2, 2, 2, 2, 2, 2, 2, 2, 2, 2, 2, 2, 2, 2, 2, 2, 2, 2, 2, 2, 2, 2, 2, 2, 2, 2, 2, 2, 2, 2, 2, 2, 2, 2, 2, 2, 2, 2, 2, 2, 2, 2, 2, 2, 2, 2, 2, 2, 2, 2, 2, 2, 2, 2, 2, 2, 2, 2, 2, 2, 2, 2, 2, 2, 2, 2, 2, 2, 2, 2, 2, 2, 2, 2, 2, 2, 2, 2, 2, 2, 2, 2, 2, 2, 2, 2, 2, 2, 2, 2, 2, 2, 2, 2, 2, 2, 2, 2, 2, 2, 2, 2, 2, 2, 2, 2, 2, 2, 2, 2, 2, 2, 2, 2, 2, 2, 2, 2, 2, 2, 2, 2, 2, 2, 2, 2, 2, 2, 2, 2, 2, 2, 2, 2, 2, 2, 2, 2, 2, 2, 4 ),
 ( 0.000000000000000000, 1.000000000000000000 ),
 ( 0.001986339241202381145, 0.003842975313193646575, 0.004771293349189279290, 0.005235452367187095647, 0.005699611385184912005, 0.006163770403182728362, 0.006627929421180544720, 0.007092088439178361077, 0.007556247457176177434, 0.008484565493171810149, 0.009412883529167442864, 0.01034120156516307558, 0.01126951960115870829, 0.01173367861915652552, 0.01219783763715434101, 0.01266199665515215650, 0.01312615567314997372, 0.01405447370914560644, 0.01498279174514123915, 0.01683942781713250458, 0.01776774585312813903, 0.01869606388912377001, 0.01916022290712158377, 0.01962438192511940099, 0.02008854094311721822, 0.02055269996111503544, 0.02148101799711066989, 0.02240933603310630087, 0.02333765406910193185, 0.02426597210509756630, 0.02519429014109320075, 0.02565844915909101798, 0.02612260817708883173, 0.02658676719508664549, 0.02705092621308446271, 0.02797924424908009716, 0.02983588032107136259, 0.03076419835706699357, 0.03122835737506481080, 0.03169251639306262802, 0.03215667541106044525, 0.03262083442905826247, 0.03354915246505389692, 0.03447747050104953137, 0.03540578853704515888, 0.03633410657304078639, 0.03726242460903642084, 0.03772658362703423807, 0.03819074264503205529, 0.03865490166302987252, 0.03911906068102768974, 0.04004737871702332419, 0.04097569675301895864, 0.04283233282501022060, 0.04376065086100584811, 0.04468896889700148256, 0.04561728693299711701, 0.04654560496899275146, 0.04840224104098402036, 0.04933055907697965481, 0.05025887711297528232, 0.05072303613097309261, 0.05118719514897090983, 0.05165135416696872706, 0.05211551318496654428, 0.05304383122096217873, 0.05397214925695781318, 0.05490046729295344763, 0.05582878532894908208, 0.05675710336494471653, 0.05722126238294253375, 0.05768542140094034404, 0.05814958041893815432, 0.05861373943693597155, 0.05954205747293160600, 0.06139869354492287490, 0.06325532961691412992, 0.06511196568890539882, 0.06604028372490103327, 0.06696860176089666772, 0.06743276077889448494, 0.06789691979689230217, 0.06836107881489011939, 0.06882523783288793662, 0.06975355586888357107, 0.07068187390487920552, 0.07161019194087483997, 0.07253850997687047442, 0.07300266899486829164, 0.07346682801286610887, 0.07393098703086392609, 0.07439514604886174332, 0.07485930506685956054, 0.07532346408485737776, 0.07625178212085299834, 0.07810841819284425336, 0.07903673622883988781, 0.07950089524683770503, 0.07996505426483552226, 0.08042921328283333948, 0.08089337230083115671, 0.08182169033682679116, 0.08275000837282242561, 0.08367832640881806006, 0.08460664444481369451, 0.08553496248080932896, 0.08646328051680496340, 0.08692743953480278063, 0.08739159855280059785, 0.08785575757079841508, 0.08831991658879623230, 0.08924823462479186675, 0.09110487069678312178, 0.09203318873277874235, 0.09296150676877437680, 0.09342566578677219402, 0.09388982480477001125, 0.09435398382276782847, 0.09481814284076564570, 0.09574646087676128015, 0.09667477891275691460, 0.09760309694875254904, 0.09853141498474818349, 0.09899557400274600072, 0.09945973302074381794, 0.09992389203874163517, 0.1003880510567394524, 0.1022446871287307213, 0.1041013232007219902, 0.1050296412367176246, 0.1054938002547154419, 0.1059579592727132452, 0.1064221182907110486, 0.1068862773087088658, 0.1078145953447045002, 0.1096712314166957691, 0.1105995494526914036, 0.1115278674886870380, 0.1124561855246826725, 0.1133845035606783069, 0.1143128215966739414, 0.1152411396326695758, 0.1170977757046608447, 0.1180260937406564792, 0.1184902527586542964, 0.1189544117766521136, 0.1194185707946499309, 0.1198827298126477481, 0.1208110478486433687 ),
 .UNSPECIFIED. ) ;
#20923 = EDGE_LOOP ( 'NONE', ( #14217, #13806, #9098, #4254 ) ) ;
#20924 = CARTESIAN_POINT ( 'NONE',  ( -213.1075012329537230, 9.698598906462684965, 66.26714140138669507 ) ) ;
#20925 = CARTESIAN_POINT ( 'NONE',  ( 199.0212029771548430, -19.33411866963394488, -5.169619751639646488 ) ) ;
#20926 = CARTESIAN_POINT ( 'NONE',  ( -105.3901353554229701, -6.689050419637368350, 20.30436174852050968 ) ) ;
#20927 = CARTESIAN_POINT ( 'NONE',  ( 151.7948205124836534, -51.78348778862535795, 4.785054706298367044 ) ) ;
#20928 = CARTESIAN_POINT ( 'NONE',  ( -370.0000000000001137, -4.611870868841670624E-14, 19.53474504356807273 ) ) ;
#20929 = CARTESIAN_POINT ( 'NONE',  ( -280.0000000000000568, 39.99999999999990763, 20.00000000000015987 ) ) ;
#20930 = CARTESIAN_POINT ( 'NONE',  ( -199.9999999999999716, -23.83302776610003093, 44.89135967046721731 ) ) ;
#20931 = FACE_OUTER_BOUND ( 'NONE', #1214, .T. ) ;
#20932 = CARTESIAN_POINT ( 'NONE',  ( -30.26275506840323359, 4.336144384597734078E-13, -41.69427246844629309 ) ) ;
#20933 = CARTESIAN_POINT ( 'NONE',  ( -135.8532207217289738, -1.208299557080134822E-13, 9.153146818113572891 ) ) ;
#20934 = CARTESIAN_POINT ( 'NONE',  ( -631.0954681582677495, 26.75583256651325570, 29.73466928390865860 ) ) ;
#20935 = CIRCLE ( 'NONE', #9438, 5.000000000000004441 ) ;
#20936 = CARTESIAN_POINT ( 'NONE',  ( -87.02159731754392169, -18.50722648783487756, -10.86245144029295595 ) ) ;
#20937 = CARTESIAN_POINT ( 'NONE',  ( 199.0099419815959436, 19.67222971740176618, 3.604179563970075773 ) ) ;
#20938 = CARTESIAN_POINT ( 'NONE',  ( -183.1090696430172784, 22.43564075022590032, 41.47043467732703448 ) ) ;
#20939 = CARTESIAN_POINT ( 'NONE',  ( 0.2972598230770027716, -38.42060263243681817, 18.14793986248684377 ) ) ;
#20940 = DIRECTION ( 'NONE',  ( 0.000000000000000000, 0.000000000000000000, 1.000000000000000000 ) ) ;
#20941 = CARTESIAN_POINT ( 'NONE',  ( 163.1118516004056573, -9.006482792069636645, 9.006482792069567367 ) ) ;
#20942 = CARTESIAN_POINT ( 'NONE',  ( -77.65695844554161908, -18.42387585928431903, 12.10528775144916125 ) ) ;
#20943 = CARTESIAN_POINT ( 'NONE',  ( -238.4067589809705794, -0.6820004457337348613, -57.25054294065803617 ) ) ;
#20944 = CARTESIAN_POINT ( 'NONE',  ( -661.3556259495545646, 44.51244333536754993, 6.632513892488236529 ) ) ;
#20945 = CARTESIAN_POINT ( 'NONE',  ( 130.8568914410475088, 34.05028731879790627, 40.00000000000002132 ) ) ;
#20946 = CARTESIAN_POINT ( 'NONE',  ( -213.1075012329537230, 37.98287015391211696, 18.58567234101190735 ) ) ;
#20947 = CARTESIAN_POINT ( 'NONE',  ( 136.1360204305621266, 35.03383547441298873, 0.000000000000000000 ) ) ;
#20948 = CARTESIAN_POINT ( 'NONE',  ( -609.3550727715755784, 33.31827460164921462, -30.25570868770995858 ) ) ;
#20949 = EDGE_LOOP ( 'NONE', ( #2920, #13062 ) ) ;
#20950 = CARTESIAN_POINT ( 'NONE',  ( 130.8568914410475372, 8.880724697947696879E-14, -5.949712681206690945 ) ) ;
#20951 = DIRECTION ( 'NONE',  ( 0.000000000000000000, 1.000000000000000000, 0.000000000000000000 ) ) ;
#20952 = LINE ( 'NONE', #12689, #6460 ) ;
#20953 = ORIENTED_EDGE ( 'NONE', *, *, #15241, .T. ) ;
#20954 = ORIENTED_EDGE ( 'NONE', *, *, #14191, .F. ) ;
#20955 = CARTESIAN_POINT ( 'NONE',  ( 151.7948205124836250, 6.767089262349059275, 2.449293598294708485E-15 ) ) ;
#20956 = CARTESIAN_POINT ( 'NONE',  ( -110.0904723790853694, -19.95170499002752962, 3.161343376076289235 ) ) ;
#20957 = CARTESIAN_POINT ( 'NONE',  ( -200.0000000000000000, 74.99999999999995737, 9.184850993605144000E-15 ) ) ;
#20958 = CARTESIAN_POINT ( 'NONE',  ( 146.6084372240433709, -39.99999999999987921, -34.62501878078319351 ) ) ;
#20959 = CARTESIAN_POINT ( 'NONE',  ( 200.0000000000005116, -0.6320235832414241584, -19.00127953747481868 ) ) ;
#20960 = CARTESIAN_POINT ( 'NONE',  ( 199.9999999999999147, -2.484827300297501207, -18.84147750260992638 ) ) ;
#20961 = CARTESIAN_POINT ( 'NONE',  ( -100.7734535825088500, -44.31723036834885932, -12.25131212657538171 ) ) ;
#20962 = CARTESIAN_POINT ( 'NONE',  ( -91.56559293963836410, 16.03295912088692177, 16.03295912088721664 ) ) ;
#20963 = CARTESIAN_POINT ( 'NONE',  ( -109.1264249741455359, -13.72187187124633212, -33.12752917268956310 ) ) ;
#20964 = CARTESIAN_POINT ( 'NONE',  ( 192.4448373802101173, 39.99999999999985079, 20.00000000003984013 ) ) ;
#20965 = CARTESIAN_POINT ( 'NONE',  ( -213.1075012329537230, -9.698598906450422774, -9.698598906450550672 ) ) ;
#20966 = CARTESIAN_POINT ( 'NONE',  ( -192.9588430854689989, -14.46834944099973086, 0.000000000000000000 ) ) ;
#20967 = CARTESIAN_POINT ( 'NONE',  ( -162.0762913951020892, 29.48230308784758691, 29.48230308784772191 ) ) ;
#20968 = ADVANCED_FACE ( 'NONE', ( #13996 ), #4025, .T. ) ;
#20969 = CARTESIAN_POINT ( 'NONE',  ( 130.8568914410475088, -32.49135343045460900, -24.07718906446924478 ) ) ;
#20970 = CARTESIAN_POINT ( 'NONE',  ( -259.2033419157646676, 9.517827891722584255, -0.000000000000000000 ) ) ;
#20972 = CARTESIAN_POINT ( 'NONE',  ( 192.4448373802100889, 1.051811698935164031E-13, -20.00000000003942091 ) ) ;
#20971 = CARTESIAN_POINT ( 'NONE',  ( -208.1127848780264742, -17.67593391476605547, -38.89260858015755673 ) ) ;
#20973 = CARTESIAN_POINT ( 'NONE',  ( 14.38125909742180752, 15.17850393972634038, 0.000000000000000000 ) ) ;
#20974 = CARTESIAN_POINT ( 'NONE',  ( 57.59792236341147031, -30.00663442387700641, 26.56190807104681895 ) ) ;
#20975 = CARTESIAN_POINT ( 'NONE',  ( 14.38125909742180752, 15.17850393972634038, 40.00000000000002132 ) ) ;
#20976 = VERTEX_POINT ( 'NONE', #8143 ) ;
#20977 = CARTESIAN_POINT ( 'NONE',  ( 16.10036699863115217, -44.47262139759284594, 24.53427828610336903 ) ) ;
#20978 = CARTESIAN_POINT ( 'NONE',  ( 170.2234770963711128, 15.44714144992819094, 2.449293598294708485E-15 ) ) ;
#20979 = EDGE_LOOP ( 'NONE', ( #691, #10491, #5619, #21719 ) ) ;
#20980 = FACE_OUTER_BOUND ( 'NONE', #14288, .T. ) ;
#20981 = CARTESIAN_POINT ( 'NONE',  ( 4.995406935893289102, 10.78321810388998081, 10.78321810389001811 ) ) ;
#20982 = CARTESIAN_POINT ( 'NONE',  ( -62.69292774200316387, -11.76166271883654701, 24.97541154609807634 ) ) ;
#20983 = CARTESIAN_POINT ( 'NONE',  ( -105.3755690713226727, -15.38646221621786481, -15.38646221621789856 ) ) ;
#20984 = CARTESIAN_POINT ( 'NONE',  ( 21.99343714674524364, -13.87412077874951954, -47.30053030063390906 ) ) ;
#20985 = CARTESIAN_POINT ( 'NONE',  ( 199.0205961407162931, -18.94296041394271768, -6.425165802706580997 ) ) ;
#20986 = CARTESIAN_POINT ( 'NONE',  ( 192.4448373802101173, 14.14213562370261279, 42.42640687122091236 ) ) ;
#20987 = CARTESIAN_POINT ( 'NONE',  ( -77.58513204269964092, -21.97516623137529379, 2.423266694425164847 ) ) ;
#20988 = CARTESIAN_POINT ( 'NONE',  ( -194.7884774423581007, -18.40784251727884779, 44.44046305925472495 ) ) ;
#20989 = CARTESIAN_POINT ( 'NONE',  ( -213.1075012329537230, -9.698598906450422774, -9.698598906450550672 ) ) ;
#20990 = CARTESIAN_POINT ( 'NONE',  ( -198.0356074513804572, -10.87444709759729911, 10.87444709759714812 ) ) ;
#20991 = CARTESIAN_POINT ( 'NONE',  ( 91.82158438592158234, -40.45024623143936537, -16.11829626348475131 ) ) ;
#20992 = CARTESIAN_POINT ( 'NONE',  ( 19.06497207195981147, -10.03556273973425483, -10.03556273973443247 ) ) ;
#20994 = CARTESIAN_POINT ( 'NONE',  ( -135.8532207217289738, 21.81201906317798134, -21.81201906317747685 ) ) ;
#20993 = CARTESIAN_POINT ( 'NONE',  ( 4.995406935893293543, -10.78321810388990265, -10.78321810389009272 ) ) ;
#20995 = CARTESIAN_POINT ( 'NONE',  ( 19.06497207195979726, 38.31983398719604139, 18.24870850772803976 ) ) ;
#20996 = CARTESIAN_POINT ( 'NONE',  ( -259.2033419157646676, 9.517827891722584255, -0.000000000000000000 ) ) ;
#20997 = CARTESIAN_POINT ( 'NONE',  ( 146.6084372240433709, -34.62501878078303008, -40.00000000000002132 ) ) ;
#20998 = CARTESIAN_POINT ( 'NONE',  ( -192.9588430854690273, 38.51493924976939098, -18.05360324515436687 ) ) ;
#20999 = CARTESIAN_POINT ( 'NONE',  ( -716.9846540392142060, -66.50000000000001421, 61.50000000000005684 ) ) ;
#21000 = CARTESIAN_POINT ( 'NONE',  ( 151.7948205124836534, -33.06932595376376582, 23.49921654115996006 ) ) ;
#21001 = CARTESIAN_POINT ( 'NONE',  ( -114.4364955367344834, 20.29001642038889841, -8.064892380842916708 ) ) ;
#21002 = ORIENTED_EDGE ( 'NONE', *, *, #17510, .F. ) ;
#21003 = CARTESIAN_POINT ( 'NONE',  ( 136.1360204305621551, -24.77266263493126885, 31.79587985999256006 ) ) ;
#21004 = CARTESIAN_POINT ( 'NONE',  ( -716.9846540392142060, -66.50000000000001421, -71.50000000000005684 ) ) ;
#21005 = CARTESIAN_POINT ( 'NONE',  ( -198.0356074513804572, -10.87444709760996986, 67.44298959253333692 ) ) ;
#21006 = CARTESIAN_POINT ( 'NONE',  ( 3.869409319527063129, -44.61273074174947340, -24.63759630013054647 ) ) ;
#21007 = VERTEX_POINT ( 'NONE', #16259 ) ;
#21008 = CARTESIAN_POINT ( 'NONE',  ( -315.0000000000000568, -4.857225732735059864E-14, 0.000000000000000000 ) ) ;
#21009 = CARTESIAN_POINT ( 'NONE',  ( -114.7826396787322665, -15.64922767586158336, -15.64922767586183738 ) ) ;
#21010 = CARTESIAN_POINT ( 'NONE',  ( 199.9999999999998579, 17.67836847945686429, -6.970492097432807732 ) ) ;
#21011 = CARTESIAN_POINT ( 'NONE',  ( -114.7469200037856325, -21.93717741968544743, 2.762404124414108875 ) ) ;
#21012 = EDGE_CURVE ( 'NONE', #20921, #9153, #20262, .T. ) ;
#21013 = CARTESIAN_POINT ( 'NONE',  ( -208.1127848780264742, 55.00245453010919050, -40.00000000000002132 ) ) ;
#21014 = CARTESIAN_POINT ( 'NONE',  ( 57.59792236341147031, -30.00663442387662627, -26.56190807104723461 ) ) ;
#21015 = CARTESIAN_POINT ( 'NONE',  ( 199.0132385929227610, 17.30986399168244461, 10.02103235953326710 ) ) ;
#21016 = ADVANCED_FACE ( 'NONE', ( #16525 ), #6152, .T. ) ;
#21017 = CARTESIAN_POINT ( 'NONE',  ( 151.7948205124835681, -4.785054706298876859, 51.78348778862533663 ) ) ;
#21018 = CARTESIAN_POINT ( 'NONE',  ( 163.1118516004056573, -40.00000000000003553, 12.73709011382460687 ) ) ;
#21019 = CARTESIAN_POINT ( 'NONE',  ( 184.8905102610680444, 39.99999999999999289, 19.07866798485573057 ) ) ;
#21020 = CARTESIAN_POINT ( 'NONE',  ( -190.0000000000000000, 1.836970198721033928E-15, 0.000000000000000000 ) ) ;
#21021 = CARTESIAN_POINT ( 'NONE',  ( 0.2972598230770129857, -54.33493731733936016, -40.00000000000002132 ) ) ;
#21023 = DIRECTION ( 'NONE',  ( 1.000000000000000000, 1.836970198721030181E-16, 0.000000000000000000 ) ) ;
#21022 = CARTESIAN_POINT ( 'NONE',  ( 22.90311673802995784, -23.44499648834451122, -42.99920082299706792 ) ) ;
#21024 = EDGE_CURVE ( 'NONE', #24029, #3167, #19987, .T. ) ;
#21025 = CARTESIAN_POINT ( 'NONE',  ( -238.4067589809705794, -40.96449428006345528, 40.00000000000002132 ) ) ;
#21026 = ADVANCED_FACE ( 'NONE', ( #5888 ), #16392, .T. ) ;
#21027 = CARTESIAN_POINT ( 'NONE',  ( -105.3755690713226585, 43.67073346367970288, 12.89780903124427702 ) ) ;
#21028 = CARTESIAN_POINT ( 'NONE',  ( 127.8236149080041457, -11.91256696755843336, -28.75948073575753128 ) ) ;
#21029 = CARTESIAN_POINT ( 'NONE',  ( -315.0000000000000568, -4.593501166854459721E-14, -21.53474504356810115 ) ) ;
#21030 = CARTESIAN_POINT ( 'NONE',  ( -280.0000000000000568, 40.00000000000017764, -19.99999999999959144 ) ) ;
#21031 = CARTESIAN_POINT ( 'NONE',  ( -162.0762913951020892, 1.198031840385716418, 1.198031840385750169 ) ) ;
#21032 = CARTESIAN_POINT ( 'NONE',  ( 98.29820294268191105, -7.653668647302824368, -18.47759065022797031 ) ) ;
#21033 = CARTESIAN_POINT ( 'NONE',  ( -210.0000000000000284, -66.50000000000001421, -66.50000000000005684 ) ) ;
#21034 = CARTESIAN_POINT ( 'NONE',  ( 200.0000000000000000, 14.14213562373083022, 42.42640687119289566 ) ) ;
#21035 = ORIENTED_EDGE ( 'NONE', *, *, #9941, .F. ) ;
#21037 = CARTESIAN_POINT ( 'NONE',  ( -8.197988474444796836, 42.01088836873199739, -17.40147972966091316 ) ) ;
#21036 = CARTESIAN_POINT ( 'NONE',  ( -77.61378591600549726, 3.452311433137887242, -21.81972450369060113 ) ) ;
#21038 = CARTESIAN_POINT ( 'NONE',  ( 200.0000000000000000, 57.47694228411675255, -64.52066607436459833 ) ) ;
#21039 = CARTESIAN_POINT ( 'NONE',  ( -30.26275506840322649, -41.69427246844630019, -2.449293598294708485E-15 ) ) ;
#21040 = SHAPE_REPRESENTATION ( 'Universal cardan joints', ( #21058 ), #3629 ) ;
#21041 = CARTESIAN_POINT ( 'NONE',  ( 200.0000000000000000, 57.47694228411675255, -64.52066607436459833 ) ) ;
#21042 = CARTESIAN_POINT ( 'NONE',  ( -189.0540043420996028, 43.34487664254652373, -17.95403576473043827 ) ) ;
#21043 = ORIENTED_EDGE ( 'NONE', *, *, #3001, .F. ) ;
#21044 = ORIENTED_EDGE ( 'NONE', *, *, #14380, .T. ) ;
#21045 = FACE_OUTER_BOUND ( 'NONE', #830, .T. ) ;
#21046 = CARTESIAN_POINT ( 'NONE',  ( -88.37877758188231780, 8.026456973467151812, -20.15391234951717792 ) ) ;
#21047 = EDGE_LOOP ( 'NONE', ( #16916, #1897, #19235, #24202 ) ) ;
#21048 = ORIENTED_EDGE ( 'NONE', *, *, #21919, .T. ) ;
#21049 = CARTESIAN_POINT ( 'NONE',  ( -208.1127848780264742, -17.67593391476659548, 38.89260858015730804 ) ) ;
#21050 = CARTESIAN_POINT ( 'NONE',  ( 199.0223302282441296, -19.84245377806801613, -2.613091800807908260 ) ) ;
#21051 = CARTESIAN_POINT ( 'NONE',  ( -110.1003821002462786, 1.261039542895549426, 20.16525298253472442 ) ) ;
#21052 = CARTESIAN_POINT ( 'NONE',  ( 163.1118516004056573, -47.56205970284957374, 9.006482792074162802 ) ) ;
#21053 = CARTESIAN_POINT ( 'NONE',  ( -105.2054292635175585, 21.49321519473984665, 5.610018989487960791E-28 ) ) ;
#21054 = CARTESIAN_POINT ( 'NONE',  ( -259.2033419157646676, 39.99999999999987210, 30.48217210827754542 ) ) ;
#21055 = CARTESIAN_POINT ( 'NONE',  ( -193.0908841288064650, -24.29092413197462008, 44.14257353178379617 ) ) ;
#21056 = CARTESIAN_POINT ( 'NONE',  ( -626.9846540392142060, -82.50099999999990530, 30.00000000000004974 ) ) ;
#21057 = CARTESIAN_POINT ( 'NONE',  ( -86.96347745069643054, -40.00000000000026290, 21.75974354311608749 ) ) ;
#21058 = AXIS2_PLACEMENT_3D ( 'NONE', #7994, #22, #15977 ) ;
#21059 = CARTESIAN_POINT ( 'NONE',  ( -91.56559293963834989, -2.543181659092656077E-13, 22.67402823373191723 ) ) ;
#21060 = CARTESIAN_POINT ( 'NONE',  ( 189.9999999999999716, 82.50000000000008527, -52.49999999999977973 ) ) ;
#21061 = CARTESIAN_POINT ( 'NONE',  ( 23.37394308801976806, -13.80096434448233111, -46.80823611210209378 ) ) ;
#21062 = CARTESIAN_POINT ( 'NONE',  ( 199.0054956575951621, 16.44889389956343706, -11.36889162147346255 ) ) ;
#21063 = CARTESIAN_POINT ( 'NONE',  ( -189.0540043421010807, 17.95403576473130869, 43.34487664254734085 ) ) ;
#21064 = CARTESIAN_POINT ( 'NONE',  ( 91.82158438592158234, 12.16597498397756993, 12.16597498397776356 ) ) ;
#21065 = CARTESIAN_POINT ( 'NONE',  ( -315.0000000000000568, -4.593501166854459721E-14, -21.53474504356810115 ) ) ;
#21066 = CARTESIAN_POINT ( 'NONE',  ( -259.2033419157646676, 6.730120644403214669, 49.83842185052034068 ) ) ;
#21067 = CARTESIAN_POINT ( 'NONE',  ( -77.66977424857952883, 21.51855955734878023, -4.737087604909469896 ) ) ;
#21068 = CIRCLE ( 'NONE', #15916, 4.999999999999997335 ) ;
#21069 = CIRCLE ( 'NONE', #3225, 60.00000000000011369 ) ;
#21070 = CARTESIAN_POINT ( 'NONE',  ( -91.56559293963834989, 16.03295912088740849, -40.53558337403661938 ) ) ;
#21071 = DIRECTION ( 'NONE',  ( 0.000000000000000000, 0.000000000000000000, 1.000000000000000000 ) ) ;
#21072 = CARTESIAN_POINT ( 'NONE',  ( -210.0000000000000284, 66.50000000000009948, -66.50000000000005684 ) ) ;
#21073 = ORIENTED_EDGE ( 'NONE', *, *, #5562, .F. ) ;
#21074 = CARTESIAN_POINT ( 'NONE',  ( 184.8905102610680444, -14.79361573936399665, 14.79361573936367158 ) ) ;
#21075 = CARTESIAN_POINT ( 'NONE',  ( -91.56559293963836410, 22.67402823373190301, 40.00000000000002132 ) ) ;
#21076 = CARTESIAN_POINT ( 'NONE',  ( -602.0130363958678572, 37.72923481230851195, 24.52994204380139109 ) ) ;
#21077 = VERTEX_POINT ( 'NONE', #10279 ) ;
#21078 = CARTESIAN_POINT ( 'NONE',  ( 184.8905102610680444, -39.99999999999978684, -19.07866798485600768 ) ) ;
#21079 = CARTESIAN_POINT ( 'NONE',  ( 199.0084075218435657, 0.1388852900563516679, -19.99583393261218589 ) ) ;
#21080 = DIRECTION ( 'NONE',  ( -1.000000000000000000, -1.836970198721030181E-16, 0.000000000000000000 ) ) ;
#21081 = AXIS2_PLACEMENT_3D ( 'NONE', #23886, #5663, #3673 ) ;
#21082 = EDGE_LOOP ( 'NONE', ( #6530, #9874 ) ) ;
#21083 = ORIENTED_EDGE ( 'NONE', *, *, #20058, .F. ) ;
#21084 = EDGE_LOOP ( 'NONE', ( #23710, #21035, #10806, #11338 ) ) ;
#21085 = CARTESIAN_POINT ( 'NONE',  ( 4.995406935893288214, 55.24977328853207581, 40.00000000000002132 ) ) ;
#21086 = PRODUCT_DEFINITION_FORMATION_WITH_SPECIFIED_SOURCE ( 'ANY', '', #12748, .NOT_KNOWN. ) ;
#21087 = DIRECTION ( 'NONE',  ( 1.000000000000000000, -1.836970198721030181E-16, -0.000000000000000000 ) ) ;
#21088 = VECTOR ( 'NONE', #17279, 1000.000000000000000 ) ;
#21089 = CARTESIAN_POINT ( 'NONE',  ( -105.2333497862505141, -21.31134136416374147, 2.723647965523766423 ) ) ;
#21090 = CARTESIAN_POINT ( 'NONE',  ( 98.29820294267528880, -14.14213562373450017, -14.14213562373441668 ) ) ;
#21091 = DIRECTION ( 'NONE',  ( -4.657398277317547006E-32, 1.682156097916904081E-16, 1.000000000000000000 ) ) ;
#21092 = CARTESIAN_POINT ( 'NONE',  ( 199.9999999999998863, -4.016713260438497635, -18.57371263647062420 ) ) ;
#21093 = APPLICATION_CONTEXT ( 'automotive_design' ) ;
#21094 = CIRCLE ( 'NONE', #23221, 15.00000000000000355 ) ;
#21095 = CARTESIAN_POINT ( 'NONE',  ( 199.9999999999999147, -3.405556461844650329, -18.69721604853318908 ) ) ;
#21096 = CARTESIAN_POINT ( 'NONE',  ( 151.7948205124836534, -23.49921654115981084, -33.06932595376387951 ) ) ;
#21097 = CARTESIAN_POINT ( 'NONE',  ( -86.96347745069644475, 15.38646221621772092, 15.38646221621800336 ) ) ;
#21098 = CARTESIAN_POINT ( 'NONE',  ( -114.7826396784770822, -16.62870539743747855, -14.66974995413669092 ) ) ;
#21099 = CARTESIAN_POINT ( 'NONE',  ( 200.0000000000000000, 40.00000000000026290, -19.99999999999950617 ) ) ;
#21100 = CARTESIAN_POINT ( 'NONE',  ( 199.9999999999999432, 14.14213562373093680, 14.14213562373114641 ) ) ;
#21101 = CARTESIAN_POINT ( 'NONE',  ( -105.3755690713226869, 21.75974354311648540, -0.000000000000000000 ) ) ;
#21102 = CARTESIAN_POINT ( 'NONE',  ( -30.26275506840322649, -29.48230279907810925, 29.48230279907778950 ) ) ;
#21103 = CARTESIAN_POINT ( 'NONE',  ( 199.0121267835791627, 18.30962774096152046, 8.053342476213535051 ) ) ;
#21105 = CARTESIAN_POINT ( 'NONE',  ( -135.8532207217289738, 40.00000000000002842, -9.153146818113432559 ) ) ;
#21104 = CARTESIAN_POINT ( 'NONE',  ( 57.59792236341147031, -1.722363176415055985, 1.722363176415024677 ) ) ;
#21106 = VECTOR ( 'NONE', #8939, 1000.000000000000000 ) ;
#21107 = CARTESIAN_POINT ( 'NONE',  ( -100.7734535825088358, -22.67402823373193499, 0.000000000000000000 ) ) ;
#21108 = CARTESIAN_POINT ( 'NONE',  ( 91.82158438592158234, -40.45024623143958564, 16.11829626348418998 ) ) ;
#21109 = CARTESIAN_POINT ( 'NONE',  ( -208.1127848780264742, 55.00245453014418473, 40.00000000000002132 ) ) ;
#21110 = ORIENTED_EDGE ( 'NONE', *, *, #25555, .T. ) ;
#21111 = CARTESIAN_POINT ( 'NONE',  ( 6.011245401506787545, -44.78331514753931231, 18.54985650214110748 ) ) ;
#21112 = CARTESIAN_POINT ( 'NONE',  ( 19.06497207195980792, 14.19242893257840699, -40.00000000000002132 ) ) ;
#21113 = EDGE_CURVE ( 'NONE', #12221, #12267, #8985, .T. ) ;
#21114 = CARTESIAN_POINT ( 'NONE',  ( 170.0000000000000284, -24.25569233607176756, -6.285860131565255138 ) ) ;
#21115 = AXIS2_PLACEMENT_3D ( 'NONE', #8037, #3797, #1669 ) ;
#21116 = CARTESIAN_POINT ( 'NONE',  ( 91.82158438592158234, 16.11829626346139577, 16.11829626346143840 ) ) ;
#21117 = CARTESIAN_POINT ( 'NONE',  ( 57.59792236341148453, -40.00000000000000000, -2.435789363418300546 ) ) ;
#21118 = CARTESIAN_POINT ( 'NONE',  ( -87.11465200126595221, 21.36863955987802655, -2.590445302511781289 ) ) ;
#21119 = EDGE_CURVE ( 'NONE', #23459, #14634, #7402, .T. ) ;
#21120 = CARTESIAN_POINT ( 'NONE',  ( 21.15737826136113853, -13.91467835516619367, -47.57244852138559565 ) ) ;
#21121 = CARTESIAN_POINT ( 'NONE',  ( 200.0000000000000853, -13.44239485489230290, 13.44239485489200803 ) ) ;
#21122 = CARTESIAN_POINT ( 'NONE',  ( 91.82158438592158234, 16.11829626348378142, 40.45024623143977749 ) ) ;
#21123 = ADVANCED_FACE ( 'NONE', ( #4309 ), #24047, .T. ) ;
#21124 = DIRECTION ( 'NONE',  ( 0.000000000000000000, 0.000000000000000000, -1.000000000000000000 ) ) ;
#21125 = CARTESIAN_POINT ( 'NONE',  ( -87.08870976744344716, 3.405966936676973589, 21.20092391030562595 ) ) ;
#21126 = CARTESIAN_POINT ( 'NONE',  ( -189.1288815661669958, -13.87115472123802462, 47.28031329128408800 ) ) ;
#21127 = CARTESIAN_POINT ( 'NONE',  ( 146.6084372240433993, -3.357462877844280890E-13, 34.62501878078305850 ) ) ;
#21128 = EDGE_CURVE ( 'NONE', #7186, #19106, #23181, .T. ) ;
#21129 = CARTESIAN_POINT ( 'NONE',  ( -91.56559293963834989, 16.03295912088683650, 40.53558337403684675 ) ) ;
#21130 = CARTESIAN_POINT ( 'NONE',  ( 160.9163046357249129, -135.7889608577475542, -55.61140153332245006 ) ) ;
#21131 = CARTESIAN_POINT ( 'NONE',  ( -56.48582580120559982, 34.75652343174628101, -21.81201906317743067 ) ) ;
#21133 = CARTESIAN_POINT ( 'NONE',  ( 130.8568914410475372, 4.207082182992923691, -4.207082182992794017 ) ) ;
#21132 = CARTESIAN_POINT ( 'NONE',  ( -135.8532207217289738, 6.472252184284096543, 6.472252184284234211 ) ) ;
#21134 = CARTESIAN_POINT ( 'NONE',  ( -280.0000000000000000, 14.14213562373108246, -14.14213562373078581 ) ) ;
#21135 = CARTESIAN_POINT ( 'NONE',  ( -86.96347745069644475, -21.75974354311651737, 0.000000000000000000 ) ) ;
#21136 = CARTESIAN_POINT ( 'NONE',  ( -56.48582580120559271, -6.472252184284187138, -6.472252184284199572 ) ) ;
#21137 = DIRECTION ( 'NONE',  ( 0.000000000000000000, 0.000000000000000000, -1.000000000000000000 ) ) ;
#21138 = CARTESIAN_POINT ( 'NONE',  ( -198.0356074513804572, -67.44298959253333692, -10.87444709761016348 ) ) ;
#21139 = CARTESIAN_POINT ( 'NONE',  ( -114.4388184736442469, 20.16431396440428614, -8.352332320010020794 ) ) ;
#21140 = ORIENTED_EDGE ( 'NONE', *, *, #11030, .F. ) ;
#21141 = CARTESIAN_POINT ( 'NONE',  ( -56.48582580120559982, -6.472252184284282173, 50.09629031063965243 ) ) ;
#21142 = AXIS2_PLACEMENT_3D ( 'NONE', #7153, #793, #15514 ) ;
#21143 = FACE_OUTER_BOUND ( 'NONE', #6240, .T. ) ;
#21144 = CARTESIAN_POINT ( 'NONE',  ( -192.9588430854690273, 18.05360324515418924, 38.51493924976949756 ) ) ;
#21145 = CARTESIAN_POINT ( 'NONE',  ( -24.15343516395653012, -37.49996374353147388, -15.53299357101481704 ) ) ;
#21146 = VERTEX_POINT ( 'NONE', #19052 ) ;
#21147 = CARTESIAN_POINT ( 'NONE',  ( -144.0562564044143414, -29.54282788290112904, 14.68019406016581030 ) ) ;
#21148 = CARTESIAN_POINT ( 'NONE',  ( 199.9999999999998863, 18.47321080301961160, -4.449129010553737551 ) ) ;
#21149 = CARTESIAN_POINT ( 'NONE',  ( -114.5450021253299866, -20.85732849908723097, -6.791646844857083032 ) ) ;
#21150 = CARTESIAN_POINT ( 'NONE',  ( 0.2972598230769930017, 14.33493731733933352, -40.00000000000002132 ) ) ;
#21151 = CARTESIAN_POINT ( 'NONE',  ( -726.9846540392142060, -66.50000000000001421, 66.50000000000005684 ) ) ;
#21152 = CARTESIAN_POINT ( 'NONE',  ( 199.0207542291320522, 6.104323864361830942, 19.05092312409432154 ) ) ;
#21153 = CARTESIAN_POINT ( 'NONE',  ( -135.8532207217289738, -50.09629031063973770, 6.472252184283735943 ) ) ;
#21154 = CARTESIAN_POINT ( 'NONE',  ( -105.3755690713226585, 39.99999999999993605, 18.24025645688366737 ) ) ;
#21155 = CARTESIAN_POINT ( 'NONE',  ( 19.06497207195980792, 39.99999999999983658, 54.19242893257857929 ) ) ;
#21156 = CARTESIAN_POINT ( 'NONE',  ( -210.0000000000000284, 52.49999999999988631, -82.49999999999998579 ) ) ;
#21157 = CARTESIAN_POINT ( 'NONE',  ( -238.4067589809705794, -40.96449427990185654, -40.00000000000002132 ) ) ;
#21159 = CARTESIAN_POINT ( 'NONE',  ( 136.1360204305621266, 24.77266263493138965, -24.77266263493110188 ) ) ;
#21158 = CARTESIAN_POINT ( 'NONE',  ( 19.44355705748453289, -18.20455056367453750, -43.94967286773175630 ) ) ;
#21160 = CARTESIAN_POINT ( 'NONE',  ( -56.48582580120559982, 9.153146818113574668, 40.00000000000002132 ) ) ;
#21161 = CARTESIAN_POINT ( 'NONE',  ( 170.2234770963711128, 17.36149277827004411, -17.36149277826983095 ) ) ;
#21162 = CARTESIAN_POINT ( 'NONE',  ( 136.1360204305621266, -3.419521671106983309E-13, 35.03383547441296741 ) ) ;
#21163 = DIRECTION ( 'NONE',  ( -0.7071067811865549002, 8.659560562354844111E-17, -0.7071067811865401342 ) ) ;
#21164 = CARTESIAN_POINT ( 'NONE',  ( -100.7734535825088500, -40.00000000000027711, 22.67402823373149801 ) ) ;
#21165 = CARTESIAN_POINT ( 'NONE',  ( 199.0263115711520072, -12.44642065545630238, 15.66510279686564289 ) ) ;
#21166 = CARTESIAN_POINT ( 'NONE',  ( 169.9999999999999716, -22.62041470344880523, -9.369682556672316309 ) ) ;
#21167 = CARTESIAN_POINT ( 'NONE',  ( -91.56559293963834989, 12.25131212657428748, 44.31723036834913643 ) ) ;
#21168 = CARTESIAN_POINT ( 'NONE',  ( 14.38125909742180752, 17.55144818341448953, 39.01709431150923280 ) ) ;
#21169 = ORIENTED_EDGE ( 'NONE', *, *, #10101, .F. ) ;
#21171 = CARTESIAN_POINT ( 'NONE',  ( -77.90022806218905771, 20.16431395584832131, -8.352332316461433592 ) ) ;
#21170 = CARTESIAN_POINT ( 'NONE',  ( -100.7734535825088500, 16.03295912088691821, 16.03295912088721309 ) ) ;
#21172 = CARTESIAN_POINT ( 'NONE',  ( 159.7744820660626885, 25.95909830917692673, -10.75261058663744507 ) ) ;
#21173 = CARTESIAN_POINT ( 'NONE',  ( -56.48582580120559982, 9.153146818113574668, 40.00000000000002132 ) ) ;
#21174 = EDGE_CURVE ( 'NONE', #2595, #17928, #2957, .T. ) ;
#21175 = CARTESIAN_POINT ( 'NONE',  ( -189.1288337602818501, 47.28029723722971767, -13.87115233298132999 ) ) ;
#21176 = ORIENTED_EDGE ( 'NONE', *, *, #13523, .F. ) ;
#21177 = EDGE_LOOP ( 'NONE', ( #21849, #18818, #20346, #1592 ) ) ;
#21178 = CARTESIAN_POINT ( 'NONE',  ( 199.9999999999999147, 0.2942279655520377291, 19.00909807434749865 ) ) ;
#21179 = FACE_OUTER_BOUND ( 'NONE', #2950, .T. ) ;
#21180 = EDGE_CURVE ( 'NONE', #6050, #15177, #11515, .T. ) ;
#21181 = ORIENTED_EDGE ( 'NONE', *, *, #22319, .T. ) ;
#21182 = VERTEX_POINT ( 'NONE', #10944 ) ;
#21183 = CARTESIAN_POINT ( 'NONE',  ( 199.0196534518890701, -18.22073438007316071, -8.257363271777977687 ) ) ;
#21184 = DIRECTION ( 'NONE',  ( 1.000000000000000000, 1.836970198721030181E-16, 0.000000000000000000 ) ) ;
#21185 = EDGE_CURVE ( 'NONE', #14871, #10760, #18790, .T. ) ;
#21186 = CARTESIAN_POINT ( 'NONE',  ( -208.1127848780264742, 10.60833733270764867, 67.17687982763166588 ) ) ;
#21187 = CARTESIAN_POINT ( 'NONE',  ( -105.3287628664957651, 20.69538202814367622, 5.523081874391006174 ) ) ;
#21188 = CARTESIAN_POINT ( 'NONE',  ( -105.3755690713226585, 40.00000000000007816, -21.75974354311636461 ) ) ;
#21189 = CARTESIAN_POINT ( 'NONE',  ( -200.0000000000000284, -47.96425349429453888, 15.65821854886114295 ) ) ;
#21190 = CARTESIAN_POINT ( 'NONE',  ( 190.0000000000000000, -66.50000000000001421, 66.50000000000005684 ) ) ;
#21191 = CARTESIAN_POINT ( 'NONE',  ( 146.6084372240433709, -39.99999999999993605, -5.374981219217395356 ) ) ;
#21192 = CARTESIAN_POINT ( 'NONE',  ( 14.38125909742180930, 40.00000000000060396, -55.17850393974224232 ) ) ;
#21193 = CARTESIAN_POINT ( 'NONE',  ( -87.12760505690756929, 16.17310810899977724, 14.16732333546323730 ) ) ;
#21194 = DIRECTION ( 'NONE',  ( 1.000000000000000000, 1.836970198721030427E-16, -0.000000000000000000 ) ) ;
#21195 = CARTESIAN_POINT ( 'NONE',  ( 199.0058938177734547, 17.94521767341456098, -8.824629201450257199 ) ) ;
#21196 = CARTESIAN_POINT ( 'NONE',  ( 91.82158438592158234, 12.16597498397773869, -12.16597498397759303 ) ) ;
#21197 = CARTESIAN_POINT ( 'NONE',  ( -94.58366989427236149, 8.190486896678876860, 20.91926462023921829 ) ) ;
#21198 = VECTOR ( 'NONE', #11567, 1000.000000000000000 ) ;
#21199 =( BOUNDED_CURVE ( )  B_SPLINE_CURVE ( 3, ( #1396, #1143, #15360, #23993 ),
 .UNSPECIFIED., .F., .F. ) 
 B_SPLINE_CURVE_WITH_KNOTS ( ( 4, 4 ),
 ( 0.04745072232841010540, 0.05537094628643264571 ),
 .UNSPECIFIED. ) 
 CURVE ( )  GEOMETRIC_REPRESENTATION_ITEM ( )  RATIONAL_B_SPLINE_CURVE ( ( 0.7232313460858100784, 0.7971366613350190367, 0.8893928793064156402, 1.000000000000000000 ) ) 
 REPRESENTATION_ITEM ( '' )  );
#21200 = CARTESIAN_POINT ( 'NONE',  ( -77.90255099906772784, 8.644468104261493480, 20.04994828523958361 ) ) ;
#21201 = CARTESIAN_POINT ( 'NONE',  ( -213.1075012329537230, -9.698598906450557777, 9.698598906450415669 ) ) ;
#21202 = CARTESIAN_POINT ( 'NONE',  ( -82.26533530497846414, -10.28306516078646915, 17.41444274466569198 ) ) ;
#21203 = CARTESIAN_POINT ( 'NONE',  ( -100.7734535825088500, -40.53558337403692491, 16.03295912088671571 ) ) ;
#21204 = CARTESIAN_POINT ( 'NONE',  ( -636.3947065546303747, 29.79081638863893744, -33.73087704270072607 ) ) ;
#21205 = CARTESIAN_POINT ( 'NONE',  ( 17.75917276260965849, 24.33671690504829144, 44.20478326162346860 ) ) ;
#21206 = ORIENTED_EDGE ( 'NONE', *, *, #8097, .T. ) ;
#21207 = CARTESIAN_POINT ( 'NONE',  ( 151.7948205124836534, 4.785054706297857230, 51.78348778862544322 ) ) ;
#21208 = DIRECTION ( 'NONE',  ( 0.000000000000000000, 0.000000000000000000, 1.000000000000000000 ) ) ;
#21209 = EDGE_CURVE ( 'NONE', #23307, #13991, #702, .T. ) ;
#21210 = CARTESIAN_POINT ( 'NONE',  ( -598.4915613741692368, 40.14731501344079589, -20.33361824257625372 ) ) ;
#21211 = ORIENTED_EDGE ( 'NONE', *, *, #18927, .F. ) ;
#21212 = CARTESIAN_POINT ( 'NONE',  ( 4.995406935893306866, -39.99999999999944578, -55.24977328856505920 ) ) ;
#21213 = CARTESIAN_POINT ( 'NONE',  ( 199.0118400166160200, -7.512756401568218223, -18.53321931831850478 ) ) ;
#21214 = FACE_BOUND ( 'NONE', #21935, .T. ) ;
#21215 = ORIENTED_EDGE ( 'NONE', *, *, #7803, .F. ) ;
#21216 = ORIENTED_EDGE ( 'NONE', *, *, #12006, .T. ) ;
#21217 = ORIENTED_EDGE ( 'NONE', *, *, #26177, .F. ) ;
#21218 = CARTESIAN_POINT ( 'NONE',  ( -213.1075012329537230, 53.71589010951910836, 2.449293598294708485E-15 ) ) ;
#21219 = EDGE_CURVE ( 'NONE', #21905, #21146, #18651, .T. ) ;
#21220 = EDGE_CURVE ( 'NONE', #21839, #8490, #12804, .T. ) ;
#21221 = CARTESIAN_POINT ( 'NONE',  ( 170.0000000000000284, -19.80854622259133890, -15.47746304364911829 ) ) ;
#21222 = CIRCLE ( 'NONE', #11842, 14.99999999999999645 ) ;
#21223 = CARTESIAN_POINT ( 'NONE',  ( -77.72892396114286839, -19.09609284691637754, 10.88898768917809434 ) ) ;
#21224 = CARTESIAN_POINT ( 'NONE',  ( -259.2033419157646676, -1.438356298054549103E-14, -9.517827891722632216 ) ) ;
#21225 = CARTESIAN_POINT ( 'NONE',  ( 200.0000000000001421, -10.69674284809226350, -15.70882504007707681 ) ) ;
#21226 = DIRECTION ( 'NONE',  ( 1.000000000000000000, 1.836970198721030181E-16, 0.000000000000000000 ) ) ;
#21227 = CARTESIAN_POINT ( 'NONE',  ( -56.48582580120559271, -6.472252184284276844, 6.472252184284108978 ) ) ;
#21228 = CARTESIAN_POINT ( 'NONE',  ( 136.1360204305621266, -3.511608612531119000, 53.05693388239312469 ) ) ;
#21229 = CARTESIAN_POINT ( 'NONE',  ( -86.84962968273566730, 19.67999904273991163, 8.151722510992470916 ) ) ;
#21230 = CARTESIAN_POINT ( 'NONE',  ( 14.38125909742182529, -39.99999999999944578, -55.17850393971050238 ) ) ;
#21231 = CARTESIAN_POINT ( 'NONE',  ( 170.2234770963711128, 17.36149277826980253, 17.36149277827007253 ) ) ;
#21232 = CARTESIAN_POINT ( 'NONE',  ( -91.56559293963834989, -17.32597176626812185, -40.00000000000002132 ) ) ;
#21233 = CARTESIAN_POINT ( 'NONE',  ( -56.48582580120558561, 6.472252184283903809, 50.09629031063968796 ) ) ;
#21234 = DIRECTION ( 'NONE',  ( 0.000000000000000000, -1.000000000000000000, 0.000000000000000000 ) ) ;
#21236 = CARTESIAN_POINT ( 'NONE',  ( 91.82158438592156813, 40.00000000000009948, -17.20528682183286051 ) ) ;
#21235 = CARTESIAN_POINT ( 'NONE',  ( 192.4448373802101173, -42.42640687122053578, -14.14213562370360577 ) ) ;
#21237 = CARTESIAN_POINT ( 'NONE',  ( 192.4448373802100889, -20.00000000003938538, 0.000000000000000000 ) ) ;
#21238 = CARTESIAN_POINT ( 'NONE',  ( 91.82158438592158234, -12.16597498400057198, 44.40256751092329779 ) ) ;
#21239 = CARTESIAN_POINT ( 'NONE',  ( 146.6084372240433993, -34.62501878078303008, 0.000000000000000000 ) ) ;
#21240 = ORIENTED_EDGE ( 'NONE', *, *, #11647, .F. ) ;
#21241 = AXIS2_PLACEMENT_3D ( 'NONE', #2415, #12382, #10664 ) ;
#21242 = CARTESIAN_POINT ( 'NONE',  ( 3.468680969975848072, -48.91035688726934438, 14.11592159091329712 ) ) ;
#21243 = CARTESIAN_POINT ( 'NONE',  ( -100.7734535825088500, 17.32597176626809699, -40.00000000000002132 ) ) ;
#21244 = CARTESIAN_POINT ( 'NONE',  ( -86.86493150571114086, -8.366608963953616751, 19.60045294882772993 ) ) ;
#21245 = CARTESIAN_POINT ( 'NONE',  ( -30.26275506840323715, 29.48230279907789253, 29.48230279907799556 ) ) ;
#21246 = CARTESIAN_POINT ( 'NONE',  ( -86.96347745069644475, 5.999880687339585546E-14, -21.75974354311649961 ) ) ;
#21247 = CARTESIAN_POINT ( 'NONE',  ( -77.79205229025097879, 20.86780749215325415, -6.766653315070159103 ) ) ;
#21248 = CARTESIAN_POINT ( 'NONE',  ( -3.486753633152344989, -13.85715877881399116, -47.18604396268663947 ) ) ;
#21249 = CARTESIAN_POINT ( 'NONE',  ( 199.0252366630825520, -19.04991887513223503, 6.114737037930856545 ) ) ;
#21250 = CARTESIAN_POINT ( 'NONE',  ( -105.3755690713226585, 12.89780903124349720, 43.67073346367994446 ) ) ;
#21251 = FACE_OUTER_BOUND ( 'NONE', #15985, .T. ) ;
#21252 = DIRECTION ( 'NONE',  ( 0.000000000000000000, 1.000000000000000000, 0.000000000000000000 ) ) ;
#21253 = CARTESIAN_POINT ( 'NONE',  ( -199.0730705747436957, -18.57195860669628473, 44.83667434818101327 ) ) ;
#21254 = CARTESIAN_POINT ( 'NONE',  ( 57.59792236341147031, -1.493297263419786540E-14, 2.435789363418160658 ) ) ;
#21255 = AXIS2_PLACEMENT_3D ( 'NONE', #1757, #11856, #23964 ) ;
#21256 = CARTESIAN_POINT ( 'NONE',  ( 0.2972598230770048811, -10.13633138497510089, 66.70487387989852834 ) ) ;
#21257 = CARTESIAN_POINT ( 'NONE',  ( -77.61421004778013355, 12.97751843348148881, -17.87698779688713913 ) ) ;
#21258 = CARTESIAN_POINT ( 'NONE',  ( 192.4448373802100889, 14.14213562375873678, 14.14213562375894817 ) ) ;
#21260 = CARTESIAN_POINT ( 'NONE',  ( 19.06497207195980792, 66.60410523465830579, -10.03556273973354251 ) ) ;
#21259 = CARTESIAN_POINT ( 'NONE',  ( -91.56559293963836410, 16.03295912088692177, 16.03295912088721664 ) ) ;
#21261 = CARTESIAN_POINT ( 'NONE',  ( 0.2972598230770011618, 10.13633138497555919, -66.70487387989845729 ) ) ;
#21262 = CARTESIAN_POINT ( 'NONE',  ( 163.1118516004056573, -27.26290988616869626, -40.00000000000002132 ) ) ;
#21263 = CARTESIAN_POINT ( 'NONE',  ( 200.0000000000000000, 42.42640687119288856, -14.14213562373094746 ) ) ;
#21264 = DIRECTION ( 'NONE',  ( -1.000000000000000000, -1.836970198721030181E-16, -0.000000000000000000 ) ) ;
#21265 = CARTESIAN_POINT ( 'NONE',  ( -162.0762913951021176, -29.48230308784793152, 27.08623940707591515 ) ) ;
#21266 = DIRECTION ( 'NONE',  ( 0.000000000000000000, 1.000000000000000000, 0.000000000000000000 ) ) ;
#21267 = VERTEX_POINT ( 'NONE', #13560 ) ;
#21268 = CARTESIAN_POINT ( 'NONE',  ( 19.06497207195981147, 38.31983398719620482, 38.31983398719633271 ) ) ;
#21269 = CARTESIAN_POINT ( 'NONE',  ( -105.4741150117383057, 8.366608964593771347, 19.60045294982731789 ) ) ;
#21270 = CARTESIAN_POINT ( 'NONE',  ( -4.121597284766443714, -42.98102224344790301, -23.43330939486633824 ) ) ;
#21271 = EDGE_LOOP ( 'NONE', ( #1079, #22785, #1401, #2858, #13690, #19046, #18711, #6204 ) ) ;
#21272 = CARTESIAN_POINT ( 'NONE',  ( -114.4364955367321244, -20.04994829327305084, 8.644468109216932206 ) ) ;
#21273 = AXIS2_PLACEMENT_3D ( 'NONE', #13694, #11561, #11693 ) ;
#21274 = ADVANCED_FACE ( 'NONE', ( #11186 ), #19814, .F. ) ;
#21275 = CARTESIAN_POINT ( 'NONE',  ( 199.9999999999998863, -3.863658434880562265, -18.60611098383053630 ) ) ;
#21276 = CARTESIAN_POINT ( 'NONE',  ( 23.32574057153124869, -23.35062444423053662, 42.87194976637110244 ) ) ;
#21277 = CARTESIAN_POINT ( 'NONE',  ( 14.38125909742180752, 15.17850393972634038, -40.00000000000002132 ) ) ;
#21278 = CARTESIAN_POINT ( 'NONE',  ( 23.37394308801976806, 42.85717664514618264, -23.33966569535049373 ) ) ;
#21279 = CARTESIAN_POINT ( 'NONE',  ( 199.0176798082135008, 11.64390658120213828, 16.27508030683247497 ) ) ;
#21280 = CARTESIAN_POINT ( 'NONE',  ( -238.4067589809705794, -28.96627169325352469, 27.60227080167035041 ) ) ;
#21281 = CARTESIAN_POINT ( 'NONE',  ( 184.8905102610680444, 40.00000000000013500, -20.92133201514430141 ) ) ;
#21282 = FACE_OUTER_BOUND ( 'NONE', #13272, .T. ) ;
#21283 = DIRECTION ( 'NONE',  ( 1.000000000000000000, -1.836970198721030181E-16, -0.000000000000000000 ) ) ;
#21284 = CARTESIAN_POINT ( 'NONE',  ( 200.0000000000000000, -19.99999999999988631, -40.00000000000002132 ) ) ;
#21286 = CARTESIAN_POINT ( 'NONE',  ( -599.2626224583869998, 38.32091463456419689, 11.47750068289685821 ) ) ;
#21285 = CARTESIAN_POINT ( 'NONE',  ( 22.98934664983253029, -17.85845455615937283, -43.11412319250651137 ) ) ;
#21287 = CARTESIAN_POINT ( 'NONE',  ( 91.82158438592156813, 17.20528682183302038, 40.00000000000002132 ) ) ;
#21288 = CARTESIAN_POINT ( 'NONE',  ( 192.4448373802101173, 42.42640687122070631, 14.14213562370331623 ) ) ;
#21289 = VECTOR ( 'NONE', #12248, 1000.000000000000000 ) ;
#21290 = CARTESIAN_POINT ( 'NONE',  ( 130.8568914410475088, 39.99999999999969447, 34.05028731879830417 ) ) ;
#21291 = FACE_OUTER_BOUND ( 'NONE', #20175, .T. ) ;
#21292 = CARTESIAN_POINT ( 'NONE',  ( 151.7948205124836534, -40.00000000000034817, 33.23291073765511072 ) ) ;
#21293 = CARTESIAN_POINT ( 'NONE',  ( 199.0254609980498799, -7.058152949095585882, 18.72097443096651403 ) ) ;
#21294 = CARTESIAN_POINT ( 'NONE',  ( 144.9498910354600696, -30.13892677251539709, -12.48395222454551323 ) ) ;
#21295 = CARTESIAN_POINT ( 'NONE',  ( -259.2033419157646676, 21.55415060305790931, 35.01439189186571355 ) ) ;
#21296 = CARTESIAN_POINT ( 'NONE',  ( 0.2972598230770048811, -10.13633138497510089, 66.70487387989852834 ) ) ;
#21297 = EDGE_LOOP ( 'NONE', ( #18911, #22683, #6670, #994 ) ) ;
#21299 = CARTESIAN_POINT ( 'NONE',  ( -4.112199523539896262, 46.96527782736888668, -13.82298295336167904 ) ) ;
#21298 = FACE_OUTER_BOUND ( 'NONE', #12927, .T. ) ;
#21300 = CARTESIAN_POINT ( 'NONE',  ( 0.2972598230770129857, -54.33493731733938148, 40.00000000000002132 ) ) ;
#21301 = CARTESIAN_POINT ( 'NONE',  ( 4.995406935893289102, 10.78321810389013002, -10.78321810388986712 ) ) ;
#21302 = DIRECTION ( 'NONE',  ( 0.000000000000000000, 0.9307566067255934605, 0.3656393565204090201 ) ) ;
#21303 = CARTESIAN_POINT ( 'NONE',  ( 0.000000000000000000, 0.000000000000000000, 0.000000000000000000 ) ) ;
#21304 = ORIENTED_EDGE ( 'NONE', *, *, #18331, .T. ) ;
#21305 = ORIENTED_EDGE ( 'NONE', *, *, #9386, .T. ) ;
#21306 = CARTESIAN_POINT ( 'NONE',  ( -88.39148973765156825, 8.577159256668517529, -19.92926839984427545 ) ) ;
#21307 = CARTESIAN_POINT ( 'NONE',  ( 23.37394308801980713, -42.85717664514568526, -23.33966569535099822 ) ) ;
#21308 = B_SPLINE_CURVE_WITH_KNOTS ( 'NONE', 3,
 ( #9602, #11995, #5741, #13847, #3896, #21982 ),
 .UNSPECIFIED., .F., .F.,
 ( 4, 2, 4 ),
 ( -0.0001324603514786740893, 0.04003846212279590228, 0.08020938459707047108 ),
 .UNSPECIFIED. ) ;
#21309 = CARTESIAN_POINT ( 'NONE',  ( -94.58366989427319993, 8.190486896679173512, -20.91926462023913658 ) ) ;
#21310 = ORIENTED_EDGE ( 'NONE', *, *, #12729, .F. ) ;
#21311 = CARTESIAN_POINT ( 'NONE',  ( 199.0263429660336385, -15.25543418246514982, 12.94225785457335753 ) ) ;
#21312 = CIRCLE ( 'NONE', #20447, 20.53474504356812247 ) ;
#21313 = CARTESIAN_POINT ( 'NONE',  ( -188.2995950289363805, 23.44932284466059969, -43.00522595870931752 ) ) ;
#21314 = CARTESIAN_POINT ( 'NONE',  ( -259.2033419157646676, -35.01439189186554302, 21.55415060305832498 ) ) ;
#21315 = CIRCLE ( 'NONE', #24289, 10.00000000000000000 ) ;
#21316 = CARTESIAN_POINT ( 'NONE',  ( -100.7734535825088358, -16.03295912088706743, -16.03295912088710296 ) ) ;
#21317 = CARTESIAN_POINT ( 'NONE',  ( -192.9588430854690273, 39.99999999999980105, 54.46834944098235809 ) ) ;
#21318 = CARTESIAN_POINT ( 'NONE',  ( -199.9999999999999716, -44.86878812508714276, 24.82633483071253622 ) ) ;
#21319 = CARTESIAN_POINT ( 'NONE',  ( -726.9846540392142060, 66.50000000000009948, -66.50000000000005684 ) ) ;
#21320 = CARTESIAN_POINT ( 'NONE',  ( 151.7948205124836534, -40.00000000000034817, 33.23291073765511072 ) ) ;
#21321 = CARTESIAN_POINT ( 'NONE',  ( 192.4448373802101173, 40.00000000000026290, -19.99999999996018474 ) ) ;
#21322 = CARTESIAN_POINT ( 'NONE',  ( -77.58759120052278035, 17.31422299681156929, 13.74448509166802701 ) ) ;
#21323 = CARTESIAN_POINT ( 'NONE',  ( -192.9588430854689989, -10.23066800230756890, 10.23066800230742501 ) ) ;
#21324 = CARTESIAN_POINT ( 'NONE',  ( -199.9999999999998010, 24.82633483071100500, -44.86878812508844305 ) ) ;
#21325 = CARTESIAN_POINT ( 'NONE',  ( -188.2995950289364089, 43.00522595870987885, -23.44932284465868477 ) ) ;
#21326 = CARTESIAN_POINT ( 'NONE',  ( 104.1600437297061461, 20.63676802951782818, 8.548029200544462469 ) ) ;
#21327 = LINE ( 'NONE', #13083, #393 ) ;
#21328 = CARTESIAN_POINT ( 'NONE',  ( -362.0709805440841365, -4.857225732735059864E-14, 0.000000000000000000 ) ) ;
#21329 = CARTESIAN_POINT ( 'NONE',  ( -82.28162732581432692, -9.169756991548416281, 18.01798805100655088 ) ) ;
#21330 = AXIS2_PLACEMENT_3D ( 'NONE', #3861, #22360, #5711 ) ;
#21331 = CARTESIAN_POINT ( 'NONE',  ( 136.1360204305621551, -31.79587985999279454, 24.77266263493094911 ) ) ;
#21332 = CARTESIAN_POINT ( 'NONE',  ( -121.8281150765456147, -10.16552078725611352, -22.46071699959419732 ) ) ;
#21333 = DIRECTION ( 'NONE',  ( 0.9698969544411740751, -0.2249791741491982133, 0.09318942517732352326 ) ) ;
#21334 = EDGE_LOOP ( 'NONE', ( #18345, #20743 ) ) ;
#21335 = CARTESIAN_POINT ( 'NONE',  ( -259.2033419157646676, -6.730120644402966867, -49.83842185052038332 ) ) ;
#21336 = CARTESIAN_POINT ( 'NONE',  ( -200.0000000000000000, 66.50000000000009948, -66.50000000000005684 ) ) ;
#21337 = CARTESIAN_POINT ( 'NONE',  ( -611.2495423974685309, 32.35569666353303120, 31.28312433736698495 ) ) ;
#21338 = VERTEX_POINT ( 'NONE', #17307 ) ;
#21339 = CARTESIAN_POINT ( 'NONE',  ( 14.38125909742181818, -39.99999999999986500, -15.17850393972675604 ) ) ;
#21340 = CARTESIAN_POINT ( 'NONE',  ( 199.0206683190968135, -19.03253901574858986, -6.320310628391184515 ) ) ;
#21341 = CARTESIAN_POINT ( 'NONE',  ( 23.37394308801977871, -42.85717664514601921, 23.33966569535066071 ) ) ;
#21342 = ORIENTED_EDGE ( 'NONE', *, *, #19154, .F. ) ;
#21343 = VERTEX_POINT ( 'NONE', #1468 ) ;
#21344 = CARTESIAN_POINT ( 'NONE',  ( 200.0000000000000000, 19.99999999999995737, 40.00000000000002132 ) ) ;
#21345 = UNCERTAINTY_MEASURE_WITH_UNIT (LENGTH_MEASURE( 1.000000000000000082E-05 ), #8933, 'distance_accuracy_value', 'NONE');
#21346 = CARTESIAN_POINT ( 'NONE',  ( -135.8532207217289738, 6.472252184284186249, -6.472252184284142729 ) ) ;
#21347 = LINE ( 'NONE', #3117, #7437 ) ;
#21348 = AXIS2_PLACEMENT_3D ( 'NONE', #4458, #21080, #2453 ) ;
#21349 = EDGE_CURVE ( 'NONE', #20872, #23006, #12390, .T. ) ;
#21350 = CARTESIAN_POINT ( 'NONE',  ( -77.61378591600585253, -12.98772233503525619, 17.87002798532632042 ) ) ;
#21351 =( BOUNDED_SURFACE ( )  B_SPLINE_SURFACE ( 3, 3, ( 
 ( #21570, #23566, #10957, #1097, #23193, #11200, #4974, #25579, #15566, #9457, #13451, #19063, #846, #5219, #19567, #13081, #7202, #21443, #1227, #7325, #21196, #2968, #3343, #17563, #11079, #15439, #5341, #19193, #976, #11444 ),
 ( #16235, #20236, #9719, #1744, #25835, #5726, #24363, #7978, #13830, #1614, #22237, #13967, #7840, #1879, #17822, #6, #15962, #11573, #6001, #16096, #7579, #9983, #15691, #24087, #18094, #7710, #15821, #6127, #23950, #5861 ),
 ( #10119, #14108, #20102, #21963, #22102, #13705, #4012, #11707, #12111, #2017, #18220, #3737, #11840, #9852, #3877, #8118, #24227, #3475, #19961, #17691, #25970, #23816, #26243, #14235, #19692, #1480, #9586, #5598, #11978, #21829 ),
 ( #17955, #3599, #26102, #19828, #546, #4542, #18895, #12638, #14762, #16896, #10652, #22891, #12246, #142, #8245, #8783, #12773, #2271, #20628, #18362, #24626, #25028, #8650, #6383, #20499, #4671, #6514, #410, #20765, #10380 ),
 ( #20368, #18490, #271, #2678, #16501, #6781, #22375, #2535, #8513, #2142, #16632, #10253, #14625, #12500, #10513, #10785, #6647, #18762, #14500, #24761, #6258, #20900, #4281, #22762, #4151, #674, #16363, #24497, #14371, #16758 ),
 ( #22504, #12371, #24892, #8379, #22631, #2402, #4406, #18627, #9048, #21027, #23413, #19155, #19030, #25669, #13043, #23286, #939, #809, #11165, #17153, #6911, #9424, #12910, #25287, #14893, #25418, #15028, #1064, #21288, #2808 ),
 ( #11044, #7044, #23534, #3186, #11411, #3063, #9301, #8915, #17284, #10919, #15161, #23033, #7167, #23158, #9171, #19281, #17024, #5305, #4808, #25160, #4935, #19412, #5190, #13292, #19533, #5062, #21161, #13168, #17405, #13416 ) ),
 .UNSPECIFIED., .T., .F., .T. ) 
 B_SPLINE_SURFACE_WITH_KNOTS ( ( 4, 3, 4 ),
 ( 4, 2, 2, 2, 2, 2, 2, 2, 2, 2, 2, 2, 2, 2, 4 ),
 ( 0.000000000000000000, 0.5000000000000000000, 1.000000000000000000 ),
 ( 0.000000000000000000, 0.1357259735107005372, 0.1651108541090157700, 0.1944957347073310028, 0.3598804999793158710, 0.3867117631979620773, 0.4135430264166082281, 0.5789277916885930964, 0.6062785021374117456, 0.6336292125862302838, 0.8508620842112317728, 0.8814014469398914198, 0.9119408096685510667, 0.9559704048342755334, 1.000000000000000000 ),
 .UNSPECIFIED. ) 
 GEOMETRIC_REPRESENTATION_ITEM ( )  RATIONAL_B_SPLINE_SURFACE ( (
 ( 1.000000000000000000, 1.000000000000000000, 1.000000000000000000, 1.000000000000000000, 1.000000000000000000, 1.000000000000000000, 1.000000000000000000, 1.000000000000000000, 1.000000000000000000, 1.000000000000000000, 1.000000000000000000, 1.000000000000000000, 1.000000000000000000, 1.000000000000000000, 1.000000000000000000, 1.000000000000000000, 1.000000000000000000, 1.000000000000000000, 1.000000000000000000, 1.000000000000000000, 1.000000000000000000, 1.000000000000000000, 1.000000000000000000, 1.000000000000000000, 1.000000000000000000, 1.000000000000000000, 1.000000000000000000, 1.000000000000000000, 1.000000000000000000, 1.000000000000000000),
 ( 0.3333333333333333703, 0.3333333333333333703, 0.3333333333333333703, 0.3333333333333333703, 0.3333333333333333703, 0.3333333333333333703, 0.3333333333333333703, 0.3333333333333333703, 0.3333333333333333703, 0.3333333333333333703, 0.3333333333333333703, 0.3333333333333333703, 0.3333333333333333703, 0.3333333333333333703, 0.3333333333333333703, 0.3333333333333333703, 0.3333333333333333703, 0.3333333333333333703, 0.3333333333333333703, 0.3333333333333333703, 0.3333333333333333703, 0.3333333333333333703, 0.3333333333333333703, 0.3333333333333333703, 0.3333333333333333703, 0.3333333333333333703, 0.3333333333333333703, 0.3333333333333333703, 0.3333333333333333703, 0.3333333333333333703),
 ( 0.3333333333333333703, 0.3333333333333333703, 0.3333333333333333703, 0.3333333333333333703, 0.3333333333333333703, 0.3333333333333333703, 0.3333333333333333703, 0.3333333333333333703, 0.3333333333333333703, 0.3333333333333333703, 0.3333333333333333703, 0.3333333333333333703, 0.3333333333333333703, 0.3333333333333333703, 0.3333333333333333703, 0.3333333333333333703, 0.3333333333333333703, 0.3333333333333333703, 0.3333333333333333703, 0.3333333333333333703, 0.3333333333333333703, 0.3333333333333333703, 0.3333333333333333703, 0.3333333333333333703, 0.3333333333333333703, 0.3333333333333333703, 0.3333333333333333703, 0.3333333333333333703, 0.3333333333333333703, 0.3333333333333333703),
 ( 1.000000000000000000, 1.000000000000000000, 1.000000000000000000, 1.000000000000000000, 1.000000000000000000, 1.000000000000000000, 1.000000000000000000, 1.000000000000000000, 1.000000000000000000, 1.000000000000000000, 1.000000000000000000, 1.000000000000000000, 1.000000000000000000, 1.000000000000000000, 1.000000000000000000, 1.000000000000000000, 1.000000000000000000, 1.000000000000000000, 1.000000000000000000, 1.000000000000000000, 1.000000000000000000, 1.000000000000000000, 1.000000000000000000, 1.000000000000000000, 1.000000000000000000, 1.000000000000000000, 1.000000000000000000, 1.000000000000000000, 1.000000000000000000, 1.000000000000000000),
 ( 0.3333333333333333703, 0.3333333333333333703, 0.3333333333333333703, 0.3333333333333333703, 0.3333333333333333703, 0.3333333333333333703, 0.3333333333333333703, 0.3333333333333333703, 0.3333333333333333703, 0.3333333333333333703, 0.3333333333333333703, 0.3333333333333333703, 0.3333333333333333703, 0.3333333333333333703, 0.3333333333333333703, 0.3333333333333333703, 0.3333333333333333703, 0.3333333333333333703, 0.3333333333333333703, 0.3333333333333333703, 0.3333333333333333703, 0.3333333333333333703, 0.3333333333333333703, 0.3333333333333333703, 0.3333333333333333703, 0.3333333333333333703, 0.3333333333333333703, 0.3333333333333333703, 0.3333333333333333703, 0.3333333333333333703),
 ( 0.3333333333333333703, 0.3333333333333333703, 0.3333333333333333703, 0.3333333333333333703, 0.3333333333333333703, 0.3333333333333333703, 0.3333333333333333703, 0.3333333333333333703, 0.3333333333333333703, 0.3333333333333333703, 0.3333333333333333703, 0.3333333333333333703, 0.3333333333333333703, 0.3333333333333333703, 0.3333333333333333703, 0.3333333333333333703, 0.3333333333333333703, 0.3333333333333333703, 0.3333333333333333703, 0.3333333333333333703, 0.3333333333333333703, 0.3333333333333333703, 0.3333333333333333703, 0.3333333333333333703, 0.3333333333333333703, 0.3333333333333333703, 0.3333333333333333703, 0.3333333333333333703, 0.3333333333333333703, 0.3333333333333333703),
 ( 1.000000000000000000, 1.000000000000000000, 1.000000000000000000, 1.000000000000000000, 1.000000000000000000, 1.000000000000000000, 1.000000000000000000, 1.000000000000000000, 1.000000000000000000, 1.000000000000000000, 1.000000000000000000, 1.000000000000000000, 1.000000000000000000, 1.000000000000000000, 1.000000000000000000, 1.000000000000000000, 1.000000000000000000, 1.000000000000000000, 1.000000000000000000, 1.000000000000000000, 1.000000000000000000, 1.000000000000000000, 1.000000000000000000, 1.000000000000000000, 1.000000000000000000, 1.000000000000000000, 1.000000000000000000, 1.000000000000000000, 1.000000000000000000, 1.000000000000000000) ) ) 
 REPRESENTATION_ITEM ( '' )  SURFACE ( )  );
#21352 = CARTESIAN_POINT ( 'NONE',  ( -105.2054292635175727, 15.19799821370213522, 15.19799821370241943 ) ) ;
#21353 = CARTESIAN_POINT ( 'NONE',  ( 200.0000000000001421, -12.54320094651582451, -14.29122475987005458 ) ) ;
#21354 = ADVANCED_FACE ( 'NONE', ( #19302 ), #9446, .T. ) ;
#21355 = CARTESIAN_POINT ( 'NONE',  ( -87.11181970786255135, 13.17799186809413392, 17.01573394368394077 ) ) ;
#21356 = CARTESIAN_POINT ( 'NONE',  ( -70.33906594972403070, -9.443630401875100944, -22.79894061986596654 ) ) ;
#21357 = CARTESIAN_POINT ( 'NONE',  ( 57.59792236341147031, 1.722363176415040886, 1.722363176415060426 ) ) ;
#21358 = CARTESIAN_POINT ( 'NONE',  ( -105.4741150117382631, -19.60045294982879582, -8.366608964590131592 ) ) ;
#21359 = CARTESIAN_POINT ( 'NONE',  ( 163.1118516004056573, -39.99999999999986500, -12.73709011382517353 ) ) ;
#21360 = FACE_OUTER_BOUND ( 'NONE', #1245, .T. ) ;
#21361 = CARTESIAN_POINT ( 'NONE',  ( -86.96347745069643054, -18.24025645688353947, -40.00000000000002132 ) ) ;
#21362 = EDGE_CURVE ( 'NONE', #22617, #7462, #65, .T. ) ;
#21363 = EDGE_CURVE ( 'NONE', #9502, #19805, #21814, .T. ) ;
#21364 = CARTESIAN_POINT ( 'NONE',  ( 57.59792236341148453, -26.56190807104700369, 26.56190807104673723 ) ) ;
#21365 = CARTESIAN_POINT ( 'NONE',  ( -100.7734535825088500, -17.32597176626812185, -40.00000000000002132 ) ) ;
#21367 = CARTESIAN_POINT ( 'NONE',  ( -162.0762913951020892, -3.568845385355699554E-14, 1.694272876828323948 ) ) ;
#21366 = CARTESIAN_POINT ( 'NONE',  ( -110.0305071378944319, 18.66378802528556946, 7.635428997630903325 ) ) ;
#21368 = CARTESIAN_POINT ( 'NONE',  ( -86.96347745069644475, -21.75974354311652093, -40.00000000000002132 ) ) ;
#21369 = CARTESIAN_POINT ( 'NONE',  ( -162.0762913951020892, 57.76657433537918251, 1.198031840455469066 ) ) ;
#21370 = CARTESIAN_POINT ( 'NONE',  ( -30.26275506840324425, 41.69427246844628598, -40.00000000000002132 ) ) ;
#21371 = VERTEX_POINT ( 'NONE', #21431 ) ;
#21372 = CARTESIAN_POINT ( 'NONE',  ( 22.90311673803729420, -42.99920082299467339, 23.44499648834695549 ) ) ;
#21373 = CARTESIAN_POINT ( 'NONE',  ( -83.21262154144248768, 13.72187187061550695, -33.12752917118394436 ) ) ;
#21374 = CARTESIAN_POINT ( 'NONE',  ( 146.6084372240433709, -52.76785682606516303, 3.800685668858563737 ) ) ;
#21375 = CARTESIAN_POINT ( 'NONE',  ( -56.48582580120558561, -40.00000000000000000, -9.153146818113723882 ) ) ;
#21376 = DIRECTION ( 'NONE',  ( 1.000000000000000000, 1.836970198721030181E-16, 0.000000000000000000 ) ) ;
#21377 = CARTESIAN_POINT ( 'NONE',  ( -70.30307074931239697, 8.711708294051453194, -23.14841682951314894 ) ) ;
#21378 = CARTESIAN_POINT ( 'NONE',  ( 200.0000000000001421, -0.6349535514222880428, 19.00853270881595591 ) ) ;
#21379 = CARTESIAN_POINT ( 'NONE',  ( -642.1214326342156937, 30.47265398018172888, -25.91871900570560783 ) ) ;
#21380 = DIRECTION ( 'NONE',  ( 1.000000000000000000, 1.836970198721025990E-16, 0.000000000000000000 ) ) ;
#21381 = CARTESIAN_POINT ( 'NONE',  ( 146.6084372240433709, 3.800685668858042821, 52.76785682606522698 ) ) ;
#21382 = CARTESIAN_POINT ( 'NONE',  ( -86.96347745069645896, 43.67073346367988762, -12.89780903124366418 ) ) ;
#21383 = CARTESIAN_POINT ( 'NONE',  ( 57.59792236341148453, 1.722363176414758668, 54.84617931850880268 ) ) ;
#21384 = CARTESIAN_POINT ( 'NONE',  ( -362.0709805440841365, -4.857225732735059864E-14, 20.53474504356812247 ) ) ;
#21385 = CARTESIAN_POINT ( 'NONE',  ( -259.2033419157646676, 6.730120644403426944, 6.730120644403592145 ) ) ;
#21387 = CARTESIAN_POINT ( 'NONE',  ( 136.1360204305621551, -53.05693388239309627, -3.511608612531332163 ) ) ;
#21386 = CARTESIAN_POINT ( 'NONE',  ( 14.38125909742180752, 17.55144818341503665, -39.01709431150898411 ) ) ;
#21388 = CARTESIAN_POINT ( 'NONE',  ( 184.8905102610680444, 13.49065550809826952, -13.49065550809790359 ) ) ;
#21389 = CARTESIAN_POINT ( 'NONE',  ( -135.8532207217289738, -9.153146818113595984, 0.000000000000000000 ) ) ;
#21390 = DIRECTION ( 'NONE',  ( 0.000000000000000000, 0.000000000000000000, -1.000000000000000000 ) ) ;
#21391 = CARTESIAN_POINT ( 'NONE',  ( -100.7734535825088358, 6.065416334915073333E-14, -22.67402823373191723 ) ) ;
#21392 = CARTESIAN_POINT ( 'NONE',  ( -105.3755690713226585, -41.18208027870611687, 15.38646221621750954 ) ) ;
#21393 = CARTESIAN_POINT ( 'NONE',  ( -166.7090608787311226, 37.06260950144081079, -15.35183551249070533 ) ) ;
#21394 = ORIENTED_EDGE ( 'NONE', *, *, #8145, .T. ) ;
#21395 = CARTESIAN_POINT ( 'NONE',  ( 151.7948205124836534, 33.06932595376365924, -23.49921654116018743 ) ) ;
#21396 = CARTESIAN_POINT ( 'NONE',  ( -97.72675010090327419, -20.89622088363361385, -8.185591577777390881 ) ) ;
#21397 = CARTESIAN_POINT ( 'NONE',  ( 22.13784119382970061, 17.95298715833905234, 43.34234508276811937 ) ) ;
#21398 = CARTESIAN_POINT ( 'NONE',  ( -86.95493927446905502, -20.33927854521762058, 6.698173996902891503 ) ) ;
#21399 = VERTEX_POINT ( 'NONE', #5586 ) ;
#21400 = CARTESIAN_POINT ( 'NONE',  ( -129.2303492451636941, -24.84170067260939874, 11.67678589703593772 ) ) ;
#21401 = CARTESIAN_POINT ( 'NONE',  ( 199.9999999999998863, -11.20618975336454071, -15.34975362513495689 ) ) ;
#21402 = CARTESIAN_POINT ( 'NONE',  ( 23.72853009152683157, -13.77482773664794458, 46.68009952139140495 ) ) ;
#21403 = CARTESIAN_POINT ( 'NONE',  ( 169.9999999999999716, -15.47746304364925329, 19.80854622259126430 ) ) ;
#21404 = CARTESIAN_POINT ( 'NONE',  ( 199.0071786209885261, 3.739031945787267386, -19.64359944086908527 ) ) ;
#21405 = CARTESIAN_POINT ( 'NONE',  ( -87.10405235694547343, 21.30065104412373245, 2.801403629797663442 ) ) ;
#21406 = CARTESIAN_POINT ( 'NONE',  ( 14.38125909742180220, 39.99999999999997158, 15.17850393972647716 ) ) ;
#21407 = CARTESIAN_POINT ( 'NONE',  ( 19.06497207195981147, -4.605042221739098431E-14, 14.19242893257840521 ) ) ;
#21408 = CARTESIAN_POINT ( 'NONE',  ( -200.0000000000001705, -23.83166235904677777, -44.86667451853072919 ) ) ;
#21409 = CARTESIAN_POINT ( 'NONE',  ( 4.995406935893307754, -55.24977328853207581, -40.00000000000002132 ) ) ;
#21411 = CARTESIAN_POINT ( 'NONE',  ( -200.0000000000000000, 52.50000000000007816, 52.49999999999999289 ) ) ;
#21410 = CARTESIAN_POINT ( 'NONE',  ( 20.17262239841839389, -18.14389419515046242, -43.80323544018617099 ) ) ;
#21412 = CARTESIAN_POINT ( 'NONE',  ( 14.38125909742182884, -55.17850393971007605, 40.00000000000002132 ) ) ;
#21413 = CARTESIAN_POINT ( 'NONE',  ( -238.4067589809705794, -0.9644942799826262680, 0.000000000000000000 ) ) ;
#21414 = CARTESIAN_POINT ( 'NONE',  ( 57.59792236341147031, 40.00000000000042633, -37.56421063658144277 ) ) ;
#21415 = CARTESIAN_POINT ( 'NONE',  ( -238.4067589809705794, -39.99999999999963762, -40.96449428006383187 ) ) ;
#21416 = EDGE_CURVE ( 'NONE', #23676, #19014, #6154, .T. ) ;
#21417 = CARTESIAN_POINT ( 'NONE',  ( 167.0465517065776737, -23.44217192942191730, -9.710065544648454505 ) ) ;
#21418 = VERTEX_POINT ( 'NONE', #17809 ) ;
#21420 = CARTESIAN_POINT ( 'NONE',  ( 15.76057515052796276, 44.53539632572124418, -18.44716516378320037 ) ) ;
#21419 = CARTESIAN_POINT ( 'NONE',  ( 19.06497207195981147, -10.03556273973425483, -10.03556273973443247 ) ) ;
#21421 = CARTESIAN_POINT ( 'NONE',  ( 163.1118516004056573, -12.73709011382472589, 40.00000000000002132 ) ) ;
#21422 = CARTESIAN_POINT ( 'NONE',  ( -198.9234529668597986, 49.24835336344366965, -14.16707775654091606 ) ) ;
#21423 = CARTESIAN_POINT ( 'NONE',  ( 0.000000000000000000, 0.000000000000000000, 0.000000000000000000 ) ) ;
#21424 = ORIENTED_EDGE ( 'NONE', *, *, #12719, .T. ) ;
#21425 = ORIENTED_EDGE ( 'NONE', *, *, #6153, .T. ) ;
#21426 = CARTESIAN_POINT ( 'NONE',  ( -135.8532207217289738, 6.472252184284186249, -6.472252184284142729 ) ) ;
#21427 = CARTESIAN_POINT ( 'NONE',  ( 144.9504669809064126, 12.48392651407853471, -30.13886470195694400 ) ) ;
#21428 = ORIENTED_EDGE ( 'NONE', *, *, #3781, .T. ) ;
#21429 = ORIENTED_EDGE ( 'NONE', *, *, #19081, .T. ) ;
#21430 = CARTESIAN_POINT ( 'NONE',  ( 199.9999999999998863, -9.643221244315762775, 16.38360543750208009 ) ) ;
#21431 = CARTESIAN_POINT ( 'NONE',  ( 169.9999999999999716, -125.7889608577475400, -82.49999999999998579 ) ) ;
#21432 = EDGE_CURVE ( 'NONE', #26151, #2862, #23432, .T. ) ;
#21433 = CARTESIAN_POINT ( 'NONE',  ( 146.6084372240433993, 3.800685668858676980, 3.800685668858667210 ) ) ;
#21434 = CARTESIAN_POINT ( 'NONE',  ( -121.8281150760332991, -23.07023398566525074, -8.694016612792475840 ) ) ;
#21435 = CARTESIAN_POINT ( 'NONE',  ( 57.59792236341147031, 1.908507979671054758E-14, -2.435789363418160658 ) ) ;
#21436 = CARTESIAN_POINT ( 'NONE',  ( 21.15358250000287654, -13.91686544622502097, 47.58740525742008032 ) ) ;
#21437 = CYLINDRICAL_SURFACE ( 'NONE', #5471, 10.00000000000000000 ) ;
#21438 = CARTESIAN_POINT ( 'NONE',  ( 0.2972598230770030492, -39.99999999999987210, -14.33493731733975451 ) ) ;
#21439 = CARTESIAN_POINT ( 'NONE',  ( 200.0000000000000000, 40.00000000000026290, -19.99999999999950617 ) ) ;
#21440 = CARTESIAN_POINT ( 'NONE',  ( -82.24986055077694402, 16.41205588405924942, 11.76386043655782032 ) ) ;
#21441 = CARTESIAN_POINT ( 'NONE',  ( 199.9999999999999432, 14.14213562373113398, -14.14213562373094923 ) ) ;
#21442 = CARTESIAN_POINT ( 'NONE',  ( 130.8568914410475372, 1.429239637432775288E-13, -34.05028731879788495 ) ) ;
#21443 = CARTESIAN_POINT ( 'NONE',  ( 14.38125909742181285, -10.73282306404727393, 10.73282306404716380 ) ) ;
#21444 = CARTESIAN_POINT ( 'NONE',  ( 118.9130007099547299, 25.80693111732287548, 10.68958087202344664 ) ) ;
#21445 = EDGE_CURVE ( 'NONE', #17458, #22617, #7099, .T. ) ;
#21446 = CARTESIAN_POINT ( 'NONE',  ( 98.29820294271928560, -12.26677183925107428, -16.01749940821211382 ) ) ;
#21447 = CARTESIAN_POINT ( 'NONE',  ( 14.38125909742181285, -10.73282306404727393, 10.73282306404716380 ) ) ;
#21448 = CARTESIAN_POINT ( 'NONE',  ( -82.25988539630567686, -17.04081484590923168, 10.82485991172919526 ) ) ;
#21449 = CARTESIAN_POINT ( 'NONE',  ( 19.06497207195981858, 10.03556273973424062, 66.60410523465820631 ) ) ;
#21450 =( BOUNDED_SURFACE ( )  B_SPLINE_SURFACE ( 3, 3, ( 
 ( #638, #2903, #24854, #20989, #24993, #14726, #8878, #6745, #4635, #7135, #18721, #14857, #12601, #23124, #12736, #2638, #2771, #22992, #10880, #10747, #19120, #9130, #903, #18858, #5028, #25250, #22858, #772, #506, #13136 ),
 ( #8743, #8612, #16988, #4768, #25124, #17245, #14990, #25383, #9015, #17120, #15249, #23379, #21382, #13761, #25764, #11773, #25510, #19892, #1281, #9782, #15622, #3278, #17373, #21758, #13259, #5404, #7770, #9389, #11376, #3154 ),
 ( #13504, #19497, #21626, #5154, #3402, #5274, #11504, #23624, #19628, #1413, #17884, #23745, #3665, #17496, #11255, #11632, #9514, #26033, #23500, #15751, #21888, #5526, #1677, #25637, #15885, #19374, #23879, #13633, #1161, #17754 ),
 ( #9265, #7259, #15377, #13379, #17619, #7514, #21506, #3531, #7383, #19754, #15494, #1544, #9649, #25895, #7635, #5656, #1942, #18019, #6315, #18424, #5929, #1810, #24423, #14435, #8311, #24297, #22436, #20430, #3805, #10050 ),
 ( #16434, #22564, #4213, #12041, #16299, #9913, #6065, #18156, #26168, #20299, #26303, #16027, #18561, #22032, #8046, #24011, #8182, #24152, #14036, #14167, #16162, #22300, #22170, #14302, #12435, #6189, #3944, #202, #10318, #7908 ),
 ( #4077, #8444, #11909, #20161, #20032, #12178, #2076, #10183, #4343, #18287, #24560, #73, #5791, #2209, #12303, #13899, #20563, #2334, #10448, #340, #5002, #12703, #21228, #746, #14698, #2467, #6846, #24693, #16831, #19223 ),
 ( #875, #24966, #6713, #14827, #4607, #22959, #16563, #4738, #16693, #12846, #8715, #20962, #2743, #3000, #8850, #15090, #22830, #6448, #23099, #10847, #11107, #8582, #8986, #6976, #16960, #13107, #20831, #23224, #14564, #17091 ) ),
 .UNSPECIFIED., .T., .F., .T. ) 
 B_SPLINE_SURFACE_WITH_KNOTS ( ( 4, 3, 4 ),
 ( 4, 2, 2, 2, 2, 2, 2, 2, 2, 2, 2, 2, 2, 2, 4 ),
 ( 0.000000000000000000, 0.5000000000000000000, 1.000000000000000000 ),
 ( 0.000000000000000000, 0.1357259735107005372, 0.1651108541090157700, 0.1944957347073310028, 0.3598804999793158710, 0.3867117631979620773, 0.4135430264166082281, 0.5789277916885930964, 0.6062785021374117456, 0.6336292125862302838, 0.8508620842112317728, 0.8814014469398914198, 0.9119408096685510667, 0.9559704048342755334, 1.000000000000000000 ),
 .UNSPECIFIED. ) 
 GEOMETRIC_REPRESENTATION_ITEM ( )  RATIONAL_B_SPLINE_SURFACE ( (
 ( 1.000000000000000000, 1.000000000000000000, 1.000000000000000000, 1.000000000000000000, 1.000000000000000000, 1.000000000000000000, 1.000000000000000000, 1.000000000000000000, 1.000000000000000000, 1.000000000000000000, 1.000000000000000000, 1.000000000000000000, 1.000000000000000000, 1.000000000000000000, 1.000000000000000000, 1.000000000000000000, 1.000000000000000000, 1.000000000000000000, 1.000000000000000000, 1.000000000000000000, 1.000000000000000000, 1.000000000000000000, 1.000000000000000000, 1.000000000000000000, 1.000000000000000000, 1.000000000000000000, 1.000000000000000000, 1.000000000000000000, 1.000000000000000000, 1.000000000000000000),
 ( 0.3333333333333333703, 0.3333333333333333703, 0.3333333333333333703, 0.3333333333333333703, 0.3333333333333333703, 0.3333333333333333703, 0.3333333333333333703, 0.3333333333333333703, 0.3333333333333333703, 0.3333333333333333703, 0.3333333333333333703, 0.3333333333333333703, 0.3333333333333333703, 0.3333333333333333703, 0.3333333333333333703, 0.3333333333333333703, 0.3333333333333333703, 0.3333333333333333703, 0.3333333333333333703, 0.3333333333333333703, 0.3333333333333333703, 0.3333333333333333703, 0.3333333333333333703, 0.3333333333333333703, 0.3333333333333333703, 0.3333333333333333703, 0.3333333333333333703, 0.3333333333333333703, 0.3333333333333333703, 0.3333333333333333703),
 ( 0.3333333333333333703, 0.3333333333333333703, 0.3333333333333333703, 0.3333333333333333703, 0.3333333333333333703, 0.3333333333333333703, 0.3333333333333333703, 0.3333333333333333703, 0.3333333333333333703, 0.3333333333333333703, 0.3333333333333333703, 0.3333333333333333703, 0.3333333333333333703, 0.3333333333333333703, 0.3333333333333333703, 0.3333333333333333703, 0.3333333333333333703, 0.3333333333333333703, 0.3333333333333333703, 0.3333333333333333703, 0.3333333333333333703, 0.3333333333333333703, 0.3333333333333333703, 0.3333333333333333703, 0.3333333333333333703, 0.3333333333333333703, 0.3333333333333333703, 0.3333333333333333703, 0.3333333333333333703, 0.3333333333333333703),
 ( 1.000000000000000000, 1.000000000000000000, 1.000000000000000000, 1.000000000000000000, 1.000000000000000000, 1.000000000000000000, 1.000000000000000000, 1.000000000000000000, 1.000000000000000000, 1.000000000000000000, 1.000000000000000000, 1.000000000000000000, 1.000000000000000000, 1.000000000000000000, 1.000000000000000000, 1.000000000000000000, 1.000000000000000000, 1.000000000000000000, 1.000000000000000000, 1.000000000000000000, 1.000000000000000000, 1.000000000000000000, 1.000000000000000000, 1.000000000000000000, 1.000000000000000000, 1.000000000000000000, 1.000000000000000000, 1.000000000000000000, 1.000000000000000000, 1.000000000000000000),
 ( 0.3333333333333333703, 0.3333333333333333703, 0.3333333333333333703, 0.3333333333333333703, 0.3333333333333333703, 0.3333333333333333703, 0.3333333333333333703, 0.3333333333333333703, 0.3333333333333333703, 0.3333333333333333703, 0.3333333333333333703, 0.3333333333333333703, 0.3333333333333333703, 0.3333333333333333703, 0.3333333333333333703, 0.3333333333333333703, 0.3333333333333333703, 0.3333333333333333703, 0.3333333333333333703, 0.3333333333333333703, 0.3333333333333333703, 0.3333333333333333703, 0.3333333333333333703, 0.3333333333333333703, 0.3333333333333333703, 0.3333333333333333703, 0.3333333333333333703, 0.3333333333333333703, 0.3333333333333333703, 0.3333333333333333703),
 ( 0.3333333333333333703, 0.3333333333333333703, 0.3333333333333333703, 0.3333333333333333703, 0.3333333333333333703, 0.3333333333333333703, 0.3333333333333333703, 0.3333333333333333703, 0.3333333333333333703, 0.3333333333333333703, 0.3333333333333333703, 0.3333333333333333703, 0.3333333333333333703, 0.3333333333333333703, 0.3333333333333333703, 0.3333333333333333703, 0.3333333333333333703, 0.3333333333333333703, 0.3333333333333333703, 0.3333333333333333703, 0.3333333333333333703, 0.3333333333333333703, 0.3333333333333333703, 0.3333333333333333703, 0.3333333333333333703, 0.3333333333333333703, 0.3333333333333333703, 0.3333333333333333703, 0.3333333333333333703, 0.3333333333333333703),
 ( 1.000000000000000000, 1.000000000000000000, 1.000000000000000000, 1.000000000000000000, 1.000000000000000000, 1.000000000000000000, 1.000000000000000000, 1.000000000000000000, 1.000000000000000000, 1.000000000000000000, 1.000000000000000000, 1.000000000000000000, 1.000000000000000000, 1.000000000000000000, 1.000000000000000000, 1.000000000000000000, 1.000000000000000000, 1.000000000000000000, 1.000000000000000000, 1.000000000000000000, 1.000000000000000000, 1.000000000000000000, 1.000000000000000000, 1.000000000000000000, 1.000000000000000000, 1.000000000000000000, 1.000000000000000000, 1.000000000000000000, 1.000000000000000000, 1.000000000000000000) ) ) 
 REPRESENTATION_ITEM ( '' )  SURFACE ( )  );
#21451 = CARTESIAN_POINT ( 'NONE',  ( 4.995406935893312195, -67.35176059882525124, -10.78321810390210445 ) ) ;
#21452 = CARTESIAN_POINT ( 'NONE',  ( -652.3345777734953117, 37.97727100629618491, -24.15733517944065412 ) ) ;
#21453 = CARTESIAN_POINT ( 'NONE',  ( -109.1264249741456211, -33.12752917268984731, 13.72187187124577434 ) ) ;
#21454 = ORIENTED_EDGE ( 'NONE', *, *, #4933, .T. ) ;
#21455 = CARTESIAN_POINT ( 'NONE',  ( -208.1127848780265026, 38.89260858015777700, -38.89260858015687461 ) ) ;
#21456 = DIRECTION ( 'NONE',  ( -0.7071067811865549002, 0.000000000000000000, 0.7071067811865401342 ) ) ;
#21457 = DIRECTION ( 'NONE',  ( -1.000000000000000000, -0.000000000000000000, -0.000000000000000000 ) ) ;
#21458 = ORIENTED_EDGE ( 'NONE', *, *, #16287, .T. ) ;
#21459 = CARTESIAN_POINT ( 'NONE',  ( -210.0000000000000284, 71.50000000000011369, -66.50000000000005684 ) ) ;
#21460 = CARTESIAN_POINT ( 'NONE',  ( 199.0255849842728253, -18.49502280213427952, 7.623850636981702955 ) ) ;
#21461 = FACE_OUTER_BOUND ( 'NONE', #17390, .T. ) ;
#21462 = ORIENTED_EDGE ( 'NONE', *, *, #1668, .T. ) ;
#21463 = ORIENTED_EDGE ( 'NONE', *, *, #5754, .T. ) ;
#21464 = CARTESIAN_POINT ( 'NONE',  ( -135.8532207217289738, 39.99999999999989342, 30.84685318188660474 ) ) ;
#21465 = MECHANICAL_DESIGN_GEOMETRIC_PRESENTATION_REPRESENTATION (  '', ( #15717 ), #222 ) ;
#21466 = CARTESIAN_POINT ( 'NONE',  ( -726.9846540392142060, 82.50000000000008527, -52.49999999999977973 ) ) ;
#21467 = CARTESIAN_POINT ( 'NONE',  ( -280.0000000000000000, 1.839446121267387017E-14, -20.00000000000001421 ) ) ;
#21468 = CARTESIAN_POINT ( 'NONE',  ( 199.9999999999999147, -13.65919145721374761, -13.21838778087559518 ) ) ;
#21469 = AXIS2_PLACEMENT_3D ( 'NONE', #8172, #16286, #20555 ) ;
#21470 = AXIS2_PLACEMENT_3D ( 'NONE', #24538, #20673, #6294 ) ;
#21471 = B_SPLINE_CURVE_WITH_KNOTS ( 'NONE', 3,
 ( #7486, #21733, #15597, #19603, #13353, #17471, #22006, #3776 ),
 .UNSPECIFIED., .F., .F.,
 ( 4, 2, 2, 4 ),
 ( 0.008473926331994447239, 0.01052499632799544851, 0.01257606632399645152, 0.01667820631599845754 ),
 .UNSPECIFIED. ) ;
#21472 = CARTESIAN_POINT ( 'NONE',  ( -77.90255099906777048, 8.644468104261289199, 20.04994828523966177 ) ) ;
#21473 = CARTESIAN_POINT ( 'NONE',  ( 136.1360204305621266, -24.77266263493151044, 24.77266263493093135 ) ) ;
#21474 = CARTESIAN_POINT ( 'NONE',  ( 91.82158438592159655, 12.16597498400091304, -44.40256751092321963 ) ) ;
#21475 = CARTESIAN_POINT ( 'NONE',  ( -210.0000000000000284, 75.52305771588336825, -68.47933392563552957 ) ) ;
#21476 = CARTESIAN_POINT ( 'NONE',  ( -56.48582580120557850, -39.99999999999970868, -30.84685318188687120 ) ) ;
#21477 = CYLINDRICAL_SURFACE ( 'NONE', #4922, 5.000000000000039080 ) ;
#21478 = CARTESIAN_POINT ( 'NONE',  ( -280.0000000000000000, 19.99999999999996092, -0.000000000000000000 ) ) ;
#21479 = CARTESIAN_POINT ( 'NONE',  ( 91.82158438592159655, -22.79471317813468545, -40.00000000000002132 ) ) ;
#21480 = CARTESIAN_POINT ( 'NONE',  ( 14.38125909742180752, 17.55144818341448953, 39.01709431150923280 ) ) ;
#21481 = CARTESIAN_POINT ( 'NONE',  ( -30.26275506840323004, -41.69427246844627888, -40.00000000000002132 ) ) ;
#21483 = CARTESIAN_POINT ( 'NONE',  ( 192.4448373802101173, 39.99999999999998579, 19.99999999996075317 ) ) ;
#21482 = CARTESIAN_POINT ( 'NONE',  ( 170.2234770963711128, -17.36149277827010096, 17.36149277826970660 ) ) ;
#21484 = CARTESIAN_POINT ( 'NONE',  ( -96.94475454970501005, -20.58449551012127898, 9.001119816584967737 ) ) ;
#21485 = CARTESIAN_POINT ( 'NONE',  ( -114.7831050401054682, 22.13388504846499671, -0.1750307869482046752 ) ) ;
#21486 = CARTESIAN_POINT ( 'NONE',  ( -192.9588430854689989, 38.51493924976929861, 38.51493924976947625 ) ) ;
#21487 = CARTESIAN_POINT ( 'NONE',  ( -91.56559293963834989, 17.32597176626809699, -40.00000000000002132 ) ) ;
#21488 = ORIENTED_EDGE ( 'NONE', *, *, #22155, .F. ) ;
#21489 = ADVANCED_FACE ( 'NONE', ( #19553 ), #9319, .T. ) ;
#21490 = CARTESIAN_POINT ( 'NONE',  ( 23.58679727197035092, -42.79169916605200541, 23.29637218065948545 ) ) ;
#21491 = VECTOR ( 'NONE', #21376, 1000.000000000000000 ) ;
#21492 = DIRECTION ( 'NONE',  ( 3.936061032557140787E-17, -0.2142691827715865471, -0.9767746502210202797 ) ) ;
#21493 = EDGE_CURVE ( 'NONE', #11462, #12135, #23450, .T. ) ;
#21494 =( BOUNDED_SURFACE ( )  B_SPLINE_SURFACE ( 3, 2, ( 
 ( #17214, #25481, #21472 ),
 ( #19345, #7108, #23350 ),
 ( #5127, #13232, #1254 ),
 ( #21355, #3124, #9238 ),
 ( #7230, #23474, #5246 ),
 ( #13350, #9358, #17468 ) ),
 .UNSPECIFIED., .F., .F., .F. ) 
 B_SPLINE_SURFACE_WITH_KNOTS ( ( 4, 2, 4 ),
 ( 3, 3 ),
 ( 0.04143177204337192970, 0.04845749460347205384, 0.05548321716357218492 ),
 ( 0.000000000000000000, 1.000000000000000000 ),
 .UNSPECIFIED. ) 
 GEOMETRIC_REPRESENTATION_ITEM ( )  RATIONAL_B_SPLINE_SURFACE ( (
 ( 1.000000000000000000, 0.9541700779530459808, 1.000000000000000000),
 ( 1.000000000000000000, 0.9520119500059182061, 1.000000000000000000),
 ( 1.000000000000000000, 0.9503149744749778138, 1.000000000000000000),
 ( 1.000000000000000000, 0.9480088402726788432, 1.000000000000000000),
 ( 1.000000000000000000, 0.9474362538696746716, 1.000000000000000000),
 ( 1.000000000000000000, 0.9474350314971542453, 1.000000000000000000) ) ) 
 REPRESENTATION_ITEM ( '' )  SURFACE ( )  );
#21495 = CARTESIAN_POINT ( 'NONE',  ( -162.0762913951021176, 1.198031840315997298, 57.76657433523996588 ) ) ;
#21496 = CARTESIAN_POINT ( 'NONE',  ( -162.0762913951021176, -40.00000000000005684, 1.694272876828184504 ) ) ;
#21497 = CARTESIAN_POINT ( 'NONE',  ( -82.25907871058393539, 19.72177579145719051, -4.317081979949474402 ) ) ;
#21498 = EDGE_CURVE ( 'NONE', #5885, #24064, #25439, .T. ) ;
#21499 = CIRCLE ( 'NONE', #10026, 15.00000000000000000 ) ;
#21500 = CIRCLE ( 'NONE', #24923, 30.00000000000000355 ) ;
#21501 = AXIS2_PLACEMENT_3D ( 'NONE', #16650, #16777, #2828 ) ;
#21502 = CARTESIAN_POINT ( 'NONE',  ( -24.15343516389538081, 15.53299357102992495, -37.49996374344652139 ) ) ;
#21503 = CARTESIAN_POINT ( 'NONE',  ( 199.9999999999998863, 8.393744152662998559, 17.05383455604227905 ) ) ;
#21504 = CARTESIAN_POINT ( 'NONE',  ( -646.7283122382513056, 32.99571033938487830, -22.66550611626425038 ) ) ;
#21505 = CARTESIAN_POINT ( 'NONE',  ( -213.1075012329537230, 37.98287015391211696, 18.58567234101190735 ) ) ;
#21506 = CARTESIAN_POINT ( 'NONE',  ( -192.9588430854689705, -38.51493924976909966, -38.51493924976973915 ) ) ;
#21507 = CARTESIAN_POINT ( 'NONE',  ( 163.1118516004056573, 47.56205970284957374, 9.006482792074494981 ) ) ;
#21508 = FACE_BOUND ( 'NONE', #3452, .T. ) ;
#21509 = CARTESIAN_POINT ( 'NONE',  ( 0.2972598230770100991, -38.42060263243632079, -38.42060263243699580 ) ) ;
#21511 = CARTESIAN_POINT ( 'NONE',  ( -100.7734535825088500, -16.03295912088659492, -40.53558337403696044 ) ) ;
#21510 = CARTESIAN_POINT ( 'NONE',  ( 151.7948205124836534, 23.49921654116056047, -33.06932595376338213 ) ) ;
#21512 = CARTESIAN_POINT ( 'NONE',  ( 199.9999999999999432, 14.14213562373110911, -14.14213562373072364 ) ) ;
#21513 = CARTESIAN_POINT ( 'NONE',  ( -238.4067589809705794, -0.6820004457913680929, 0.6820004457913170226 ) ) ;
#21514 = DIRECTION ( 'NONE',  ( -1.000000000000000000, 0.000000000000000000, 0.000000000000000000 ) ) ;
#21515 = CARTESIAN_POINT ( 'NONE',  ( 4.995406935893290878, -5.232665749138292703E-14, 15.24977328854832592 ) ) ;
#21516 = CARTESIAN_POINT ( 'NONE',  ( 130.8568914410475088, -4.207082182990058428, 52.36146031193416661 ) ) ;
#21517 = CARTESIAN_POINT ( 'NONE',  ( 130.8568914410475088, 5.949712681206712261, 40.00000000000002132 ) ) ;
#21518 = ORIENTED_EDGE ( 'NONE', *, *, #19719, .T. ) ;
#21519 = CARTESIAN_POINT ( 'NONE',  ( -198.0356074513804572, 67.44298959253333692, 10.87444709760969452 ) ) ;
#21520 = CARTESIAN_POINT ( 'NONE',  ( -100.0753760173618900, -20.72827493166393609, -8.149786832858609387 ) ) ;
#21521 = CARTESIAN_POINT ( 'NONE',  ( -53.37769371643637584, -10.11111068828991577, -29.42719939405419893 ) ) ;
#21522 = CARTESIAN_POINT ( 'NONE',  ( -3.838270362648686707, -43.19795333834416340, -17.89317813949888603 ) ) ;
#21523 = ORIENTED_EDGE ( 'NONE', *, *, #23949, .T. ) ;
#21524 = CARTESIAN_POINT ( 'NONE',  ( -129.2303492453802676, -25.82246949215104337, 9.309000511570687308 ) ) ;
#21525 = CARTESIAN_POINT ( 'NONE',  ( 199.9999999999998863, -5.231270638550959085, -18.27112563740264761 ) ) ;
#21526 = CARTESIAN_POINT ( 'NONE',  ( 23.84827734669550736, -13.76599369847126830, 46.63681169410619276 ) ) ;
#21527 = EDGE_CURVE ( 'NONE', #8430, #22425, #13646, .T. ) ;
#21528 = CARTESIAN_POINT ( 'NONE',  ( 90.71511022964570259, 8.335579106121171478, -21.46756116452269580 ) ) ;
#21529 = CARTESIAN_POINT ( 'NONE',  ( 199.0058919196228260, 8.838798596736017643, -17.93603902042922726 ) ) ;
#21530 = CARTESIAN_POINT ( 'NONE',  ( -87.01512800814687409, 20.72591320789969771, 5.554844834155465705 ) ) ;
#21531 = CARTESIAN_POINT ( 'NONE',  ( 91.82158438592156813, 40.00000000000009948, -17.20528682183286051 ) ) ;
#21533 = AXIS2_PLACEMENT_3D ( 'NONE', #2815, #20634, #12646 ) ;
#21532 = DIRECTION ( 'NONE',  ( 1.000000000000000000, 0.000000000000000000, 0.000000000000000000 ) ) ;
#21534 = CARTESIAN_POINT ( 'NONE',  ( 21.15737826136114208, 47.57244852138565960, -13.91467835516647789 ) ) ;
#21535 = CARTESIAN_POINT ( 'NONE',  ( -198.0356074513804572, -15.37879056873074290, 40.00000000000002132 ) ) ;
#21537 = CARTESIAN_POINT ( 'NONE',  ( -607.2237257255731038, 33.00592889815013109, -22.65123783916381939 ) ) ;
#21536 = CARTESIAN_POINT ( 'NONE',  ( -129.2920262390587993, 10.46331600574958642, -25.26067940841951298 ) ) ;
#21538 = CARTESIAN_POINT ( 'NONE',  ( 163.1118516004056573, 27.26290988616876021, 40.00000000000002132 ) ) ;
#21539 = CARTESIAN_POINT ( 'NONE',  ( -105.3755690713226869, 21.75974354311648540, -0.000000000000000000 ) ) ;
#21540 = AXIS2_PLACEMENT_3D ( 'NONE', #21008, #10497, #2385 ) ;
#21541 = CARTESIAN_POINT ( 'NONE',  ( 130.8568914410475372, -3.326198072800416995E-13, 34.05028731879788495 ) ) ;
#21542 = CARTESIAN_POINT ( 'NONE',  ( 0.2972598230770103767, -39.99999999999945288, -54.33493731733979359 ) ) ;
#21543 = CARTESIAN_POINT ( 'NONE',  ( 100.8632772039314744, -19.41886981475201068, -8.043559243227951683 ) ) ;
#21544 = ORIENTED_EDGE ( 'NONE', *, *, #6629, .T. ) ;
#21546 = CARTESIAN_POINT ( 'NONE',  ( 3.468680969975556305, 44.56630890487243590, -24.60338114558966183 ) ) ;
#21545 = CARTESIAN_POINT ( 'NONE',  ( 200.0000000000000000, -52.49999999999991473, 52.49999999999999289 ) ) ;
#21547 = CARTESIAN_POINT ( 'NONE',  ( -56.48582580120558561, -30.84685318188645908, 40.00000000000002132 ) ) ;
#21548 = CARTESIAN_POINT ( 'NONE',  ( -135.8532207217289738, -6.472252184284280396, 6.472252184284099208 ) ) ;
#21549 = CARTESIAN_POINT ( 'NONE',  ( -188.9524464571040880, 43.19209889639678579, -23.58788642769180655 ) ) ;
#21550 = CARTESIAN_POINT ( 'NONE',  ( 0.000000000000000000, 0.000000000000000000, 0.000000000000000000 ) ) ;
#21551 = ORIENTED_EDGE ( 'NONE', *, *, #4274, .F. ) ;
#21552 = EDGE_LOOP ( 'NONE', ( #24341, #13468 ) ) ;
#21553 = CARTESIAN_POINT ( 'NONE',  ( -259.2033419157646676, 6.730120644403521979, -6.730120644403498886 ) ) ;
#21554 = CARTESIAN_POINT ( 'NONE',  ( 130.1167162091014120, 12.15076864148467628, -29.33455044752955132 ) ) ;
#21555 = EDGE_LOOP ( 'NONE', ( #5981, #7816, #5546, #4859 ) ) ;
#21556 = ORIENTED_EDGE ( 'NONE', *, *, #16141, .T. ) ;
#21557 = CARTESIAN_POINT ( 'NONE',  ( 199.0262399469797572, -16.26902294624164469, 11.64593733880351500 ) ) ;
#21558 = DIRECTION ( 'NONE',  ( 0.000000000000000000, -1.000000000000000000, 0.000000000000000000 ) ) ;
#21559 = CARTESIAN_POINT ( 'NONE',  ( 130.8568914410475372, 4.207082182992862407, 4.207082182992856190 ) ) ;
#21560 = DIRECTION ( 'NONE',  ( 0.000000000000000000, 1.000000000000000000, 0.000000000000000000 ) ) ;
#21561 = FACE_OUTER_BOUND ( 'NONE', #18948, .T. ) ;
#21562 = CARTESIAN_POINT ( 'NONE',  ( 18.90082769090740200, -14.00978943384292208, 48.20711988125824377 ) ) ;
#21563 = DIRECTION ( 'NONE',  ( 0.000000000000000000, 0.000000000000000000, 1.000000000000000000 ) ) ;
#21564 = CARTESIAN_POINT ( 'NONE',  ( -53.37686176745754096, 13.65870576116527957, -27.95807077219528480 ) ) ;
#21565 = CARTESIAN_POINT ( 'NONE',  ( 130.8568914410475088, -39.99999999999992895, -5.949712681207114606 ) ) ;
#21566 = CARTESIAN_POINT ( 'NONE',  ( 0.2972598230769956662, 40.00000000000058975, -54.33493731733894094 ) ) ;
#21567 = DIRECTION ( 'NONE',  ( 0.000000000000000000, 1.000000000000000000, 0.000000000000000000 ) ) ;
#21568 = CARTESIAN_POINT ( 'NONE',  ( 192.4448373802100889, 14.14213562375893574, -14.14213562375874922 ) ) ;
#21569 = CARTESIAN_POINT ( 'NONE',  ( 136.1360204305621266, 1.473277640373554421E-13, -35.03383547441296741 ) ) ;
#21570 = CARTESIAN_POINT ( 'NONE',  ( -280.0000000000000000, 14.14213562373098299, -14.14213562373088706 ) ) ;
#21571 = CARTESIAN_POINT ( 'NONE',  ( 141.7948666911895259, 30.38861427224621536, 12.58737617328915448 ) ) ;
#21572 = PLANE ( 'NONE',  #15336 ) ;
#21573 = CARTESIAN_POINT ( 'NONE',  ( -100.7734535825088500, 16.03295912088713848, -16.03295912088698927 ) ) ;
#21574 = CARTESIAN_POINT ( 'NONE',  ( -100.7734535825088500, -39.99999999999995737, -22.67402823373205578 ) ) ;
#21575 = CARTESIAN_POINT ( 'NONE',  ( 130.8568914410475088, -52.36146031193419503, 4.207082182989537955 ) ) ;
#21576 = CARTESIAN_POINT ( 'NONE',  ( 170.2234770963711128, -39.20704971665404059, 17.36149277826957160 ) ) ;
#21577 = CARTESIAN_POINT ( 'NONE',  ( -121.8281150758381557, -8.694016608770111176, -23.07023398735807262 ) ) ;
#21578 = LINE ( 'NONE', #7089, #8748 ) ;
#21579 = EDGE_CURVE ( 'NONE', #6963, #9873, #450, .T. ) ;
#21580 = ORIENTED_EDGE ( 'NONE', *, *, #3146, .F. ) ;
#21581 = CARTESIAN_POINT ( 'NONE',  ( 19.06497207195981858, 10.03556273973516078, -66.60410523465806421 ) ) ;
#21582 = CYLINDRICAL_SURFACE ( 'NONE', #4354, 74.99999999999991473 ) ;
#21583 = CARTESIAN_POINT ( 'NONE',  ( 170.0000000000001137, 3.062538285712881336, 24.95097643317000191 ) ) ;
#21584 = ORIENTED_EDGE ( 'NONE', *, *, #7357, .T. ) ;
#21585 = APPLICATION_CONTEXT ( 'automotive_design' ) ;
#21586 = CARTESIAN_POINT ( 'NONE',  ( 91.82158438592158234, -1.633484621919921769E-13, 17.20528682183300262 ) ) ;
#21587 = CARTESIAN_POINT ( 'NONE',  ( 199.0168320490197402, -15.28088196978702129, -12.92611743443934813 ) ) ;
#21588 = CARTESIAN_POINT ( 'NONE',  ( -70.35386311724839459, 8.707385196241270719, 23.12931224237960848 ) ) ;
#21589 = ORIENTED_EDGE ( 'NONE', *, *, #25263, .F. ) ;
#21590 = ORIENTED_EDGE ( 'NONE', *, *, #23947, .F. ) ;
#21591 = CARTESIAN_POINT ( 'NONE',  ( -91.56559293963836410, -12.25131212657462321, -44.31723036834905827 ) ) ;
#21592 = CARTESIAN_POINT ( 'NONE',  ( 4.995406935893292655, 39.99999999999982947, 55.24977328856478209 ) ) ;
#21593 = ADVANCED_FACE ( 'NONE', ( #11558 ), #18206, .T. ) ;
#21594 = CARTESIAN_POINT ( 'NONE',  ( -86.86493150571118349, -19.77569912839183885, -7.943527260495956810 ) ) ;
#21595 = EDGE_CURVE ( 'NONE', #16510, #24713, #14222, .T. ) ;
#21596 = CARTESIAN_POINT ( 'NONE',  ( -280.0000000000000000, 14.14213562373108424, -14.14213562373078759 ) ) ;
#21597 = CARTESIAN_POINT ( 'NONE',  ( 136.1360204305621551, -40.00000000000001421, 4.966164525586921563 ) ) ;
#21598 = CARTESIAN_POINT ( 'NONE',  ( 199.9999999999998295, -19.00894346483091724, 0.1575548292166454312 ) ) ;
#21599 = CARTESIAN_POINT ( 'NONE',  ( 146.6084372240433709, 40.00000000000003553, 5.374981219217116468 ) ) ;
#21600 = CARTESIAN_POINT ( 'NONE',  ( -189.9999999999999716, 82.50000000000008527, 52.49999999999977973 ) ) ;
#21601 = CARTESIAN_POINT ( 'NONE',  ( -7.769366557097388437, -22.72119856428940210, -41.90323276218089887 ) ) ;
#21602 = CARTESIAN_POINT ( 'NONE',  ( 146.6084372240433709, 52.76785682606523409, -3.800685668858194255 ) ) ;
#21603 = FACE_OUTER_BOUND ( 'NONE', #252, .T. ) ;
#21604 = CARTESIAN_POINT ( 'NONE',  ( 19.06497207195982924, -39.99999999999945288, -54.19242893257885640 ) ) ;
#21605 = CARTESIAN_POINT ( 'NONE',  ( 169.9999999999999432, -24.25569233607180308, 6.285860131565189413 ) ) ;
#21606 = CARTESIAN_POINT ( 'NONE',  ( -162.0762913951021176, -1.694272876828353702, 40.00000000000002132 ) ) ;
#21607 = CARTESIAN_POINT ( 'NONE',  ( -259.2033419157646676, -30.48217210827743884, -40.00000000000002132 ) ) ;
#21608 = CARTESIAN_POINT ( 'NONE',  ( -162.0762913951020892, -1.198031840385783919, 1.198031840385741731 ) ) ;
#21609 = CARTESIAN_POINT ( 'NONE',  ( -280.0000000000000568, 19.99999999999996092, -40.00000000000002132 ) ) ;
#21611 = CARTESIAN_POINT ( 'NONE',  ( 0.000000000000000000, 0.000000000000000000, 0.000000000000000000 ) ) ;
#21610 = CARTESIAN_POINT ( 'NONE',  ( 0.4311942631276012294, -44.08816696360405274, -24.25071831022401625 ) ) ;
#21612 = CARTESIAN_POINT ( 'NONE',  ( -238.4067589809705794, -3.369206980223063916E-14, -0.9644942799825824142 ) ) ;
#21613 = CARTESIAN_POINT ( 'NONE',  ( -238.4067589809705794, 57.25054294077225592, 0.6820004458485544596 ) ) ;
#21614 = CARTESIAN_POINT ( 'NONE',  ( -280.0000000000000000, 19.99999999999996092, 2.449293598294708485E-15 ) ) ;
#21616 = EDGE_LOOP ( 'NONE', ( #23364, #3996, #25265, #8866 ) ) ;
#21615 = AXIS2_PLACEMENT_3D ( 'NONE', #26129, #16124, #34 ) ;
#21617 = CARTESIAN_POINT ( 'NONE',  ( 36.66494225461514844, -39.17447069114134450, 16.22659705900260718 ) ) ;
#21618 = CARTESIAN_POINT ( 'NONE',  ( -200.0000000000000000, -69.99999999999995737, 0.000000000000000000 ) ) ;
#21619 = CARTESIAN_POINT ( 'NONE',  ( 14.38125909742181108, 39.01709431150907648, 39.01709431150921858 ) ) ;
#21620 = CARTESIAN_POINT ( 'NONE',  ( -198.0356074513804572, -9.007331120208026888E-14, 15.37879056873070560 ) ) ;
#21621 = CARTESIAN_POINT ( 'NONE',  ( -87.12536333654861664, 21.43930114797831621, 1.600202314776014489 ) ) ;
#21622 = DIRECTION ( 'NONE',  ( 5.551115123125783491E-15, 0.3995982397861026492, 0.9166903767138872006 ) ) ;
#21623 = CARTESIAN_POINT ( 'NONE',  ( 199.9999999999998863, 9.495902909754645904, 16.46521490772419583 ) ) ;
#21624 = CARTESIAN_POINT ( 'NONE',  ( -87.04313178894965120, -4.721723262651171815, -20.90674919797856646 ) ) ;
#21625 = CARTESIAN_POINT ( 'NONE',  ( -135.8532207217289738, 21.81201906317729566, 34.75652343174635917 ) ) ;
#21626 = CARTESIAN_POINT ( 'NONE',  ( -238.4067589809705794, -0.6820004457337348613, -57.25054294065803617 ) ) ;
#21627 = EDGE_CURVE ( 'NONE', #14909, #25810, #10868, .T. ) ;
#21628 = CARTESIAN_POINT ( 'NONE',  ( -110.1016741620976518, 20.19284057200533056, -0.4456461246811765919 ) ) ;
#21629 = CARTESIAN_POINT ( 'NONE',  ( -86.86493150571115507, 7.943527260496353826, 19.77569912839162569 ) ) ;
#21630 = CARTESIAN_POINT ( 'NONE',  ( 200.0000000000000000, 42.42640687119310172, -14.14213562373052646 ) ) ;
#21632 = CARTESIAN_POINT ( 'NONE',  ( 146.6084372240433709, -24.48358557860284179, -32.08495691632087699 ) ) ;
#21631 = CARTESIAN_POINT ( 'NONE',  ( 4.995406935893287326, 17.50105314357225694, -39.06748935135176026 ) ) ;
#21633 = CARTESIAN_POINT ( 'NONE',  ( -162.0762913951020892, 29.48230308784799902, -29.48230308784730980 ) ) ;
#21634 = AXIS2_PLACEMENT_3D ( 'NONE', #8366, #20614, #2390 ) ;
#21635 = CARTESIAN_POINT ( 'NONE',  ( 4.995406935893288214, 15.24977328854832770, 0.000000000000000000 ) ) ;
#21636 = ADVANCED_FACE ( 'NONE', ( #9839 ), #16220, .F. ) ;
#21637 = CARTESIAN_POINT ( 'NONE',  ( -716.9846540392142060, 66.50000000000009948, -66.50000000000005684 ) ) ;
#21638 = CARTESIAN_POINT ( 'NONE',  ( -162.0762913951021176, -40.00000000000005684, 1.694272876828184504 ) ) ;
#21639 = B_SPLINE_CURVE_WITH_KNOTS ( 'NONE', 3,
 ( #5281, #1289, #7521, #11511, #25644, #15385, #26040, #26175 ),
 .UNSPECIFIED., .F., .F.,
 ( 4, 2, 2, 4 ),
 ( 0.008396560128413051854, 0.01250087472273852390, 0.01455303201990126340, 0.01660518931706400289 ),
 .UNSPECIFIED. ) ;
#21640 = CARTESIAN_POINT ( 'NONE',  ( 4.995406935893293543, -10.78321810388990265, -10.78321810389009272 ) ) ;
#21641 = CARTESIAN_POINT ( 'NONE',  ( -56.48582580120559982, -9.153146818113595984, 40.00000000000002132 ) ) ;
#21642 = EDGE_LOOP ( 'NONE', ( #25856, #13588 ) ) ;
#21643 = CARTESIAN_POINT ( 'NONE',  ( -86.96347745069644475, 41.18208027870598187, -15.38646221621779731 ) ) ;
#21644 =( BOUNDED_SURFACE ( )  B_SPLINE_SURFACE ( 3, 3, ( 
 ( #10172, #3933, #10036, #16553, #6438, #20554, #18145, #16684, #14290, #5916, #24681, #8297, #467, #6178, #16285, #2456, #22426, #2199, #18681, #6306, #14555, #4201, #14423, #22555, #20422, #10566, #24283, #22685, #4334, #2323 ),
 ( #16423, #12030, #12554, #8570, #14024, #10432, #14157, #10308, #20686, #20150, #22152, #26293, #24413, #22289, #18549, #8032, #18414, #1931, #8171, #16152, #18277, #6052, #330, #62, #4063, #4461, #8433, #12166, #20287, #2066 ),
 ( #189, #3115, #9228, #865, #14686, #10976, #8974, #22819, #16949, #2734, #2596, #24815, #22949, #6835, #10839, #10710, #21085, #18955, #16817, #19334, #4595, #736, #6567, #17083, #24957, #14816, #14954, #8842, #23089, #21344 ),
 ( #599, #18819, #12835, #21218, #12693, #13225, #20822, #15215, #6703, #7102, #25084, #8706, #19086, #25217, #17207, #4860, #6966, #15082, #12965, #11220, #4728, #9099, #23215, #4994, #20955, #23342, #1120, #13100, #2869, #2992 ),
 ( #11097, #19212, #995, #25345, #5118, #21809, #9834, #25951, #18073, #3582, #3857, #6110, #19941, #2124, #21945, #25816, #9967, #3721, #11685, #22347, #12094, #7693, #19811, #26224, #8095, #1993, #17939, #16078, #14087, #23800 ),
 ( #20085, #7562, #26085, #11823, #1597, #17674, #15805, #7820, #1726, #9698, #13949, #15936, #17805, #12225, #15675, #24069, #5581, #1864, #23930, #5705, #5845, #22084, #11960, #14218, #13688, #5979, #22218, #13811, #20215, #3994 ),
 ( #24206, #10099, #7960, #18201, #16215, #24346, #20347, #22354, #4131, #10232, #22742, #8362, #4524, #20883, #4792, #18610, #20750, #10636, #2519, #8766, #12484, #16880, #23017, #16611, #123, #6241, #12757, #14482, #8228, #14354 ) ),
 .UNSPECIFIED., .T., .F., .F. ) 
 B_SPLINE_SURFACE_WITH_KNOTS ( ( 4, 3, 4 ),
 ( 4, 2, 2, 2, 2, 2, 2, 2, 2, 2, 2, 2, 2, 2, 4 ),
 ( 0.000000000000000000, 0.5000000000000000000, 1.000000000000000000 ),
 ( 0.000000000000000000, 0.1357259735107005372, 0.1651108541090157700, 0.1944957347073310028, 0.3598804999793158710, 0.3867117631979620773, 0.4135430264166082281, 0.5789277916885930964, 0.6062785021374117456, 0.6336292125862302838, 0.8508620842112317728, 0.8814014469398914198, 0.9119408096685510667, 0.9559704048342755334, 1.000000000000000000 ),
 .UNSPECIFIED. ) 
 GEOMETRIC_REPRESENTATION_ITEM ( )  RATIONAL_B_SPLINE_SURFACE ( (
 ( 1.000000000000000000, 1.000000000000000000, 1.000000000000000000, 1.000000000000000000, 1.000000000000000000, 1.000000000000000000, 1.000000000000000000, 1.000000000000000000, 1.000000000000000000, 1.000000000000000000, 1.000000000000000000, 1.000000000000000000, 1.000000000000000000, 1.000000000000000000, 1.000000000000000000, 1.000000000000000000, 1.000000000000000000, 1.000000000000000000, 1.000000000000000000, 1.000000000000000000, 1.000000000000000000, 1.000000000000000000, 1.000000000000000000, 1.000000000000000000, 1.000000000000000000, 1.000000000000000000, 1.000000000000000000, 1.000000000000000000, 1.000000000000000000, 1.000000000000000000),
 ( 0.3333333333333333703, 0.3333333333333333703, 0.3333333333333333703, 0.3333333333333333703, 0.3333333333333333703, 0.3333333333333333703, 0.3333333333333333703, 0.3333333333333333703, 0.3333333333333333703, 0.3333333333333333703, 0.3333333333333333703, 0.3333333333333333703, 0.3333333333333333703, 0.3333333333333333703, 0.3333333333333333703, 0.3333333333333333703, 0.3333333333333333703, 0.3333333333333333703, 0.3333333333333333703, 0.3333333333333333703, 0.3333333333333333703, 0.3333333333333333703, 0.3333333333333333703, 0.3333333333333333703, 0.3333333333333333703, 0.3333333333333333703, 0.3333333333333333703, 0.3333333333333333703, 0.3333333333333333703, 0.3333333333333333703),
 ( 0.3333333333333333703, 0.3333333333333333703, 0.3333333333333333703, 0.3333333333333333703, 0.3333333333333333703, 0.3333333333333333703, 0.3333333333333333703, 0.3333333333333333703, 0.3333333333333333703, 0.3333333333333333703, 0.3333333333333333703, 0.3333333333333333703, 0.3333333333333333703, 0.3333333333333333703, 0.3333333333333333703, 0.3333333333333333703, 0.3333333333333333703, 0.3333333333333333703, 0.3333333333333333703, 0.3333333333333333703, 0.3333333333333333703, 0.3333333333333333703, 0.3333333333333333703, 0.3333333333333333703, 0.3333333333333333703, 0.3333333333333333703, 0.3333333333333333703, 0.3333333333333333703, 0.3333333333333333703, 0.3333333333333333703),
 ( 1.000000000000000000, 1.000000000000000000, 1.000000000000000000, 1.000000000000000000, 1.000000000000000000, 1.000000000000000000, 1.000000000000000000, 1.000000000000000000, 1.000000000000000000, 1.000000000000000000, 1.000000000000000000, 1.000000000000000000, 1.000000000000000000, 1.000000000000000000, 1.000000000000000000, 1.000000000000000000, 1.000000000000000000, 1.000000000000000000, 1.000000000000000000, 1.000000000000000000, 1.000000000000000000, 1.000000000000000000, 1.000000000000000000, 1.000000000000000000, 1.000000000000000000, 1.000000000000000000, 1.000000000000000000, 1.000000000000000000, 1.000000000000000000, 1.000000000000000000),
 ( 0.3333333333333333703, 0.3333333333333333703, 0.3333333333333333703, 0.3333333333333333703, 0.3333333333333333703, 0.3333333333333333703, 0.3333333333333333703, 0.3333333333333333703, 0.3333333333333333703, 0.3333333333333333703, 0.3333333333333333703, 0.3333333333333333703, 0.3333333333333333703, 0.3333333333333333703, 0.3333333333333333703, 0.3333333333333333703, 0.3333333333333333703, 0.3333333333333333703, 0.3333333333333333703, 0.3333333333333333703, 0.3333333333333333703, 0.3333333333333333703, 0.3333333333333333703, 0.3333333333333333703, 0.3333333333333333703, 0.3333333333333333703, 0.3333333333333333703, 0.3333333333333333703, 0.3333333333333333703, 0.3333333333333333703),
 ( 0.3333333333333333703, 0.3333333333333333703, 0.3333333333333333703, 0.3333333333333333703, 0.3333333333333333703, 0.3333333333333333703, 0.3333333333333333703, 0.3333333333333333703, 0.3333333333333333703, 0.3333333333333333703, 0.3333333333333333703, 0.3333333333333333703, 0.3333333333333333703, 0.3333333333333333703, 0.3333333333333333703, 0.3333333333333333703, 0.3333333333333333703, 0.3333333333333333703, 0.3333333333333333703, 0.3333333333333333703, 0.3333333333333333703, 0.3333333333333333703, 0.3333333333333333703, 0.3333333333333333703, 0.3333333333333333703, 0.3333333333333333703, 0.3333333333333333703, 0.3333333333333333703, 0.3333333333333333703, 0.3333333333333333703),
 ( 1.000000000000000000, 1.000000000000000000, 1.000000000000000000, 1.000000000000000000, 1.000000000000000000, 1.000000000000000000, 1.000000000000000000, 1.000000000000000000, 1.000000000000000000, 1.000000000000000000, 1.000000000000000000, 1.000000000000000000, 1.000000000000000000, 1.000000000000000000, 1.000000000000000000, 1.000000000000000000, 1.000000000000000000, 1.000000000000000000, 1.000000000000000000, 1.000000000000000000, 1.000000000000000000, 1.000000000000000000, 1.000000000000000000, 1.000000000000000000, 1.000000000000000000, 1.000000000000000000, 1.000000000000000000, 1.000000000000000000, 1.000000000000000000, 1.000000000000000000) ) ) 
 REPRESENTATION_ITEM ( '' )  SURFACE ( )  );
#21645 = CARTESIAN_POINT ( 'NONE',  ( -8.311322960495319379, 41.20580916678637351, 17.06800500544055765 ) ) ;
#21646 = CARTESIAN_POINT ( 'NONE',  ( 23.58679727196754428, 13.78527791281921644, 46.73132340480187707 ) ) ;
#21647 = CARTESIAN_POINT ( 'NONE',  ( -77.90255099906875103, -20.29001641120621002, -8.064892378658361949 ) ) ;
#21648 = ORIENTED_EDGE ( 'NONE', *, *, #1426, .T. ) ;
#21649 = CARTESIAN_POINT ( 'NONE',  ( -188.3610564113219823, -47.01267209787972234, 13.83140491817315976 ) ) ;
#21650 = CARTESIAN_POINT ( 'NONE',  ( 199.9999999999998863, -4.322767242657778120, -18.50495320732392557 ) ) ;
#21651 = CARTESIAN_POINT ( 'NONE',  ( 25.88393124174215743, -22.82896322165249359, 42.08451360837295852 ) ) ;
#21652 = AXIS2_PLACEMENT_3D ( 'NONE', #13744, #21870, #9369 ) ;
#21653 = CARTESIAN_POINT ( 'NONE',  ( -111.5098000082168710, 19.36828941575083363, 8.022608155968326216 ) ) ;
#21654 = CARTESIAN_POINT ( 'NONE',  ( 199.0068982850735608, 19.44025291972790370, -4.682182605709538592 ) ) ;
#21655 = CARTESIAN_POINT ( 'NONE',  ( -716.9846540392142060, 0.000000000000000000, 0.000000000000000000 ) ) ;
#21656 = CARTESIAN_POINT ( 'NONE',  ( 170.2234770963711128, 40.00000000000000000, 15.44714144992830462 ) ) ;
#21657 = CARTESIAN_POINT ( 'NONE',  ( -86.86493150571119770, -7.943527260496137110, 19.77569912839176425 ) ) ;
#21658 = EDGE_CURVE ( 'NONE', #1858, #12216, #4754, .T. ) ;
#21659 = CARTESIAN_POINT ( 'NONE',  ( -199.9999999999999432, -14.52307781036537193, -48.92947633520097384 ) ) ;
#21660 = CARTESIAN_POINT ( 'NONE',  ( 4.995406935893294431, -15.24977328854832415, 40.00000000000002132 ) ) ;
#21662 = CARTESIAN_POINT ( 'NONE',  ( -618.9247522084408502, 27.64368523546104939, -28.91374874216926116 ) ) ;
#21661 = CARTESIAN_POINT ( 'NONE',  ( -144.0562696874938524, 10.50947022281075860, -31.27040355056193022 ) ) ;
#21663 = EDGE_CURVE ( 'NONE', #7220, #17385, #18780, .T. ) ;
#21664 = CARTESIAN_POINT ( 'NONE',  ( -105.3755690713226585, 21.75974354311648185, 40.00000000000002132 ) ) ;
#21665 = CARTESIAN_POINT ( 'NONE',  ( -135.8532207217289738, 9.153146818113548022, -40.00000000000002132 ) ) ;
#21666 = CARTESIAN_POINT ( 'NONE',  ( 184.8905102610680444, -20.92133201514440799, 0.000000000000000000 ) ) ;
#21667 = CARTESIAN_POINT ( 'NONE',  ( -208.1127848780264742, 40.00000000000014211, -15.00245453012627728 ) ) ;
#21668 = CYLINDRICAL_SURFACE ( 'NONE', #12294, 10.00000000000000888 ) ;
#21669 = CARTESIAN_POINT ( 'NONE',  ( 137.0932223649025161, -30.33046076074802855, -12.56328820012686798 ) ) ;
#21670 = EDGE_CURVE ( 'NONE', #16641, #18580, #19198, .T. ) ;
#21671 = EDGE_CURVE ( 'NONE', #12165, #12221, #7285, .T. ) ;
#21672 = ORIENTED_EDGE ( 'NONE', *, *, #20361, .F. ) ;
#21674 = CARTESIAN_POINT ( 'NONE',  ( 6.762329110785001873, 44.82519229649617643, -18.56720258520260813 ) ) ;
#21673 = CARTESIAN_POINT ( 'NONE',  ( -190.0000000000000000, 74.99999999999995737, 9.184850993605144000E-15 ) ) ;
#21675 = CARTESIAN_POINT ( 'NONE',  ( 91.82158438592159655, -22.79471317813468900, 40.00000000000002132 ) ) ;
#21676 = CIRCLE ( 'NONE', #8949, 5.000000000000004441 ) ;
#21677 = CARTESIAN_POINT ( 'NONE',  ( -163.5815475687391825, -38.33196416462971712, 12.03526863292968230 ) ) ;
#21678 = CARTESIAN_POINT ( 'NONE',  ( -88.37877758185140920, -8.575405935195258067, 19.92653024451507093 ) ) ;
#21679 = EDGE_LOOP ( 'NONE', ( #14515, #16776, #24843, #8395 ) ) ;
#21680 = ORIENTED_EDGE ( 'NONE', *, *, #9879, .T. ) ;
#21681 = CARTESIAN_POINT ( 'NONE',  ( 155.1206158682454657, 11.51471166709257865, -27.79897307351022917 ) ) ;
#21682 = VERTEX_POINT ( 'NONE', #21949 ) ;
#21683 = CARTESIAN_POINT ( 'NONE',  ( -102.4068193528164841, 8.088405365068929598, -20.44188272012819496 ) ) ;
#21684 = ORIENTED_EDGE ( 'NONE', *, *, #2672, .T. ) ;
#21685 = CARTESIAN_POINT ( 'NONE',  ( 199.9999999999998863, -9.236595569432955344, 16.61620204157069125 ) ) ;
#21686 = CARTESIAN_POINT ( 'NONE',  ( -196.0240758340695777, 14.12332442061101467, 48.96019759410229000 ) ) ;
#21687 = CARTESIAN_POINT ( 'NONE',  ( 192.4448373802101173, -14.14213562375886291, 42.42640687116498555 ) ) ;
#21688 = FACE_OUTER_BOUND ( 'NONE', #16781, .T. ) ;
#21689 = CARTESIAN_POINT ( 'NONE',  ( -213.1075012329537230, -8.703598725189323045E-14, 13.71589010951911902 ) ) ;
#21690 = CARTESIAN_POINT ( 'NONE',  ( -4.039451493210485467, -13.82811171175474207, 46.99046209229799587 ) ) ;
#21691 = DIRECTION ( 'NONE',  ( 0.000000000000000000, 1.000000000000000000, 0.000000000000000000 ) ) ;
#21692 = CARTESIAN_POINT ( 'NONE',  ( -28.75704569508430808, 18.59466133783093866, -35.61514925947727050 ) ) ;
#21693 = CARTESIAN_POINT ( 'NONE',  ( -192.9588430854689989, 1.161019517985663313E-13, -14.46834944099969533 ) ) ;
#21694 = CARTESIAN_POINT ( 'NONE',  ( -91.56559293963834989, 1.671088883502053755E-13, -17.32597176626811120 ) ) ;
#21695 = CARTESIAN_POINT ( 'NONE',  ( -199.9999999999999716, -46.88040655664269707, -17.27712336974166618 ) ) ;
#21696 = CARTESIAN_POINT ( 'NONE',  ( 184.8905102610680444, 14.79361573936396113, -14.79361573936377461 ) ) ;
#21697 = CARTESIAN_POINT ( 'NONE',  ( -199.9999999999999432, 15.63350978565376082, -47.95319408140855444 ) ) ;
#21698 = CARTESIAN_POINT ( 'NONE',  ( -195.1686598214383537, 14.09692385498526690, 48.78512304065124994 ) ) ;
#21699 = DIRECTION ( 'NONE',  ( -1.000000000000000000, -1.836970198721030181E-16, -2.465190328815661892E-32 ) ) ;
#21700 = CARTESIAN_POINT ( 'NONE',  ( -77.79405973474324298, 19.55084590669568456, -9.945757298482792663 ) ) ;
#21701 = CARTESIAN_POINT ( 'NONE',  ( 199.9999999999999432, 14.14213562373113398, -14.14213562373094923 ) ) ;
#21702 = CARTESIAN_POINT ( 'NONE',  ( -208.1127848780265026, -9.061048840815752106E-14, 15.00245453012669472 ) ) ;
#21703 = CARTESIAN_POINT ( 'NONE',  ( -208.1127848780264742, 10.60833733270764867, 67.17687982763166588 ) ) ;
#21704 = CARTESIAN_POINT ( 'NONE',  ( 136.1360204305621266, -3.511608612530630058, -3.511608612530719764 ) ) ;
#21705 = CARTESIAN_POINT ( 'NONE',  ( -657.8774556453281548, 41.88472458230610584, -16.46082976225948613 ) ) ;
#21706 = CARTESIAN_POINT ( 'NONE',  ( 21.16156876808018339, 23.80729322913559898, 43.48822901267189422 ) ) ;
#21707 = ORIENTED_EDGE ( 'NONE', *, *, #9011, .T. ) ;
#21708 = CARTESIAN_POINT ( 'NONE',  ( -213.1075012329537230, 37.98287015391280619, -37.98287015391192512 ) ) ;
#21709 = LINE ( 'NONE', #3487, #13684 ) ;
#21710 = CARTESIAN_POINT ( 'NONE',  ( -609.7891919193333479, 33.09846309977769607, 30.48971931906038435 ) ) ;
#21711 = EDGE_LOOP ( 'NONE', ( #8934, #9346, #8704, #19133 ) ) ;
#21712 = AXIS2_PLACEMENT_3D ( 'NONE', #7644, #7522, #21897 ) ;
#21713 = CARTESIAN_POINT ( 'NONE',  ( -162.0762913951020892, -1.202636532414034422E-14, -1.694272876828323948 ) ) ;
#21714 = CARTESIAN_POINT ( 'NONE',  ( 199.0260502585402378, -17.33706145817157562, 10.06788908951285499 ) ) ;
#21715 = CARTESIAN_POINT ( 'NONE',  ( -39.84211263215726007, 13.56589830558360532, 32.75097567529046927 ) ) ;
#21716 = CIRCLE ( 'NONE', #8108, 6.000000000000019540 ) ;
#21717 = AXIS2_PLACEMENT_3D ( 'NONE', #25325, #12817, #5101 ) ;
#21718 = ORIENTED_EDGE ( 'NONE', *, *, #10945, .T. ) ;
#21719 = ORIENTED_EDGE ( 'NONE', *, *, #21579, .T. ) ;
#21720 = CIRCLE ( 'NONE', #12366, 14.99999999999999467 ) ;
#21721 = CARTESIAN_POINT ( 'NONE',  ( 91.82158438592158234, 22.79471317813472453, -40.00000000000002132 ) ) ;
#21722 = CARTESIAN_POINT ( 'NONE',  ( 130.8568914410475372, 24.07718906447243867, -24.07718906447216156 ) ) ;
#21723 = CARTESIAN_POINT ( 'NONE',  ( 192.4448373802101173, 39.99999999999998579, 19.99999999996075317 ) ) ;
#21724 = CARTESIAN_POINT ( 'NONE',  ( -114.7539998840383504, -17.50311857019343620, -13.57334797814988470 ) ) ;
#21725 = CYLINDRICAL_SURFACE ( 'NONE', #17359, 69.99999999999995737 ) ;
#21726 = CARTESIAN_POINT ( 'NONE',  ( -109.1264249741489323, 33.12752917269099839, -13.72187187124618646 ) ) ;
#21727 = CARTESIAN_POINT ( 'NONE',  ( 57.59792236341147742, -1.230234673553095937E-13, 37.56421063658186199 ) ) ;
#21728 = CARTESIAN_POINT ( 'NONE',  ( 199.9999999999996589, -18.97053056118941328, 1.250588282361275283 ) ) ;
#21729 = CARTESIAN_POINT ( 'NONE',  ( -192.9588430854689989, -8.596193650988133061E-14, 14.46834944099969533 ) ) ;
#21730 = CARTESIAN_POINT ( 'NONE',  ( -200.0000000000000000, -52.49999999999991473, 52.49999999999999289 ) ) ;
#21731 = CARTESIAN_POINT ( 'NONE',  ( -77.90255099906774205, -8.644468104261530783, -20.04994828523958006 ) ) ;
#21732 = CARTESIAN_POINT ( 'NONE',  ( -259.2033419157646676, 6.730120644403918995, -49.83842185052024831 ) ) ;
#21733 = CARTESIAN_POINT ( 'NONE',  ( -105.2054292635175727, -21.49321519473986442, 0.6800022380102618280 ) ) ;
#21734 = CARTESIAN_POINT ( 'NONE',  ( 151.7948205124836534, -40.00000000000034817, 33.23291073765511072 ) ) ;
#21735 = FACE_OUTER_BOUND ( 'NONE', #2757, .T. ) ;
#21736 = CARTESIAN_POINT ( 'NONE',  ( -91.56559293963836410, 22.67402823373190301, 40.00000000000002132 ) ) ;
#21737 = CARTESIAN_POINT ( 'NONE',  ( 184.8905102610680444, 20.92133201514447194, -40.00000000000002132 ) ) ;
#21738 = CARTESIAN_POINT ( 'NONE',  ( 19.06497207195981147, -10.03556273973439517, 10.03556273973429214 ) ) ;
#21739 = CARTESIAN_POINT ( 'NONE',  ( -259.2033419157646676, -30.48217210827743884, -40.00000000000002132 ) ) ;
#21740 = CARTESIAN_POINT ( 'NONE',  ( 4.990269915386285504, -44.75621547178040771, -24.74342916192413355 ) ) ;
#21741 = EDGE_CURVE ( 'NONE', #19209, #8230, #16195, .T. ) ;
#21742 = CARTESIAN_POINT ( 'NONE',  ( -280.0000000000000568, 39.99999999999976552, 20.00000000000043343 ) ) ;
#21743 = CARTESIAN_POINT ( 'NONE',  ( 19.06497207195980792, 66.60410523465817789, 10.03556273973446800 ) ) ;
#21744 = CARTESIAN_POINT ( 'NONE',  ( 151.7948205124836534, 6.767089262349062828, -40.00000000000002132 ) ) ;
#21745 = EDGE_LOOP ( 'NONE', ( #19845, #1692 ) ) ;
#21746 = CARTESIAN_POINT ( 'NONE',  ( 23.37583784646189500, -42.85659535397651609, 23.33923448557682789 ) ) ;
#21747 = CIRCLE ( 'NONE', #24323, 5.000000000000004441 ) ;
#21748 = DIRECTION ( 'NONE',  ( -1.000000000000000000, -1.836970198721030181E-16, -0.000000000000000000 ) ) ;
#21749 = CARTESIAN_POINT ( 'NONE',  ( -105.3755690713226585, 41.18208027870598187, -15.38646221621779731 ) ) ;
#21750 = CARTESIAN_POINT ( 'NONE',  ( 4.995406935893298872, -1.944352046434030652E-13, 55.24977328854835434 ) ) ;
#21751 = CARTESIAN_POINT ( 'NONE',  ( 184.8905102610680444, 13.49065550809757497, 43.07788698682593065 ) ) ;
#21752 = CARTESIAN_POINT ( 'NONE',  ( 163.1118516004056573, 12.73709011382478806, -40.00000000000002132 ) ) ;
#21753 = CARTESIAN_POINT ( 'NONE',  ( -190.0000000000000000, 61.50000000000009948, 66.50000000000005684 ) ) ;
#21754 = CARTESIAN_POINT ( 'NONE',  ( 199.9999999999998863, 12.28125103214278901, 14.50804496155330447 ) ) ;
#21755 = EDGE_CURVE ( 'NONE', #10496, #20012, #11965, .T. ) ;
#21756 = CARTESIAN_POINT ( 'NONE',  ( -82.28162732594363149, 6.256644183661008718, -19.22463888481380323 ) ) ;
#21757 = CARTESIAN_POINT ( 'NONE',  ( 57.59792236341147031, 26.56190807104652052, 30.00663442387728708 ) ) ;
#21758 = CARTESIAN_POINT ( 'NONE',  ( 146.6084372240433709, 52.76785682606523409, -3.800685668858194255 ) ) ;
#21759 = FACE_OUTER_BOUND ( 'NONE', #13552, .T. ) ;
#21760 = FACE_OUTER_BOUND ( 'NONE', #21177, .T. ) ;
#21761 = CARTESIAN_POINT ( 'NONE',  ( 14.38125909742180752, 17.55144818341503665, -39.01709431150898411 ) ) ;
#21762 = AXIS2_PLACEMENT_3D ( 'NONE', #3231, #9468, #17575 ) ;
#21764 = CARTESIAN_POINT ( 'NONE',  ( -135.8532207217289738, -6.472252184283586729, -50.09629031063973770 ) ) ;
#21763 = CARTESIAN_POINT ( 'NONE',  ( 146.6084372240433709, 24.48358557860356655, -32.08495691632035118 ) ) ;
#21765 = CARTESIAN_POINT ( 'NONE',  ( 57.59792236341147031, -1.722363176415055985, 1.722363176415024677 ) ) ;
#21766 = DIRECTION ( 'NONE',  ( 0.8802361161597901384, 0.000000000000000000, -0.4745359626076072757 ) ) ;
#21767 = CARTESIAN_POINT ( 'NONE',  ( 192.4448373802100889, -14.14213562375876698, -14.14213562375885047 ) ) ;
#21769 = CARTESIAN_POINT ( 'NONE',  ( -238.4067589809705794, -40.00000000000007105, 0.9644942799824426372 ) ) ;
#21768 = CARTESIAN_POINT ( 'NONE',  ( 91.82158438592158234, 16.11829626348378142, 40.45024623143977749 ) ) ;
#21770 = CARTESIAN_POINT ( 'NONE',  ( 136.1360204305621266, -3.511608612530682905, 3.511608612530666917 ) ) ;
#21771 = CARTESIAN_POINT ( 'NONE',  ( -198.0356074513804572, -10.87444709759714634, -10.87444709759729911 ) ) ;
#21772 = CARTESIAN_POINT ( 'NONE',  ( 0.2972598230769930017, 14.33493731733933352, 40.00000000000002132 ) ) ;
#21773 = VERTEX_POINT ( 'NONE', #1868 ) ;
#21774 = CARTESIAN_POINT ( 'NONE',  ( -198.0356074513804572, 10.87444709759714989, 10.87444709759722450 ) ) ;
#21775 = CARTESIAN_POINT ( 'NONE',  ( 1.066297917906484427, 43.20144851603839697, 17.89462588950527788 ) ) ;
#21776 = CARTESIAN_POINT ( 'NONE',  ( -348.0000000000001137, -4.467814962633844109E-14, -31.79780246617542616 ) ) ;
#21777 = CARTESIAN_POINT ( 'NONE',  ( 98.29820294267436509, 14.14213562374297695, -14.14213562372651189 ) ) ;
#21778 = VERTEX_POINT ( 'NONE', #22487 ) ;
#21779 = CARTESIAN_POINT ( 'NONE',  ( -188.3610564113329247, -43.02325945309097932, 23.46269903113408262 ) ) ;
#21780 = CARTESIAN_POINT ( 'NONE',  ( 200.0000000000000000, -18.09920287623689106, -5.808051173427421610 ) ) ;
#21781 = CARTESIAN_POINT ( 'NONE',  ( 67.90397382967701390, -10.29861769470937638, 30.27708616521051255 ) ) ;
#21782 = CARTESIAN_POINT ( 'NONE',  ( 22.50777602749652218, 17.91321921095766712, -43.24633676485946410 ) ) ;
#21783 = CARTESIAN_POINT ( 'NONE',  ( 199.0058364129993436, 9.132953877242854901, -17.78802470895853816 ) ) ;
#21784 = UNCERTAINTY_MEASURE_WITH_UNIT (LENGTH_MEASURE( 1.000000000000000082E-05 ), #17040, 'distance_accuracy_value', 'NONE');
#21785 = DIRECTION ( 'NONE',  ( 0.000000000000000000, 1.000000000000000000, 0.000000000000000000 ) ) ;
#21786 = CARTESIAN_POINT ( 'NONE',  ( -100.7734535825088500, 40.00000000000008527, -22.67402823373177512 ) ) ;
#21787 = CARTESIAN_POINT ( 'NONE',  ( -77.55640685868800688, -1.385213842686960017, 22.13135000840288313 ) ) ;
#21788 = DIRECTION ( 'NONE',  ( 1.000000000000000000, 1.836970198721030427E-16, -0.000000000000000000 ) ) ;
#21789 = CARTESIAN_POINT ( 'NONE',  ( 136.1360204305621551, -4.966164525587043244, 40.00000000000002132 ) ) ;
#21791 = FACE_BOUND ( 'NONE', #14815, .T. ) ;
#21790 = CARTESIAN_POINT ( 'NONE',  ( -185.5190930961335027, 17.55874694104972988, -42.39056500340850420 ) ) ;
#21792 = CARTESIAN_POINT ( 'NONE',  ( 98.29820294267396719, -17.94316440882807129, -8.858778887858122175 ) ) ;
#21793 = CARTESIAN_POINT ( 'NONE',  ( 0.2972598230769983307, -14.33493731733933352, 0.000000000000000000 ) ) ;
#21794 = CARTESIAN_POINT ( 'NONE',  ( 91.82158438592158234, -17.20528682183298486, 40.00000000000002132 ) ) ;
#21795 = CARTESIAN_POINT ( 'NONE',  ( 14.38125909742182529, -39.99999999999944578, -55.17850393971050238 ) ) ;
#21796 = CARTESIAN_POINT ( 'NONE',  ( 91.82158438592158234, -1.633484621919921769E-13, 17.20528682183300262 ) ) ;
#21797 = CARTESIAN_POINT ( 'NONE',  ( 151.7948205124836250, 23.49921654116328540, 23.49921654116366554 ) ) ;
#21798 = ORIENTED_EDGE ( 'NONE', *, *, #1588, .F. ) ;
#21799 = CARTESIAN_POINT ( 'NONE',  ( -109.1264249741451948, 33.12752917270486819, -13.72187187121119401 ) ) ;
#21800 = CARTESIAN_POINT ( 'NONE',  ( -56.48582580120559271, 9.153146818113576444, -0.000000000000000000 ) ) ;
#21801 = CARTESIAN_POINT ( 'NONE',  ( 57.59792236341147031, -1.722363176415055985, 1.722363176415024677 ) ) ;
#21802 = CARTESIAN_POINT ( 'NONE',  ( -86.86578273022546171, -8.153770686795279943, 19.68494377654078420 ) ) ;
#21803 = CONTEXT_DEPENDENT_SHAPE_REPRESENTATION ( #8486, #26343 ) ;
#21804 = ORIENTED_EDGE ( 'NONE', *, *, #1849, .T. ) ;
#21805 = ORIENTED_EDGE ( 'NONE', *, *, #1775, .T. ) ;
#21806 = CARTESIAN_POINT ( 'NONE',  ( -105.4741150117382915, -19.60045294982753461, 8.366608964593266862 ) ) ;
#21807 = CARTESIAN_POINT ( 'NONE',  ( 23.72853009152644788, -46.68009952139126995, -13.77482773664812221 ) ) ;
#21808 = ORIENTED_EDGE ( 'NONE', *, *, #13301, .F. ) ;
#21809 = CARTESIAN_POINT ( 'NONE',  ( -198.0356074513804572, 55.37879056874818673, -40.00000000000002132 ) ) ;
#21810 = CARTESIAN_POINT ( 'NONE',  ( -94.58360650939697223, -20.91945674498037278, 8.190527749779679567 ) ) ;
#21811 = ADVANCED_FACE ( 'NONE', ( #12097 ), #24212, .F. ) ;
#21812 = ORIENTED_EDGE ( 'NONE', *, *, #15991, .T. ) ;
#21813 = CARTESIAN_POINT ( 'NONE',  ( 199.9999999999996305, -4.934527571401590151, 18.35877764772902410 ) ) ;
#21814 = LINE ( 'NONE', #1087, #20045 ) ;
#21815 = CARTESIAN_POINT ( 'NONE',  ( -105.3755690713226585, 41.18208027870598187, -15.38646221621779731 ) ) ;
#21816 = EDGE_CURVE ( 'NONE', #4168, #5362, #19946, .T. ) ;
#21817 = CARTESIAN_POINT ( 'NONE',  ( -200.0000000000000284, 30.70179486994630835, -44.88127304974036491 ) ) ;
#21818 = CARTESIAN_POINT ( 'NONE',  ( 130.8568914410475372, 1.429239637432775288E-13, -34.05028731879788495 ) ) ;
#21819 = CARTESIAN_POINT ( 'NONE',  ( -192.9588430854689989, 38.51493924976983152, -38.51493924976893624 ) ) ;
#21820 = DIRECTION ( 'NONE',  ( -1.000000000000000000, -0.000000000000000000, -0.000000000000000000 ) ) ;
#21821 = ADVANCED_FACE ( 'NONE', ( #12229 ), #2259, .T. ) ;
#21822 = EDGE_CURVE ( 'NONE', #16552, #24210, #14091, .T. ) ;
#21823 = LINE ( 'NONE', #19822, #25041 ) ;
#21824 = CARTESIAN_POINT ( 'NONE',  ( 163.1118516004056573, -2.556006622855449647E-13, 27.26290988616872824 ) ) ;
#21825 = CARTESIAN_POINT ( 'NONE',  ( -208.1127848780265026, 1.189126717069624012E-13, -15.00245453012669472 ) ) ;
#21826 = CARTESIAN_POINT ( 'NONE',  ( -200.0000000000000000, -44.98788141756672587, -22.84381638316556717 ) ) ;
#21827 = CARTESIAN_POINT ( 'NONE',  ( -198.0356074513804572, -39.15871834505905724, -17.40982414986491733 ) ) ;
#21828 = CARTESIAN_POINT ( 'NONE',  ( -238.4067589809705794, -0.9644942799826263791, -40.00000000000002132 ) ) ;
#21829 = CARTESIAN_POINT ( 'NONE',  ( 200.0000000000000000, -42.42640687119269671, -14.14213562373124766 ) ) ;
#21830 = CARTESIAN_POINT ( 'NONE',  ( -83.21262154144251610, 13.72187187061548741, -33.12752917118393015 ) ) ;
#21831 = CIRCLE ( 'NONE', #21540, 31.79780246617542616 ) ;
#21832 = CARTESIAN_POINT ( 'NONE',  ( 98.29820294268191105, -7.653668647302825256, -18.47759065022797031 ) ) ;
#21833 = CARTESIAN_POINT ( 'NONE',  ( -86.96347745069645896, 39.99999999999977973, 21.75974354311691883 ) ) ;
#21834 = CARTESIAN_POINT ( 'NONE',  ( -213.1075012329537230, -40.00000000000025580, 53.71589010953650956 ) ) ;
#21835 = CARTESIAN_POINT ( 'NONE',  ( -192.9588430854690273, 10.23066800231970319, 66.79921049724369198 ) ) ;
#21836 = CARTESIAN_POINT ( 'NONE',  ( 200.0000000000000000, -14.14213562373122457, 42.42640687119282461 ) ) ;
#21837 = CARTESIAN_POINT ( 'NONE',  ( -188.2652746676490096, -13.82569223135675607, -46.97858116094653269 ) ) ;
#21838 = CARTESIAN_POINT ( 'NONE',  ( 163.1118516004056573, 19.27778845538780317, -19.27778845538757224 ) ) ;
#21839 = VERTEX_POINT ( 'NONE', #8232 ) ;
#21840 = CARTESIAN_POINT ( 'NONE',  ( -208.1127848780264742, 10.60833733268383483, -67.17687982760675425 ) ) ;
#21841 = CARTESIAN_POINT ( 'NONE',  ( -56.48582580120559271, 9.153146818113576444, -0.000000000000000000 ) ) ;
#21842 = CARTESIAN_POINT ( 'NONE',  ( -350.0000000000001137, -4.857225732735059864E-14, 0.000000000000000000 ) ) ;
#21843 = CARTESIAN_POINT ( 'NONE',  ( 192.4448373802100889, 14.14213562370330379, -14.14213562370292365 ) ) ;
#21844 = CARTESIAN_POINT ( 'NONE',  ( -87.12809909138003661, 1.359879344810606350, 21.45715697400068578 ) ) ;
#21845 = ORIENTED_EDGE ( 'NONE', *, *, #13214, .T. ) ;
#21846 = CARTESIAN_POINT ( 'NONE',  ( -626.9846540392097722, 75.00000000000000000, 54.99999999999995737 ) ) ;
#21847 = CARTESIAN_POINT ( 'NONE',  ( 199.0255387882960747, -18.58171137233306780, 7.410670782471526330 ) ) ;
#21848 = CARTESIAN_POINT ( 'NONE',  ( -4.558244102844902557, 13.79151199599537669, 46.81081390833295330 ) ) ;
#21849 = ORIENTED_EDGE ( 'NONE', *, *, #4630, .F. ) ;
#21850 = ORIENTED_EDGE ( 'NONE', *, *, #17579, .T. ) ;
#21851 = CARTESIAN_POINT ( 'NONE',  ( 130.8568914410475088, 5.949712681206719367, -40.00000000000002132 ) ) ;
#21852 = CARTESIAN_POINT ( 'NONE',  ( -280.0000000000000000, 14.14213562373098299, -14.14213562373088706 ) ) ;
#21853 = CARTESIAN_POINT ( 'NONE',  ( -213.1075012329537230, 39.99999999999979394, 53.71589010950180665 ) ) ;
#21854 = CARTESIAN_POINT ( 'NONE',  ( -96.94475454970458372, -20.92018922306581530, -8.190683501986224968 ) ) ;
#21855 = EDGE_CURVE ( 'NONE', #5488, #21418, #6245, .T. ) ;
#21856 = CARTESIAN_POINT ( 'NONE',  ( 14.38125909742181108, 39.01709431150961649, -39.01709431150867147 ) ) ;
#21857 = CARTESIAN_POINT ( 'NONE',  ( 130.8568914410475088, 39.99999999999969447, 34.05028731879830417 ) ) ;
#21858 = CARTESIAN_POINT ( 'NONE',  ( 199.9999999999999716, -14.18957598410689869, 12.65210747703644500 ) ) ;
#21859 = DIRECTION ( 'NONE',  ( 0.000000000000000000, 1.000000000000000000, 0.000000000000000000 ) ) ;
#21860 = CARTESIAN_POINT ( 'NONE',  ( -3.977426076247836839, -17.87762021094878406, -43.16039317622803395 ) ) ;
#21861 = CARTESIAN_POINT ( 'NONE',  ( -192.9588430854690273, 18.05360324515473280, -38.51493924976924177 ) ) ;
#21862 = CARTESIAN_POINT ( 'NONE',  ( 151.7948205124836250, -23.49921654116371883, 23.49921654116317526 ) ) ;
#21863 = CARTESIAN_POINT ( 'NONE',  ( 91.82158438592156813, -16.11829626348402655, -40.45024623143966380 ) ) ;
#21864 = CARTESIAN_POINT ( 'NONE',  ( 200.0000000000000000, -40.00000000000019185, 19.99999999999968381 ) ) ;
#21865 = CARTESIAN_POINT ( 'NONE',  ( -105.2274517607688011, -21.34875776644186374, -2.715151009218549127 ) ) ;
#21866 = CARTESIAN_POINT ( 'NONE',  ( 91.82158438592158234, 17.20528682183301683, 0.000000000000000000 ) ) ;
#21867 = CARTESIAN_POINT ( 'NONE',  ( -100.7734535825088358, -17.32597176626813251, -2.449293598294708485E-15 ) ) ;
#21868 = CARTESIAN_POINT ( 'NONE',  ( 130.8568914410475372, 24.07718906447243867, -24.07718906447216156 ) ) ;
#21869 = CARTESIAN_POINT ( 'NONE',  ( -280.0000000000000568, -20.00000000000006395, -40.00000000000002132 ) ) ;
#21870 = DIRECTION ( 'NONE',  ( 0.9698969544411792931, 0.09318942517728809327, 0.2249791741491908026 ) ) ;
#21871 = CARTESIAN_POINT ( 'NONE',  ( -114.7484189202600930, 21.94394827837179918, 2.980060266884688946 ) ) ;
#21872 = CARTESIAN_POINT ( 'NONE',  ( -86.96347745069644475, 41.18208027870598187, -15.38646221621779731 ) ) ;
#21873 = CARTESIAN_POINT ( 'NONE',  ( 136.1360204305621551, 4.966164525587085876, 40.00000000000002132 ) ) ;
#21874 = EDGE_LOOP ( 'NONE', ( #11652, #17076 ) ) ;
#21875 =( BOUNDED_CURVE ( )  B_SPLINE_CURVE ( 3, ( #24775, #2823, #12924, #10526 ),
 .UNSPECIFIED., .F., .T. ) 
 B_SPLINE_CURVE_WITH_KNOTS ( ( 4, 4 ),
 ( 0.01388163286937179816, 0.02359082919310010601 ),
 .UNSPECIFIED. ) 
 CURVE ( )  GEOMETRIC_REPRESENTATION_ITEM ( )  RATIONAL_B_SPLINE_CURVE ( ( 1.000000000000000000, 0.8672072324488975248, 0.7608653435686167921, 0.6809743333591576908 ) ) 
 REPRESENTATION_ITEM ( '' )  );
#21876 = CYLINDRICAL_SURFACE ( 'NONE', #5679, 5.000000000000039080 ) ;
#21877 = DIRECTION ( 'NONE',  ( 0.000000000000000000, 1.000000000000000000, 0.000000000000000000 ) ) ;
#21878 = CARTESIAN_POINT ( 'NONE',  ( -135.8532207217289738, 21.81201906317777883, -34.75652343174605363 ) ) ;
#21879 = CARTESIAN_POINT ( 'NONE',  ( 146.6084372240433709, -40.00000000000001421, 5.374981219216829587 ) ) ;
#21880 = AXIS2_PLACEMENT_3D ( 'NONE', #14702, #16963, #22833 ) ;
#21881 = CARTESIAN_POINT ( 'NONE',  ( -280.0000000000000000, -14.14213562373118549, 14.14213562373078936 ) ) ;
#21882 = CARTESIAN_POINT ( 'NONE',  ( -238.4067589809705794, 0.9644942799825386714, 0.000000000000000000 ) ) ;
#21883 = CARTESIAN_POINT ( 'NONE',  ( 136.1360204305621551, 4.966164525587093870, -40.00000000000002132 ) ) ;
#21884 = CARTESIAN_POINT ( 'NONE',  ( -188.2995950289364089, -43.00522595870943832, -23.44932284466036521 ) ) ;
#21885 = CARTESIAN_POINT ( 'NONE',  ( 199.9999999999998863, -9.643221244315762775, 16.38360543750208009 ) ) ;
#21886 = CARTESIAN_POINT ( 'NONE',  ( 199.9999999999998863, -18.28231079023461092, -5.210528357603022798 ) ) ;
#21887 = CARTESIAN_POINT ( 'NONE',  ( -238.4067589809705794, 28.96627169325285678, 27.60227080167094726 ) ) ;
#21888 = CARTESIAN_POINT ( 'NONE',  ( 91.82158438592159655, 12.16597498400091304, -44.40256751092321963 ) ) ;
#21889 = AXIS2_PLACEMENT_3D ( 'NONE', #7333, #5351, #13210 ) ;
#21890 = CARTESIAN_POINT ( 'NONE',  ( 4.995406935893293543, -10.78321810389005364, 10.78321810388994173 ) ) ;
#21891 = CARTESIAN_POINT ( 'NONE',  ( -77.65695844553741267, 18.42387585929312976, -12.10528775143868252 ) ) ;
#21892 = CARTESIAN_POINT ( 'NONE',  ( -198.0356074513804288, -39.15871834505882276, -39.15871834505946936 ) ) ;
#21894 = CARTESIAN_POINT ( 'NONE',  ( 4.995406935893294431, -17.50105314357144337, -39.06748935135212264 ) ) ;
#21893 = CARTESIAN_POINT ( 'NONE',  ( 0.2972598230770100991, -38.42060263243632079, -38.42060263243699580 ) ) ;
#21895 = CARTESIAN_POINT ( 'NONE',  ( 91.82158438592158234, -40.45024623143936537, -16.11829626348475131 ) ) ;
#21896 = CARTESIAN_POINT ( 'NONE',  ( 136.1360204305621266, -35.03383547441293899, 0.000000000000000000 ) ) ;
#21897 = DIRECTION ( 'NONE',  ( 0.000000000000000000, 0.000000000000000000, 1.000000000000000000 ) ) ;
#21899 = CARTESIAN_POINT ( 'NONE',  ( 136.1360204305621266, 1.473277640373554421E-13, -35.03383547441296741 ) ) ;
#21898 = CARTESIAN_POINT ( 'NONE',  ( 0.2972598230769886718, 38.42060263243643448, 18.14793986248763957 ) ) ;
#21900 = CARTESIAN_POINT ( 'NONE',  ( -86.96347745069645896, 43.67073346367970288, 12.89780903124427702 ) ) ;
#21901 = AXIS2_PLACEMENT_3D ( 'NONE', #6968, #21087, #2735 ) ;
#21902 = CARTESIAN_POINT ( 'NONE',  ( 151.7948205124836250, 23.49921654116328540, 23.49921654116366554 ) ) ;
#21903 = VECTOR ( 'NONE', #4020, 1000.000000000000000 ) ;
#21904 = CARTESIAN_POINT ( 'NONE',  ( 57.59792236341147031, -2.435789363418150000, 40.00000000000002132 ) ) ;
#21906 = EDGE_CURVE ( 'NONE', #16549, #7651, #16219, .T. ) ;
#21905 = VERTEX_POINT ( 'NONE', #15809 ) ;
#21907 = CARTESIAN_POINT ( 'NONE',  ( -100.7734535825088500, 12.25131212657490209, -44.31723036834897300 ) ) ;
#21908 = CARTESIAN_POINT ( 'NONE',  ( -63.45572741887768586, 25.09195535024256785, 10.39342821253069893 ) ) ;
#21909 = CARTESIAN_POINT ( 'NONE',  ( -626.9846540392142060, 28.28427124746186649, 34.99999999999999289 ) ) ;
#21910 = CARTESIAN_POINT ( 'NONE',  ( -198.0356074513804572, 15.37879056873067007, 0.000000000000000000 ) ) ;
#21911 = EDGE_CURVE ( 'NONE', #24911, #10231, #10534, .T. ) ;
#21912 = AXIS2_PLACEMENT_3D ( 'NONE', #19750, #26163, #16023 ) ;
#21913 = VERTEX_POINT ( 'NONE', #19018 ) ;
#21914 = AXIS2_PLACEMENT_3D ( 'NONE', #19558, #9576, #26096 ) ;
#21915 = CARTESIAN_POINT ( 'NONE',  ( -3.762763306026911447, 23.50897034858851242, -43.08566851766582317 ) ) ;
#21916 = CARTESIAN_POINT ( 'NONE',  ( 200.0000000000000000, -19.00702131438069031, 0.3144861700050793352 ) ) ;
#21917 = CARTESIAN_POINT ( 'NONE',  ( -4.022465846214220875, -23.45302613997613861, 43.01021959554137908 ) ) ;
#21918 = EDGE_CURVE ( 'NONE', #19515, #60, #9838, .T. ) ;
#21919 = EDGE_CURVE ( 'NONE', #23643, #17137, #3460, .T. ) ;
#21920 = CARTESIAN_POINT ( 'NONE',  ( 16.38602454705335276, 24.50452114746028087, -44.43226271088839496 ) ) ;
#21921 = CARTESIAN_POINT ( 'NONE',  ( 199.0070393743141892, 19.55016766319115007, -4.199986046643529924 ) ) ;
#21922 = AXIS2_PLACEMENT_3D ( 'NONE', #17071, #9215, #7211 ) ;
#21923 = DIRECTION ( 'NONE',  ( -1.000000000000000000, -0.000000000000000000, -0.000000000000000000 ) ) ;
#21924 = CARTESIAN_POINT ( 'NONE',  ( -121.8281150759179212, -8.694016608775745780, 23.07023398738753173 ) ) ;
#21925 = CARTESIAN_POINT ( 'NONE',  ( 14.38125909742181108, 39.01709431150961649, -39.01709431150867147 ) ) ;
#21926 = CARTESIAN_POINT ( 'NONE',  ( -91.56559293963836410, 22.67402823373190301, 40.00000000000002132 ) ) ;
#21928 = CARTESIAN_POINT ( 'NONE',  ( -238.4067589809705794, 0.9644942799825386714, 0.000000000000000000 ) ) ;
#21927 = CARTESIAN_POINT ( 'NONE',  ( 44.82887508592131098, -18.94256811217822900, -36.15717056695913101 ) ) ;
#21929 = CARTESIAN_POINT ( 'NONE',  ( -162.0762913951020892, 1.198031840385732849, -1.198031840385733515 ) ) ;
#21930 = CARTESIAN_POINT ( 'NONE',  ( 151.7948205124836250, 33.23291073765556547, 0.000000000000000000 ) ) ;
#21931 = CARTESIAN_POINT ( 'NONE',  ( -208.1127848780265026, 15.00245453012665564, 0.000000000000000000 ) ) ;
#21932 = CARTESIAN_POINT ( 'NONE',  ( 146.6084372240433709, -39.99999999999993605, -5.374981219217395356 ) ) ;
#21933 = CARTESIAN_POINT ( 'NONE',  ( 98.29820294267355507, -10.02182676110716208, 17.32045324916611406 ) ) ;
#21934 = CARTESIAN_POINT ( 'NONE',  ( -135.8532207217289738, 6.472252184284096543, 6.472252184284234211 ) ) ;
#21935 = EDGE_LOOP ( 'NONE', ( #7687, #8030 ) ) ;
#21936 = CARTESIAN_POINT ( 'NONE',  ( -190.0000000000000000, -52.49999999999972289, -82.49999999999998579 ) ) ;
#21937 = CARTESIAN_POINT ( 'NONE',  ( -100.7734535825088500, 22.67402823373189591, -0.000000000000000000 ) ) ;
#21938 = CARTESIAN_POINT ( 'NONE',  ( -102.4309680866254268, -8.087567261749121883, 20.43798635335615899 ) ) ;
#21939 = EDGE_LOOP ( 'NONE', ( #1333, #21458, #2119, #733 ) ) ;
#21940 = ORIENTED_EDGE ( 'NONE', *, *, #16145, .F. ) ;
#21941 = VECTOR ( 'NONE', #25634, 1000.000000000000000 ) ;
#21942 = CARTESIAN_POINT ( 'NONE',  ( 19.06497207195981858, -38.31983398719616218, -18.24870850772777331 ) ) ;
#21943 = CARTESIAN_POINT ( 'NONE',  ( 44.65795722955357405, -36.73450905827150592, -15.21593185916488622 ) ) ;
#21944 = ORIENTED_EDGE ( 'NONE', *, *, #15341, .F. ) ;
#21945 = CARTESIAN_POINT ( 'NONE',  ( -30.26275506840324425, 41.69427246844628598, -40.00000000000002132 ) ) ;
#21946 = DIRECTION ( 'NONE',  ( 1.000000000000000000, 1.836970198721030181E-16, 0.000000000000000000 ) ) ;
#21947 = EDGE_LOOP ( 'NONE', ( #5583, #19164, #25710, #16081, #13676, #14647, #11554 ) ) ;
#21948 = CARTESIAN_POINT ( 'NONE',  ( 200.0000000000000853, 18.51119012207909620, 4.337730402235636440 ) ) ;
#21949 = CARTESIAN_POINT ( 'NONE',  ( -210.0000000000000284, -52.49999999999991473, 82.49999999999998579 ) ) ;
#21950 = CARTESIAN_POINT ( 'NONE',  ( 200.0000000000000000, -14.14213562373106114, 42.42640687119278908 ) ) ;
#21951 = CARTESIAN_POINT ( 'NONE',  ( -199.9999999999998579, 44.86878812508723513, -24.82633483071237634 ) ) ;
#21952 = CIRCLE ( 'NONE', #3268, 74.99999999999995737 ) ;
#21953 = CIRCLE ( 'NONE', #7485, 5.000000000000004441 ) ;
#21954 = CARTESIAN_POINT ( 'NONE',  ( -162.0762913951020892, -3.568845385355699554E-14, 1.694272876828323948 ) ) ;
#21955 = CARTESIAN_POINT ( 'NONE',  ( 163.1118516004056573, -27.26290988616869626, 0.000000000000000000 ) ) ;
#21956 = CARTESIAN_POINT ( 'NONE',  ( 200.0000000000000000, 42.42640687119267540, 14.14213562373153543 ) ) ;
#21957 = CARTESIAN_POINT ( 'NONE',  ( 190.0000000000000284, -82.49999999999991473, -52.49999999999977973 ) ) ;
#21958 = CARTESIAN_POINT ( 'NONE',  ( -105.3755690713226727, 5.661656051307470077E-14, -21.75974354311649961 ) ) ;
#21959 = CARTESIAN_POINT ( 'NONE',  ( -135.8532207217289738, -1.208299557080134822E-13, 9.153146818113572891 ) ) ;
#21960 = CARTESIAN_POINT ( 'NONE',  ( 170.0000000000000284, -6.285860131565133457, -24.25569233607183506 ) ) ;
#21961 = CARTESIAN_POINT ( 'NONE',  ( 136.1360204305621266, -3.511608612530682905, 3.511608612530666917 ) ) ;
#21962 = CARTESIAN_POINT ( 'NONE',  ( 14.38125909742181285, -15.17850393972633505, -40.00000000000002132 ) ) ;
#21963 = CARTESIAN_POINT ( 'NONE',  ( -213.1075012329537230, -66.26714140138676612, 9.698598906462487790 ) ) ;
#21964 = CARTESIAN_POINT ( 'NONE',  ( -726.9846540392142060, -82.49999999999991473, -52.49999999999977973 ) ) ;
#21965 = ADVANCED_FACE ( 'NONE', ( #23020 ), #258, .T. ) ;
#21966 = B_SPLINE_CURVE_WITH_KNOTS ( 'NONE', 3,
 ( #17929, #7421, #25805, #23540, #3447, #13940, #5696, #13801 ),
 .UNSPECIFIED., .F., .F.,
 ( 4, 2, 2, 4 ),
 ( -5.298247996737306503E-05, 0.001923793760064214722, 0.003900570000095802611, 0.007854122480158971450 ),
 .UNSPECIFIED. ) ;
#21967 = CARTESIAN_POINT ( 'NONE',  ( -1.818469002956083935, -47.72215409237453088, 13.93708913181261799 ) ) ;
#21968 = CARTESIAN_POINT ( 'NONE',  ( 146.6084372240433993, -3.357462877844280890E-13, 34.62501878078305850 ) ) ;
#21969 = CARTESIAN_POINT ( 'NONE',  ( 0.2972598230770030492, -40.00000000000007816, 14.33493731733919496 ) ) ;
#21970 = CARTESIAN_POINT ( 'NONE',  ( -30.26275506840325136, 57.76657404653985139, 1.198031551616126178 ) ) ;
#21971 = CARTESIAN_POINT ( 'NONE',  ( -86.96347745069644475, 15.38646221621772092, 15.38646221621800336 ) ) ;
#21972 = CARTESIAN_POINT ( 'NONE',  ( -188.8753834511965692, -17.93496043754474556, -43.29882472894647094 ) ) ;
#21973 = CARTESIAN_POINT ( 'NONE',  ( 170.0000000000000000, -2.301191124287261779E-13, 24.95097643317000546 ) ) ;
#21974 = VERTEX_POINT ( 'NONE', #25015 ) ;
#21975 = CARTESIAN_POINT ( 'NONE',  ( 130.8568914410475088, -24.07718906446864793, -32.49135343045505664 ) ) ;
#21976 = CARTESIAN_POINT ( 'NONE',  ( 130.8568914410475372, 24.07718906447243867, -24.07718906447216156 ) ) ;
#21977 = CARTESIAN_POINT ( 'NONE',  ( -30.26275506840324070, -1.694272468446265112, 0.000000000000000000 ) ) ;
#21978 = CIRCLE ( 'NONE', #4934, 10.00000000000004796 ) ;
#21979 = CARTESIAN_POINT ( 'NONE',  ( -87.13361725327071383, 16.19487519257939212, 14.20112123283741745 ) ) ;
#21980 = CARTESIAN_POINT ( 'NONE',  ( -259.2033419157646676, -6.730120644402966867, -49.83842185052038332 ) ) ;
#21981 = B_SPLINE_CURVE_WITH_KNOTS ( 'NONE', 3,
 ( #18026, #1420, #23753, #7643, #23507, #15758 ),
 .UNSPECIFIED., .F., .F.,
 ( 4, 2, 4 ),
 ( 0.0003134551847831237793, 0.004478723513730584541, 0.008643991842678043838 ),
 .UNSPECIFIED. ) ;
#21982 = CARTESIAN_POINT ( 'NONE',  ( 23.37394308801977871, -42.85717664514601921, 23.33966569535066071 ) ) ;
#21983 = ORIENTED_EDGE ( 'NONE', *, *, #9254, .F. ) ;
#21984 = CARTESIAN_POINT ( 'NONE',  ( 199.9999999999999147, 18.82040333305158342, 2.653950712460805494 ) ) ;
#21985 = ADVANCED_FACE ( 'NONE', ( #12626 ), #17898, .T. ) ;
#21986 = CARTESIAN_POINT ( 'NONE',  ( -105.2502153031278880, -17.39736479739720920, 12.58638139385545607 ) ) ;
#21987 = CARTESIAN_POINT ( 'NONE',  ( -3.417371742524983880, 17.93997298316174493, 43.31092608455620763 ) ) ;
#21988 = B_SPLINE_CURVE_WITH_KNOTS ( 'NONE', 3,
 ( #24789, #4963, #25056, #21187, #8945, #6543, #12938, #21053 ),
 .UNSPECIFIED., .F., .F.,
 ( 4, 2, 2, 4 ),
 ( 1.822044248639793593E-14, 0.002116768774648846146, 0.004233537549279472491, 0.008467075098540726916 ),
 .UNSPECIFIED. ) ;
#21989 = VERTEX_POINT ( 'NONE', #8770 ) ;
#21990 = ORIENTED_EDGE ( 'NONE', *, *, #532, .F. ) ;
#21991 = CARTESIAN_POINT ( 'NONE',  ( -105.3755690713226727, -15.38646221621786481, -15.38646221621789856 ) ) ;
#21992 = CARTESIAN_POINT ( 'NONE',  ( 199.0134806391063194, -10.42534412885540185, -17.06722571675988931 ) ) ;
#21993 = CARTESIAN_POINT ( 'NONE',  ( -208.1127848780264742, 39.99999999999979394, 55.00245453010936103 ) ) ;
#21994 = ADVANCED_BREP_SHAPE_REPRESENTATION ( '', ( #8606, #21058 ), #17620 ) ;
#21995 = SURFACE_STYLE_USAGE ( .BOTH. , #13861 ) ;
#21996 = DIRECTION ( 'NONE',  ( 0.000000000000000000, -1.000000000000000000, 0.000000000000000000 ) ) ;
#21997 = CARTESIAN_POINT ( 'NONE',  ( -86.96347745069644475, -2.438961472018186339E-13, 21.75974354311649961 ) ) ;
#21998 = CARTESIAN_POINT ( 'NONE',  ( 199.9999999999998579, -18.51658467707331113, 4.312655811444462195 ) ) ;
#21999 = CARTESIAN_POINT ( 'NONE',  ( -190.0000000000000000, -52.49999999999970868, 82.49999999999998579 ) ) ;
#22000 = DIRECTION ( 'NONE',  ( 0.000000000000000000, 0.000000000000000000, -1.000000000000000000 ) ) ;
#22001 = CARTESIAN_POINT ( 'NONE',  ( 199.0242446922718784, -2.616032970993653173, 19.83497009005848710 ) ) ;
#22002 = CARTESIAN_POINT ( 'NONE',  ( -83.21262154144251610, -33.12752917118416462, -13.72187187061499536 ) ) ;
#22003 = CARTESIAN_POINT ( 'NONE',  ( -3.417371742523256373, -17.93997298316167033, -43.31092608455676185 ) ) ;
#22004 = CARTESIAN_POINT ( 'NONE',  ( 91.82158438592159655, -16.11829626346125011, -16.11829626346154853 ) ) ;
#22005 = EDGE_CURVE ( 'NONE', #4130, #3826, #20754, .T. ) ;
#22006 = CARTESIAN_POINT ( 'NONE',  ( -105.3841681040961475, -20.33889746609128579, 6.699016078410943820 ) ) ;
#22007 = CARTESIAN_POINT ( 'NONE',  ( -135.8532207217289738, -21.81201906317788186, 21.81201906317762962 ) ) ;
#22008 = CARTESIAN_POINT ( 'NONE',  ( -86.96347745069643054, -40.00000000000026290, 21.75974354311608749 ) ) ;
#22009 = DIRECTION ( 'NONE',  ( -1.303213150798907793E-16, 1.000000000000000000, -1.682156097916904081E-16 ) ) ;
#22010 = CARTESIAN_POINT ( 'NONE',  ( 192.4448373802100889, 14.14213562375873678, 14.14213562375894817 ) ) ;
#22011 = CARTESIAN_POINT ( 'NONE',  ( 192.4448373802100889, -19.99999999996057198, -2.449293598294708485E-15 ) ) ;
#22012 = CARTESIAN_POINT ( 'NONE',  ( -100.7734535825088500, 44.31723036834890905, 12.25131212657507795 ) ) ;
#22013 = CARTESIAN_POINT ( 'NONE',  ( 163.1118516004056573, -12.73709011382471878, -40.00000000000002132 ) ) ;
#22014 = CARTESIAN_POINT ( 'NONE',  ( -105.2599799664448312, 17.55584898455461840, 12.33876530776534786 ) ) ;
#22015 = CARTESIAN_POINT ( 'NONE',  ( -208.1127848780265026, 1.189126717069624012E-13, -15.00245453012669472 ) ) ;
#22016 = ADVANCED_FACE ( 'NONE', ( #4796 ), #11124, .T. ) ;
#22017 = CARTESIAN_POINT ( 'NONE',  ( -213.1075012329537230, 9.698598906450410340, 9.698598906450483170 ) ) ;
#22018 = EDGE_CURVE ( 'NONE', #16948, #8230, #24190, .T. ) ;
#22019 = CARTESIAN_POINT ( 'NONE',  ( -162.0762913951020892, 1.694272876828294194, 0.000000000000000000 ) ) ;
#22020 = EDGE_LOOP ( 'NONE', ( #7822, #255, #25206, #25144, #17293 ) ) ;
#22021 = CARTESIAN_POINT ( 'NONE',  ( 22.86726691379450926, -43.14849715852140122, 17.87269271907627655 ) ) ;
#22022 = FACE_OUTER_BOUND ( 'NONE', #11591, .T. ) ;
#22023 = CARTESIAN_POINT ( 'NONE',  ( 146.6084372240433709, 32.08495691632064961, -24.48358557860320417 ) ) ;
#22024 = CARTESIAN_POINT ( 'NONE',  ( 170.2234770963711128, -39.99999999999991473, -24.55285855007201334 ) ) ;
#22025 = CARTESIAN_POINT ( 'NONE',  ( 163.1118516004056573, -19.27778845538787422, 19.27778845538743724 ) ) ;
#22026 = CARTESIAN_POINT ( 'NONE',  ( 163.1118516004056573, -27.26290988616869626, 0.000000000000000000 ) ) ;
#22027 = CARTESIAN_POINT ( 'NONE',  ( -100.7734535825088358, -22.67402823373193499, 0.000000000000000000 ) ) ;
#22028 = DIRECTION ( 'NONE',  ( 1.298934084353256076E-16, -0.7071067811865561215, 0.7071067811865389130 ) ) ;
#22029 = CARTESIAN_POINT ( 'NONE',  ( 199.9999999999998863, 18.88157209772827017, -2.150785294275829429 ) ) ;
#22030 = CARTESIAN_POINT ( 'NONE',  ( 200.0000000000000000, -15.45605508098274861, -11.06530458668214933 ) ) ;
#22031 = CARTESIAN_POINT ( 'NONE',  ( -213.1075012329537230, 37.98287015391280619, -37.98287015391192512 ) ) ;
#22032 = CARTESIAN_POINT ( 'NONE',  ( -56.48582580120558561, -50.09629031063971638, 6.472252184283745713 ) ) ;
#22033 = CARTESIAN_POINT ( 'NONE',  ( -188.2995950289364941, -13.82811170417257607, 46.99046209955427855 ) ) ;
#22034 = CARTESIAN_POINT ( 'NONE',  ( -82.23729782343656325, 15.18297044031445431, -13.37626936639568598 ) ) ;
#22035 = CARTESIAN_POINT ( 'NONE',  ( -192.9588430854689705, -38.51493924976909966, -38.51493924976973915 ) ) ;
#22036 = B_SPLINE_CURVE_WITH_KNOTS ( 'NONE', 3,
 ( #11990, #2028, #9498, #14383, #20380, #3385 ),
 .UNSPECIFIED., .F., .F.,
 ( 4, 2, 4 ),
 ( 0.000000000000000000, 0.004519197161541735688, 0.009038394323083471377 ),
 .UNSPECIFIED. ) ;
#22038 = CARTESIAN_POINT ( 'NONE',  ( -53.37769371643646110, 10.11111068829013249, 29.42719939405408169 ) ) ;
#22037 = CARTESIAN_POINT ( 'NONE',  ( 146.6084372240433993, -3.800685668858596156, -3.800685668858692967 ) ) ;
#22039 = CARTESIAN_POINT ( 'NONE',  ( -91.56559293963834989, -16.03295912088728414, 16.03295912088688269 ) ) ;
#22040 = LINE ( 'NONE', #5534, #6186 ) ;
#22041 = CARTESIAN_POINT ( 'NONE',  ( 199.0231640206657460, 0.4968506554899906891, 19.99832409911510211 ) ) ;
#22042 = AXIS2_PLACEMENT_3D ( 'NONE', #19893, #1678, #24153 ) ;
#22044 = CARTESIAN_POINT ( 'NONE',  ( -208.1127848780264742, -40.00000000000011369, 15.00245453012655439 ) ) ;
#22043 = CARTESIAN_POINT ( 'NONE',  ( -198.0356074513804572, 67.44298959250878056, -10.87444709758402261 ) ) ;
#22045 = CARTESIAN_POINT ( 'NONE',  ( -259.2033419157646676, 6.730120644403521979, -6.730120644403498886 ) ) ;
#22046 = CARTESIAN_POINT ( 'NONE',  ( -135.8532207217289738, -6.472252184284280396, 6.472252184284099208 ) ) ;
#22047 = CARTESIAN_POINT ( 'NONE',  ( 4.995406935893288214, 55.24977328853207581, 40.00000000000002132 ) ) ;
#22048 = ORIENTED_EDGE ( 'NONE', *, *, #24365, .F. ) ;
#22049 = DIRECTION ( 'NONE',  ( 0.000000000000000000, 1.000000000000000000, 0.000000000000000000 ) ) ;
#22050 = CARTESIAN_POINT ( 'NONE',  ( 2.985930184390671371, 43.42223633017472650, 17.98607919652674170 ) ) ;
#22051 = CARTESIAN_POINT ( 'NONE',  ( 60.14720761598005083, 10.94158980372334078, 33.22245024487595089 ) ) ;
#22052 = CARTESIAN_POINT ( 'NONE',  ( -105.2274517607689290, -2.715151009219458622, 21.34875776644108569 ) ) ;
#22053 = VERTEX_POINT ( 'NONE', #8900 ) ;
#22054 = CARTESIAN_POINT ( 'NONE',  ( -190.7345856381647877, -47.78725959878028107, 13.94676320011207515 ) ) ;
#22055 = CARTESIAN_POINT ( 'NONE',  ( 199.9999999999998863, -18.14641137086378819, -5.658975142792487922 ) ) ;
#22056 = CARTESIAN_POINT ( 'NONE',  ( 17.91733029164682023, -14.04577174279065943, 48.44632265249130398 ) ) ;
#22057 = CIRCLE ( 'NONE', #4222, 69.99999999999992895 ) ;
#22058 = CARTESIAN_POINT ( 'NONE',  ( 22.01478053666848211, 13.87318432395317203, -47.29427690643910154 ) ) ;
#22059 = CARTESIAN_POINT ( 'NONE',  ( 199.0174211633917878, -15.97280307358279039, -12.03849830368706009 ) ) ;
#22060 = AXIS2_PLACEMENT_3D ( 'NONE', #10082, #18186, #26337 ) ;
#22061 = CARTESIAN_POINT ( 'NONE',  ( -626.9846540392097722, 75.00000000000000000, 54.99999999999995737 ) ) ;
#22062 = CARTESIAN_POINT ( 'NONE',  ( -151.4802930567624912, -11.09498731346505451, 33.96623840860532084 ) ) ;
#22063 = CARTESIAN_POINT ( 'NONE',  ( -105.3755690713226727, 12.89780903124418998, -12.89780903124389155 ) ) ;
#22064 = CARTESIAN_POINT ( 'NONE',  ( -192.9588430854690273, -54.46834944098226572, 40.00000000000002132 ) ) ;
#22066 = CARTESIAN_POINT ( 'NONE',  ( -86.96347745069644475, 12.89780903124349898, 43.67073346367994446 ) ) ;
#22065 = CARTESIAN_POINT ( 'NONE',  ( -121.8281150762304748, 8.694016615518547653, -23.07023398454548868 ) ) ;
#22067 = CARTESIAN_POINT ( 'NONE',  ( 98.29850319125813485, -18.22532005591201809, -8.262390927758364256 ) ) ;
#22068 = CARTESIAN_POINT ( 'NONE',  ( 136.1360204305621266, 35.03383547441298873, 0.000000000000000000 ) ) ;
#22069 = CARTESIAN_POINT ( 'NONE',  ( -259.2033419157646676, 30.48217210827734647, 40.00000000000002132 ) ) ;
#22070 = CARTESIAN_POINT ( 'NONE',  ( 19.06497207195981858, 5.735870351258996432E-13, -54.19242893257843008 ) ) ;
#22071 = CARTESIAN_POINT ( 'NONE',  ( 4.995406935893290878, 1.606505379428369110E-13, -15.24977328854832592 ) ) ;
#22072 = PRODUCT_DEFINITION_SHAPE ( 'NONE', 'NONE',  #11592 ) ;
#22073 = CARTESIAN_POINT ( 'NONE',  ( 57.59792236341147031, 30.00663442387720181, -26.56190807104661289 ) ) ;
#22074 = ORIENTED_EDGE ( 'NONE', *, *, #24254, .T. ) ;
#22075 = CARTESIAN_POINT ( 'NONE',  ( -77.90255099906769942, -20.29001641120661859, 8.064892378658379712 ) ) ;
#22076 = CARTESIAN_POINT ( 'NONE',  ( 192.4448373802100889, 20.00000000003945644, 0.000000000000000000 ) ) ;
#22077 = EDGE_CURVE ( 'NONE', #11822, #18109, #9001, .T. ) ;
#22078 = PRODUCT_CONTEXT ( 'NONE', #2450, 'mechanical' ) ;
#22079 = VERTEX_POINT ( 'NONE', #23146 ) ;
#22080 = ORIENTED_EDGE ( 'NONE', *, *, #19960, .F. ) ;
#22081 = CARTESIAN_POINT ( 'NONE',  ( 146.6084372240433709, -3.800685668858344801, -52.76785682606520567 ) ) ;
#22082 = CARTESIAN_POINT ( 'NONE',  ( 23.48902902575148488, -42.82177761400719618, -23.31625887490651650 ) ) ;
#22083 = ORIENTED_EDGE ( 'NONE', *, *, #18585, .T. ) ;
#22084 = CARTESIAN_POINT ( 'NONE',  ( 130.8568914410475088, -34.05028731879786363, -40.00000000000002132 ) ) ;
#22085 = CARTESIAN_POINT ( 'NONE',  ( -102.4294859497687327, -20.29697089191209969, 8.407280618541118855 ) ) ;
#22086 = AXIS2_PLACEMENT_3D ( 'NONE', #21033, #6521, #24505 ) ;
#22087 = ORIENTED_EDGE ( 'NONE', *, *, #9807, .T. ) ;
#22088 = CARTESIAN_POINT ( 'NONE',  ( 200.0000000000000000, 5.800536564436440834, 18.10358378745109320 ) ) ;
#22089 = DIRECTION ( 'NONE',  ( 0.9352143328345118301, -0.3271292286605502753, 0.1355013631549612796 ) ) ;
#22090 = CARTESIAN_POINT ( 'NONE',  ( -213.1075012329537230, 37.98287015391236565, -18.58567234101138510 ) ) ;
#22091 = CARTESIAN_POINT ( 'NONE',  ( -183.6285492668830557, -41.87133366545522506, -17.34367427884065549 ) ) ;
#22092 = CARTESIAN_POINT ( 'NONE',  ( -259.2033419157646676, -1.564921101325656229E-13, 30.48217210827739621 ) ) ;
#22093 = CARTESIAN_POINT ( 'NONE',  ( -135.8532207217289738, -9.153146818113595984, 0.000000000000000000 ) ) ;
#22094 = CARTESIAN_POINT ( 'NONE',  ( 163.1118516004056573, -19.27778845539181063, -37.29075403953176959 ) ) ;
#22095 = CYLINDRICAL_SURFACE ( 'NONE', #919, 30.00000000000003908 ) ;
#22096 = CARTESIAN_POINT ( 'NONE',  ( 170.2234770963711128, 1.169953928977015745E-13, -24.55285855007187124 ) ) ;
#22097 = AXIS2_PLACEMENT_3D ( 'NONE', #11348, #5624, #21996 ) ;
#22098 = CARTESIAN_POINT ( 'NONE',  ( -91.56559293963834989, -40.00000000000027711, 22.67402823373149801 ) ) ;
#22099 = FACE_BOUND ( 'NONE', #11851, .T. ) ;
#22100 = CARTESIAN_POINT ( 'NONE',  ( -100.7734535825088500, 16.03295912088683295, 40.53558337403684675 ) ) ;
#22101 = CARTESIAN_POINT ( 'NONE',  ( 184.8905102610680444, 20.92133201514447194, -40.00000000000002132 ) ) ;
#22102 = CARTESIAN_POINT ( 'NONE',  ( -208.1127848780264742, -67.17687982763172272, 10.60833733270744617 ) ) ;
#22103 = PLANE ( 'NONE',  #9220 ) ;
#22104 = AXIS2_PLACEMENT_3D ( 'NONE', #15452, #1893, #13983 ) ;
#22105 = DIRECTION ( 'NONE',  ( 1.836970198721030181E-16, -1.000000000000000000, 0.000000000000000000 ) ) ;
#22106 = CARTESIAN_POINT ( 'NONE',  ( -259.2033419157646676, -40.00000000000003553, -9.517827891722768996 ) ) ;
#22107 = CARTESIAN_POINT ( 'NONE',  ( -198.0356074513804572, 39.15871834505912119, -17.40982414986464377 ) ) ;
#22108 = CARTESIAN_POINT ( 'NONE',  ( -135.8532207217289738, 6.472252184284096543, 6.472252184284234211 ) ) ;
#22109 = CARTESIAN_POINT ( 'NONE',  ( -188.3066136396867307, -13.82848859481001647, -46.99300418776059729 ) ) ;
#22110 = CARTESIAN_POINT ( 'NONE',  ( -86.96347745069644475, 15.38646221621793586, -15.38646221621778842 ) ) ;
#22111 = ORIENTED_EDGE ( 'NONE', *, *, #2485, .T. ) ;
#22112 = CARTESIAN_POINT ( 'NONE',  ( -280.0000000000000000, -14.14213562373118549, 14.14213562373078936 ) ) ;
#22113 = CYLINDRICAL_SURFACE ( 'NONE', #10191, 44.99999999999997158 ) ;
#22114 = CARTESIAN_POINT ( 'NONE',  ( 192.4448373802100889, 14.14213562375893574, -14.14213562375874922 ) ) ;
#22115 = CARTESIAN_POINT ( 'NONE',  ( -100.7734535825088500, 22.67402823373189591, -0.000000000000000000 ) ) ;
#22116 = CARTESIAN_POINT ( 'NONE',  ( 190.0000000000000000, -71.50000000000002842, 66.50000000000005684 ) ) ;
#22117 = CARTESIAN_POINT ( 'NONE',  ( 91.82158438592158234, -12.16597498399995203, -44.40256751092347542 ) ) ;
#22118 = DIRECTION ( 'NONE',  ( 0.000000000000000000, 0.000000000000000000, 1.000000000000000000 ) ) ;
#22119 = VERTEX_POINT ( 'NONE', #2923 ) ;
#22120 = CARTESIAN_POINT ( 'NONE',  ( 199.9999999999999432, 18.36080785346942434, 4.936233792941779441 ) ) ;
#22121 = CARTESIAN_POINT ( 'NONE',  ( -200.0000000000000000, 82.50000000000008527, 52.49999999999979394 ) ) ;
#22122 = CARTESIAN_POINT ( 'NONE',  ( -6.342283169555448907, 23.00001740814278506, 42.32555349774906972 ) ) ;
#22123 = ORIENTED_EDGE ( 'NONE', *, *, #5254, .T. ) ;
#22124 = ORIENTED_EDGE ( 'NONE', *, *, #2841, .F. ) ;
#22125 = CARTESIAN_POINT ( 'NONE',  ( -213.1075012329537230, 9.698598906450410340, 9.698598906450483170 ) ) ;
#22126 = CARTESIAN_POINT ( 'NONE',  ( 199.0056860580130262, 9.997888132351027579, -17.31887563448481160 ) ) ;
#22127 = CARTESIAN_POINT ( 'NONE',  ( -86.96347745069644475, -15.38646221621786125, -15.38646221621789856 ) ) ;
#22128 = AXIS2_PLACEMENT_3D ( 'NONE', #22850, #14323, #16979 ) ;
#22129 = PLANE ( 'NONE',  #11825 ) ;
#22130 = CARTESIAN_POINT ( 'NONE',  ( 85.88436428469954365, 10.32541753206531432, -22.72801546669109385 ) ) ;
#22131 = CARTESIAN_POINT ( 'NONE',  ( 200.0000000000001421, -15.08701489606589341, 11.56722645162647467 ) ) ;
#22132 = CARTESIAN_POINT ( 'NONE',  ( -645.2837021124099692, 32.14196927292066874, -23.84742176288152748 ) ) ;
#22133 = CARTESIAN_POINT ( 'NONE',  ( -4.039451493210490796, -23.44932283416679297, 43.00522595894000943 ) ) ;
#22134 = CARTESIAN_POINT ( 'NONE',  ( 199.0231121918538975, 0.6363371645724309467, 19.99606429142543362 ) ) ;
#22135 = CARTESIAN_POINT ( 'NONE',  ( -166.3490444791740401, 19.13701437391346616, 36.43931842066525917 ) ) ;
#22136 = CARTESIAN_POINT ( 'NONE',  ( -4.082462733454488735, -13.82507958736516684, -46.97557262069201300 ) ) ;
#22137 = CARTESIAN_POINT ( 'NONE',  ( 170.2234770963711128, -39.20704971665404059, 17.36149277826957160 ) ) ;
#22138 = CARTESIAN_POINT ( 'NONE',  ( 98.29820294267862835, 15.90088694521858415, -12.38338430224807851 ) ) ;
#22139 = CARTESIAN_POINT ( 'NONE',  ( -192.9588430854689705, -38.51493924976963967, 38.51493924976919914 ) ) ;
#22140 = CARTESIAN_POINT ( 'NONE',  ( 151.7948205124836250, -3.202120068677277203E-13, 33.23291073765553705 ) ) ;
#22141 = CARTESIAN_POINT ( 'NONE',  ( 151.7948205124836250, 33.23291073765556547, 0.000000000000000000 ) ) ;
#22142 = CARTESIAN_POINT ( 'NONE',  ( -135.8532207217289738, -30.84685318188647685, -2.449293598294708485E-15 ) ) ;
#22143 = DIRECTION ( 'NONE',  ( -1.000000000000000000, -1.836970198721030181E-16, 0.000000000000000000 ) ) ;
#22144 = AXIS2_PLACEMENT_3D ( 'NONE', #19283, #1066, #9884 ) ;
#22145 = CARTESIAN_POINT ( 'NONE',  ( -100.7734535825088500, -17.32597176626813251, 40.00000000000002132 ) ) ;
#22146 = AXIS2_PLACEMENT_3D ( 'NONE', #18066, #7813, #15929 ) ;
#22147 = CARTESIAN_POINT ( 'NONE',  ( -97.72675010090206627, 20.89622088363370622, -8.185591577777238115 ) ) ;
#22148 = CARTESIAN_POINT ( 'NONE',  ( -91.56559293963836410, 40.00000000000019185, -17.32597176626768487 ) ) ;
#22149 = CARTESIAN_POINT ( 'NONE',  ( 4.995406935893289102, 10.78321810388998081, 10.78321810389001811 ) ) ;
#22150 = CARTESIAN_POINT ( 'NONE',  ( -162.0762913951021176, 1.694272876828294194, -40.00000000000002132 ) ) ;
#22151 = ORIENTED_EDGE ( 'NONE', *, *, #4782, .F. ) ;
#22152 = CARTESIAN_POINT ( 'NONE',  ( -100.7734535825088500, -22.67402823373193499, 40.00000000000002132 ) ) ;
#22153 = CIRCLE ( 'NONE', #20016, 5.000000000000004441 ) ;
#22154 = CARTESIAN_POINT ( 'NONE',  ( 118.9130007099547299, 10.68958087202317131, 25.80693111732301048 ) ) ;
#22155 = EDGE_CURVE ( 'NONE', #12135, #11462, #10043, .T. ) ;
#22156 = CARTESIAN_POINT ( 'NONE',  ( -198.0356074513804572, 67.44298959253333692, 10.87444709760969452 ) ) ;
#22157 = CARTESIAN_POINT ( 'NONE',  ( -105.3755690713226585, -40.00000000000010658, 18.24025645688337249 ) ) ;
#22158 = CIRCLE ( 'NONE', #24711, 40.00000000000003553 ) ;
#22159 = ADVANCED_FACE ( 'NONE', ( #18614 ), #8755, .T. ) ;
#22160 = CARTESIAN_POINT ( 'NONE',  ( -30.26275506840324070, 1.694272468446254232, 0.000000000000000000 ) ) ;
#22161 = CIRCLE ( 'NONE', #3789, 31.79780246617542616 ) ;
#22162 = CARTESIAN_POINT ( 'NONE',  ( 190.0000000000000000, -66.50000000000001421, -66.50000000000005684 ) ) ;
#22163 = DIRECTION ( 'NONE',  ( 0.000000000000000000, 1.000000000000000000, 0.000000000000000000 ) ) ;
#22164 = CARTESIAN_POINT ( 'NONE',  ( 200.0000000000002558, 17.05253901346626222, -8.385556056821480198 ) ) ;
#22165 = ADVANCED_FACE ( 'NONE', ( #24580, #18584 ), #20723, .F. ) ;
#22166 = EDGE_CURVE ( 'NONE', #11718, #14180, #26330, .T. ) ;
#22167 = CARTESIAN_POINT ( 'NONE',  ( 199.9999999999999432, -18.76513715205313559, -3.093437544788904869 ) ) ;
#22168 = B_SPLINE_CURVE_WITH_KNOTS ( 'NONE', 3,
 ( #24583, #14461, #20586, #17558, #22592, #14854 ),
 .UNSPECIFIED., .F., .F.,
 ( 4, 2, 4 ),
 ( -5.998621906156382924E-08, 0.03938016914544737596, 0.07876039827711382724 ),
 .UNSPECIFIED. ) ;
#22169 = CARTESIAN_POINT ( 'NONE',  ( 91.82158438592158234, 16.11829626346161604, -16.11829626346121103 ) ) ;
#22170 = CARTESIAN_POINT ( 'NONE',  ( 136.1360204305621551, -31.79587985999279454, 24.77266263493094911 ) ) ;
#22171 = CARTESIAN_POINT ( 'NONE',  ( -105.4894168351564048, 19.67999904371083275, 8.151722511394638104 ) ) ;
#22172 = CARTESIAN_POINT ( 'NONE',  ( -259.2033419157646676, -1.473088368616265084E-13, 9.517827891722632216 ) ) ;
#22173 = CARTESIAN_POINT ( 'NONE',  ( -259.2033419157646676, -21.55415060305872998, 35.01439189186525880 ) ) ;
#22174 = CARTESIAN_POINT ( 'NONE',  ( 151.7948205124836250, -23.49921654116371883, 23.49921654116317526 ) ) ;
#22175 = CARTESIAN_POINT ( 'NONE',  ( 184.8905102610680444, -43.07788698682556827, -13.49065550809859104 ) ) ;
#22176 = CARTESIAN_POINT ( 'NONE',  ( -198.0356074513804572, -39.15871834505905724, -17.40982414986491733 ) ) ;
#22177 = CARTESIAN_POINT ( 'NONE',  ( 199.0232603141898551, 0.2386269578223878252, 20.00239709541226674 ) ) ;
#22179 = CARTESIAN_POINT ( 'NONE',  ( -162.0762913951021176, -40.00000000000019895, 41.69427287672974813 ) ) ;
#22178 = CARTESIAN_POINT ( 'NONE',  ( -259.2033419157646676, 21.55415060305860209, -21.55415060305812602 ) ) ;
#22180 = CARTESIAN_POINT ( 'NONE',  ( -238.4067589809705794, 0.6820004457912851592, -0.6820004457913123597 ) ) ;
#22181 = VECTOR ( 'NONE', #13816, 1000.000000000000000 ) ;
#22182 = CARTESIAN_POINT ( 'NONE',  ( 8.209392600929815487, 44.89226883836261806, -24.84362085272430676 ) ) ;
#22183 = CARTESIAN_POINT ( 'NONE',  ( 4.995406935893288214, 55.24977328854835434, 2.449293598294708485E-15 ) ) ;
#22184 = ORIENTED_EDGE ( 'NONE', *, *, #10112, .F. ) ;
#22185 = CARTESIAN_POINT ( 'NONE',  ( -678.9461782662772293, 75.00000000000000000, 30.00000000000158096 ) ) ;
#22186 = CARTESIAN_POINT ( 'NONE',  ( 51.52267038239544661, 34.28362880217498798, 14.20074401722577839 ) ) ;
#22187 = DIRECTION ( 'NONE',  ( 1.000000000000000000, 1.836970198721030181E-16, 0.000000000000000000 ) ) ;
#22188 = CARTESIAN_POINT ( 'NONE',  ( 151.7948205124836250, -33.23291073765550863, 0.000000000000000000 ) ) ;
#22189 = ORIENTED_EDGE ( 'NONE', *, *, #21185, .T. ) ;
#22190 = CARTESIAN_POINT ( 'NONE',  ( -189.1288337602858860, -43.24060467048573031, 23.62383291543415709 ) ) ;
#22191 = CARTESIAN_POINT ( 'NONE',  ( 199.9999999999999432, -13.66164182518334691, 13.22314710892283074 ) ) ;
#22192 = CARTESIAN_POINT ( 'NONE',  ( 11.59303701482094517, -18.58252782966835781, 44.86219070952759580 ) ) ;
#22193 = CARTESIAN_POINT ( 'NONE',  ( 23.54890483848243221, 23.30407993985267012, -42.80335737019193942 ) ) ;
#22194 = CARTESIAN_POINT ( 'NONE',  ( 199.0108247880216368, -5.504876786518239307, -19.22761790364454271 ) ) ;
#22195 = CIRCLE ( 'NONE', #17500, 5.000000000000004441 ) ;
#22196 = CARTESIAN_POINT ( 'NONE',  ( 137.0939645874030930, -30.33050608226204758, 12.56330697291239140 ) ) ;
#22197 = CARTESIAN_POINT ( 'NONE',  ( -200.0000000000000000, 60.00000000000009948, 0.000000000000000000 ) ) ;
#22198 =( BOUNDED_SURFACE ( )  B_SPLINE_SURFACE ( 3, 3, ( 
 ( #21881, #8036, #24004, #9508, #3658, #5647, #7763, #5784, #3525, #26296, #19884, #5921, #1667, #3796, #5520, #17613, #25886, #7629, #18147, #13753, #24287, #19622, #18012, #13891, #1407, #22025, #25757, #11899, #9775, #26026 ),
 ( #26159, #16155, #22292, #7505, #6056, #15742, #20023, #1803, #7901, #9642, #17745, #1935, #14160, #1537, #15615, #9906, #20153, #3938, #17876, #16020, #24145, #23739, #23872, #13625, #14029, #12034, #10040, #21751, #11626, #19747 ),
 ( #2202, #8174, #12428, #18416, #6181, #22821, #20290, #10311, #4069, #332, #14294, #4204, #14426, #191, #22557, #469, #16289, #24683, #8573, #8301, #2069, #16686, #10436, #24817, #24553, #18280, #12171, #12296, #14557, #4336 ),
 ( #16426, #66, #22429, #6570, #14690, #24416, #18552, #6308, #20556, #10176, #20423, #2325, #8437, #16555, #6441, #22688, #4463, #2458, #12557, #20690, #10570, #18684, #4598, #12696, #19977, #22251, #1758, #20116, #21843, #25849 ),
 ( #8132, #21980, #14249, #1495, #7993, #5878, #17706, #13984, #7593, #1894, #17969, #15976, #3613, #5612, #15705, #14123, #4027, #16249, #24104, #24377, #22117, #9601, #12125, #2031, #20250, #3894, #6141, #16112, #10133, #7724 ),
 ( #9867, #26257, #24242, #23829, #13846, #13718, #6014, #18236, #7855, #11724, #21, #25984, #26116, #19843, #22389, #4166, #1628, #9735, #12259, #17837, #9999, #15835, #23965, #3751, #11994, #18107, #5740, #11857, #20780, #4686 ),
 ( #16774, #156, #23047, #8529, #20643, #24776, #560, #8665, #10667, #2159, #4558, #24512, #4822, #8798, #16377, #20383, #12514, #14778, #2418, #12654, #14386, #18377, #8393, #16515, #689, #14514, #6796, #10267, #24907, #6529 ) ),
 .UNSPECIFIED., .T., .F., .F. ) 
 B_SPLINE_SURFACE_WITH_KNOTS ( ( 4, 3, 4 ),
 ( 4, 2, 2, 2, 2, 2, 2, 2, 2, 2, 2, 2, 2, 2, 4 ),
 ( 0.000000000000000000, 0.5000000000000000000, 1.000000000000000000 ),
 ( 0.000000000000000000, 0.1357259735107005372, 0.1651108541090157700, 0.1944957347073310028, 0.3598804999793158710, 0.3867117631979620773, 0.4135430264166082281, 0.5789277916885930964, 0.6062785021374117456, 0.6336292125862302838, 0.8508620842112317728, 0.8814014469398914198, 0.9119408096685510667, 0.9559704048342755334, 1.000000000000000000 ),
 .UNSPECIFIED. ) 
 GEOMETRIC_REPRESENTATION_ITEM ( )  RATIONAL_B_SPLINE_SURFACE ( (
 ( 1.000000000000000000, 1.000000000000000000, 1.000000000000000000, 1.000000000000000000, 1.000000000000000000, 1.000000000000000000, 1.000000000000000000, 1.000000000000000000, 1.000000000000000000, 1.000000000000000000, 1.000000000000000000, 1.000000000000000000, 1.000000000000000000, 1.000000000000000000, 1.000000000000000000, 1.000000000000000000, 1.000000000000000000, 1.000000000000000000, 1.000000000000000000, 1.000000000000000000, 1.000000000000000000, 1.000000000000000000, 1.000000000000000000, 1.000000000000000000, 1.000000000000000000, 1.000000000000000000, 1.000000000000000000, 1.000000000000000000, 1.000000000000000000, 1.000000000000000000),
 ( 0.3333333333333333703, 0.3333333333333333703, 0.3333333333333333703, 0.3333333333333333703, 0.3333333333333333703, 0.3333333333333333703, 0.3333333333333333703, 0.3333333333333333703, 0.3333333333333333703, 0.3333333333333333703, 0.3333333333333333703, 0.3333333333333333703, 0.3333333333333333703, 0.3333333333333333703, 0.3333333333333333703, 0.3333333333333333703, 0.3333333333333333703, 0.3333333333333333703, 0.3333333333333333703, 0.3333333333333333703, 0.3333333333333333703, 0.3333333333333333703, 0.3333333333333333703, 0.3333333333333333703, 0.3333333333333333703, 0.3333333333333333703, 0.3333333333333333703, 0.3333333333333333703, 0.3333333333333333703, 0.3333333333333333703),
 ( 0.3333333333333333703, 0.3333333333333333703, 0.3333333333333333703, 0.3333333333333333703, 0.3333333333333333703, 0.3333333333333333703, 0.3333333333333333703, 0.3333333333333333703, 0.3333333333333333703, 0.3333333333333333703, 0.3333333333333333703, 0.3333333333333333703, 0.3333333333333333703, 0.3333333333333333703, 0.3333333333333333703, 0.3333333333333333703, 0.3333333333333333703, 0.3333333333333333703, 0.3333333333333333703, 0.3333333333333333703, 0.3333333333333333703, 0.3333333333333333703, 0.3333333333333333703, 0.3333333333333333703, 0.3333333333333333703, 0.3333333333333333703, 0.3333333333333333703, 0.3333333333333333703, 0.3333333333333333703, 0.3333333333333333703),
 ( 1.000000000000000000, 1.000000000000000000, 1.000000000000000000, 1.000000000000000000, 1.000000000000000000, 1.000000000000000000, 1.000000000000000000, 1.000000000000000000, 1.000000000000000000, 1.000000000000000000, 1.000000000000000000, 1.000000000000000000, 1.000000000000000000, 1.000000000000000000, 1.000000000000000000, 1.000000000000000000, 1.000000000000000000, 1.000000000000000000, 1.000000000000000000, 1.000000000000000000, 1.000000000000000000, 1.000000000000000000, 1.000000000000000000, 1.000000000000000000, 1.000000000000000000, 1.000000000000000000, 1.000000000000000000, 1.000000000000000000, 1.000000000000000000, 1.000000000000000000),
 ( 0.3333333333333333703, 0.3333333333333333703, 0.3333333333333333703, 0.3333333333333333703, 0.3333333333333333703, 0.3333333333333333703, 0.3333333333333333703, 0.3333333333333333703, 0.3333333333333333703, 0.3333333333333333703, 0.3333333333333333703, 0.3333333333333333703, 0.3333333333333333703, 0.3333333333333333703, 0.3333333333333333703, 0.3333333333333333703, 0.3333333333333333703, 0.3333333333333333703, 0.3333333333333333703, 0.3333333333333333703, 0.3333333333333333703, 0.3333333333333333703, 0.3333333333333333703, 0.3333333333333333703, 0.3333333333333333703, 0.3333333333333333703, 0.3333333333333333703, 0.3333333333333333703, 0.3333333333333333703, 0.3333333333333333703),
 ( 0.3333333333333333703, 0.3333333333333333703, 0.3333333333333333703, 0.3333333333333333703, 0.3333333333333333703, 0.3333333333333333703, 0.3333333333333333703, 0.3333333333333333703, 0.3333333333333333703, 0.3333333333333333703, 0.3333333333333333703, 0.3333333333333333703, 0.3333333333333333703, 0.3333333333333333703, 0.3333333333333333703, 0.3333333333333333703, 0.3333333333333333703, 0.3333333333333333703, 0.3333333333333333703, 0.3333333333333333703, 0.3333333333333333703, 0.3333333333333333703, 0.3333333333333333703, 0.3333333333333333703, 0.3333333333333333703, 0.3333333333333333703, 0.3333333333333333703, 0.3333333333333333703, 0.3333333333333333703, 0.3333333333333333703),
 ( 1.000000000000000000, 1.000000000000000000, 1.000000000000000000, 1.000000000000000000, 1.000000000000000000, 1.000000000000000000, 1.000000000000000000, 1.000000000000000000, 1.000000000000000000, 1.000000000000000000, 1.000000000000000000, 1.000000000000000000, 1.000000000000000000, 1.000000000000000000, 1.000000000000000000, 1.000000000000000000, 1.000000000000000000, 1.000000000000000000, 1.000000000000000000, 1.000000000000000000, 1.000000000000000000, 1.000000000000000000, 1.000000000000000000, 1.000000000000000000, 1.000000000000000000, 1.000000000000000000, 1.000000000000000000, 1.000000000000000000, 1.000000000000000000, 1.000000000000000000) ) ) 
 REPRESENTATION_ITEM ( '' )  SURFACE ( )  );
#22199 = CARTESIAN_POINT ( 'NONE',  ( -280.0000000000000000, 14.14213562373108246, -14.14213562373078581 ) ) ;
#22200 = CARTESIAN_POINT ( 'NONE',  ( -280.0000000000000000, 19.99999999999996092, -0.000000000000000000 ) ) ;
#22202 = CARTESIAN_POINT ( 'NONE',  ( 170.0000000000000853, -9.369682556672300322, 22.62041470344878746 ) ) ;
#22201 = CARTESIAN_POINT ( 'NONE',  ( -188.2871287166302636, 13.82723289751406703, -46.98614659774629843 ) ) ;
#22203 = CARTESIAN_POINT ( 'NONE',  ( 98.29820294267378245, -17.32045324915796769, -10.02182676112147774 ) ) ;
#22204 = CARTESIAN_POINT ( 'NONE',  ( 19.06497207195981503, -14.19242893257840166, 0.000000000000000000 ) ) ;
#22205 = CARTESIAN_POINT ( 'NONE',  ( 0.2972598230769930572, 14.33493731733933352, 0.000000000000000000 ) ) ;
#22206 = CARTESIAN_POINT ( 'NONE',  ( -259.2033419157646676, -39.99999999999975131, -30.48217210827782608 ) ) ;
#22207 = CARTESIAN_POINT ( 'NONE',  ( -162.0762913951020892, 57.76657433537918251, 1.198031840455469066 ) ) ;
#22208 = CARTESIAN_POINT ( 'NONE',  ( 180.0000000000000000, -35.78896085774753288, 1.496915739050593134E-14 ) ) ;
#22209 = CARTESIAN_POINT ( 'NONE',  ( 170.2234770963711128, 17.36149277826980253, 17.36149277827007253 ) ) ;
#22210 = ORIENTED_EDGE ( 'NONE', *, *, #17029, .T. ) ;
#22211 = CARTESIAN_POINT ( 'NONE',  ( 91.82158438592158234, -40.45024623143958564, 16.11829626348418998 ) ) ;
#22212 = CARTESIAN_POINT ( 'NONE',  ( -86.86493150571116928, -7.943527260496078490, 19.77569912839177135 ) ) ;
#22213 = ORIENTED_EDGE ( 'NONE', *, *, #21911, .T. ) ;
#22214 = EDGE_LOOP ( 'NONE', ( #10935, #15176, #528, #23925 ) ) ;
#22215 = CARTESIAN_POINT ( 'NONE',  ( 184.8905102610680444, -13.49065550809780412, -43.07788698682583828 ) ) ;
#22216 = CARTESIAN_POINT ( 'NONE',  ( 22.33254948916634319, -43.29223140031879780, -17.93222939140903449 ) ) ;
#22217 = ORIENTED_EDGE ( 'NONE', *, *, #17141, .F. ) ;
#22218 = CARTESIAN_POINT ( 'NONE',  ( 170.2234770963711128, -24.55285855007184281, -40.00000000000002132 ) ) ;
#22219 = PLANE ( 'NONE',  #17670 ) ;
#22220 = ORIENTED_EDGE ( 'NONE', *, *, #23866, .F. ) ;
#22221 = CARTESIAN_POINT ( 'NONE',  ( 199.9999999999996874, 13.64679526057751069, 13.22824625860694070 ) ) ;
#22222 = DIRECTION ( 'NONE',  ( 0.000000000000000000, 1.000000000000000000, 0.000000000000000000 ) ) ;
#22223 = CARTESIAN_POINT ( 'NONE',  ( 200.0000000000000000, 42.42640687119288856, -14.14213562373094746 ) ) ;
#22224 = CARTESIAN_POINT ( 'NONE',  ( -188.4265466358226035, -43.04237830659937458, -23.47687925214709637 ) ) ;
#22225 = CARTESIAN_POINT ( 'NONE',  ( -56.48582580120558561, -40.00000000000000000, -9.153146818113723882 ) ) ;
#22226 = CARTESIAN_POINT ( 'NONE',  ( 130.8568914410475372, -34.05028731879786363, 0.000000000000000000 ) ) ;
#22227 = CARTESIAN_POINT ( 'NONE',  ( -105.3755690713226585, -15.38646221621738164, -41.18208027870615240 ) ) ;
#22228 = CARTESIAN_POINT ( 'NONE',  ( 199.0250816517838359, -5.508431349499541163, 19.23181920140171997 ) ) ;
#22229 = CARTESIAN_POINT ( 'NONE',  ( 91.82158438592159655, -39.99999999999994316, -17.20528682183314118 ) ) ;
#22230 = CARTESIAN_POINT ( 'NONE',  ( -238.4067589809705794, -40.00000000000021316, 40.96449427990166470 ) ) ;
#22231 = CARTESIAN_POINT ( 'NONE',  ( -56.48582580120559271, -1.062504017861011783E-13, 9.153146818113587102 ) ) ;
#22232 = CARTESIAN_POINT ( 'NONE',  ( 146.6084372240433709, 40.00000000000017053, -34.62501878078291639 ) ) ;
#22233 = EDGE_CURVE ( 'NONE', #6105, #10135, #11852, .T. ) ;
#22234 = CARTESIAN_POINT ( 'NONE',  ( 199.9999999999999432, 20.00000000000013856, 0.000000000000000000 ) ) ;
#22235 = CARTESIAN_POINT ( 'NONE',  ( -100.7734535825088500, -40.53558337403669753, -16.03295912088728770 ) ) ;
#22236 = CARTESIAN_POINT ( 'NONE',  ( -100.7734535825088500, 22.67402823373189591, -0.000000000000000000 ) ) ;
#22237 = CARTESIAN_POINT ( 'NONE',  ( -100.7734535825088500, -12.25131212657462498, -44.31723036834905827 ) ) ;
#22238 = LINE ( 'NONE', #20103, #19818 ) ;
#22239 = CYLINDRICAL_SURFACE ( 'NONE', #10680, 34.99999999999999289 ) ;
#22240 = CARTESIAN_POINT ( 'NONE',  ( 151.7948205124836250, 23.49921654116328540, 23.49921654116366554 ) ) ;
#22241 = CARTESIAN_POINT ( 'NONE',  ( -208.1127848780265026, -2.327190355601776466E-13, 55.00245453012672670 ) ) ;
#22242 = CARTESIAN_POINT ( 'NONE',  ( 199.9999999999999432, 14.14213562373090838, 14.14213562373092437 ) ) ;
#22243 = CARTESIAN_POINT ( 'NONE',  ( -213.1075012329537230, -9.698598906450422774, -9.698598906450550672 ) ) ;
#22244 = CARTESIAN_POINT ( 'NONE',  ( -190.7346372395361129, -13.94676542151222343, -47.78727444209329889 ) ) ;
#22245 = CARTESIAN_POINT ( 'NONE',  ( -280.0000000000000568, -14.14213562373078226, -42.42640687119295251 ) ) ;
#22246 = ORIENTED_EDGE ( 'NONE', *, *, #17665, .F. ) ;
#22247 = CARTESIAN_POINT ( 'NONE',  ( -56.48582580120559982, -34.75652343174584047, -21.81201906317815187 ) ) ;
#22248 = LINE ( 'NONE', #22386, #2971 ) ;
#22249 = CARTESIAN_POINT ( 'NONE',  ( 14.38125909742181285, -15.17850393972633505, 0.000000000000000000 ) ) ;
#22250 = CARTESIAN_POINT ( 'NONE',  ( -86.84962968273566730, 19.67999904273991163, 8.151722510992470916 ) ) ;
#22251 = CARTESIAN_POINT ( 'NONE',  ( 163.1118516004056573, 9.006482792069759213, -9.006482792069505194 ) ) ;
#22252 = DIRECTION ( 'NONE',  ( 0.000000000000000000, 1.000000000000000000, 0.000000000000000000 ) ) ;
#22253 = EDGE_LOOP ( 'NONE', ( #22974, #2688, #15204, #16741, #16975, #10939 ) ) ;
#22254 = CARTESIAN_POINT ( 'NONE',  ( 199.9999999999999716, 16.13598342540508668, 10.05825190933999203 ) ) ;
#22255 = CARTESIAN_POINT ( 'NONE',  ( 23.23639021239535651, -23.37084785298091916, 42.89921396172186974 ) ) ;
#22256 = EDGE_CURVE ( 'NONE', #20847, #8430, #6994, .T. ) ;
#22257 = CARTESIAN_POINT ( 'NONE',  ( -4.082462733456166504, 23.44093842354227419, 42.99255347688187356 ) ) ;
#22258 = ORIENTED_EDGE ( 'NONE', *, *, #2836, .T. ) ;
#22259 = ORIENTED_EDGE ( 'NONE', *, *, #26072, .F. ) ;
#22260 = CARTESIAN_POINT ( 'NONE',  ( -100.7734535825088358, -16.03295912088706743, -16.03295912088710296 ) ) ;
#22261 = CARTESIAN_POINT ( 'NONE',  ( 199.0082207658673781, 0.6402583678929150146, -19.98857080023024579 ) ) ;
#22262 = CARTESIAN_POINT ( 'NONE',  ( -114.4364955367327212, -8.064892380842954012, -20.29001642038816300 ) ) ;
#22263 = ADVANCED_FACE ( 'NONE', ( #1274 ), #25630, .F. ) ;
#22264 =( LENGTH_UNIT ( ) NAMED_UNIT ( * ) SI_UNIT ( .MILLI., .METRE. ) );
#22265 = CARTESIAN_POINT ( 'NONE',  ( 17.75917276260960875, 44.20478326162373151, -24.33671690504812801 ) ) ;
#22266 = ADVANCED_FACE ( 'NONE', ( #7128 ), #6730, .T. ) ;
#22267 = CARTESIAN_POINT ( 'NONE',  ( -100.7734535825088500, 39.99999999999976552, 22.67402823373233645 ) ) ;
#22268 = CARTESIAN_POINT ( 'NONE',  ( 199.9999999999998579, -17.68075590865577951, 6.990562776172230208 ) ) ;
#22269 = CARTESIAN_POINT ( 'NONE',  ( -77.70091844760044353, -21.35079699648278861, -5.501606197251263985 ) ) ;
#22270 = CARTESIAN_POINT ( 'NONE',  ( 200.0000000000000000, 66.50000000000009948, 66.50000000000005684 ) ) ;
#22271 = B_SPLINE_CURVE_WITH_KNOTS ( 'NONE', 3,
 ( #13904, #16167, #22038, #17889, #22569, #3810 ),
 .UNSPECIFIED., .F., .F.,
 ( 4, 2, 4 ),
 ( 0.000000000000000000, 0.03937634048170812057, 0.07875268096341624113 ),
 .UNSPECIFIED. ) ;
#22272 = CARTESIAN_POINT ( 'NONE',  ( 199.0189287881835583, 9.564175521352543896, 17.56735958655279362 ) ) ;
#22273 = CARTESIAN_POINT ( 'NONE',  ( -114.4364955367302912, 8.644468109216418839, 20.04994829327247530 ) ) ;
#22274 = CARTESIAN_POINT ( 'NONE',  ( -4.004886986944679705, -13.82996668233299431, -47.00296421444959805 ) ) ;
#22275 = CARTESIAN_POINT ( 'NONE',  ( -198.0356074513804288, -39.15871834505882276, -39.15871834505946936 ) ) ;
#22276 = CARTESIAN_POINT ( 'NONE',  ( -100.0753760173601279, 20.41987330121804334, -8.894334231739408736 ) ) ;
#22277 = CARTESIAN_POINT ( 'NONE',  ( -259.2033419157646676, -49.83842185052031937, -6.730120644403796426 ) ) ;
#22278 = CARTESIAN_POINT ( 'NONE',  ( 130.8568914410475088, -40.00000000000036238, 34.05028731879746573 ) ) ;
#22279 = CARTESIAN_POINT ( 'NONE',  ( -162.0762913951021176, 27.08623940707639477, -29.48230308784743059 ) ) ;
#22280 = CARTESIAN_POINT ( 'NONE',  ( 200.0000000000000000, -19.99999999999989342, 40.00000000000002132 ) ) ;
#22281 = LINE ( 'NONE', #1921, #15954 ) ;
#22282 = CARTESIAN_POINT ( 'NONE',  ( 146.6084372240433993, -5.374981219216945938, -2.449293598294708485E-15 ) ) ;
#22283 = CARTESIAN_POINT ( 'NONE',  ( -110.0830815298113095, 11.16636597695389987, 16.82107498772007759 ) ) ;
#22284 = CARTESIAN_POINT ( 'NONE',  ( -91.56559293963836410, 39.99999999999976552, 22.67402823373234000 ) ) ;
#22285 = CARTESIAN_POINT ( 'NONE',  ( 146.6084372240433993, -24.48358557860319706, -24.48358557860330720 ) ) ;
#22286 = CARTESIAN_POINT ( 'NONE',  ( 91.82158438592158234, -17.20528682183298486, 0.000000000000000000 ) ) ;
#22287 = VERTEX_POINT ( 'NONE', #23435 ) ;
#22288 = ORIENTED_EDGE ( 'NONE', *, *, #10112, .T. ) ;
#22289 = CARTESIAN_POINT ( 'NONE',  ( -56.48582580120559982, -9.153146818113595984, 40.00000000000002132 ) ) ;
#22290 = CARTESIAN_POINT ( 'NONE',  ( 146.5090579137182090, 12.40347562390415348, 29.94463907179425988 ) ) ;
#22291 = CARTESIAN_POINT ( 'NONE',  ( -91.56559293963834989, -40.00000000000009948, 17.32597176626796553 ) ) ;
#22292 = CARTESIAN_POINT ( 'NONE',  ( -238.4067589809705794, 28.96627169325285678, 27.60227080167094726 ) ) ;
#22293 = CARTESIAN_POINT ( 'NONE',  ( 146.6084372240433993, -34.62501878078303008, 0.000000000000000000 ) ) ;
#22294 = CARTESIAN_POINT ( 'NONE',  ( -196.0240701155048271, -44.60678452943326988, -24.63338802315930565 ) ) ;
#22295 = PRODUCT_DEFINITION_SHAPE ( 'NONE', 'NONE',  #26365 ) ;
#22296 = CARTESIAN_POINT ( 'NONE',  ( -190.1760961841080757, 13.92889018282242830, -47.67020129349042179 ) ) ;
#22297 = CARTESIAN_POINT ( 'NONE',  ( 200.0000000000001421, 17.31676413174603013, -7.825505819403215213 ) ) ;
#22298 = CARTESIAN_POINT ( 'NONE',  ( 199.9999999999999432, -18.94552238787882104, -1.555198626918513849 ) ) ;
#22299 = CARTESIAN_POINT ( 'NONE',  ( -30.26275506840325136, 57.76657404653985139, -1.198031551615314161 ) ) ;
#22300 = CARTESIAN_POINT ( 'NONE',  ( 130.8568914410475088, -32.49135343045495006, 24.07718906446878648 ) ) ;
#22301 = CARTESIAN_POINT ( 'NONE',  ( -109.1264249741455927, -13.72187187124634278, -33.12752917268957020 ) ) ;
#22302 = CARTESIAN_POINT ( 'NONE',  ( -82.30220482034332008, 18.51665893431357901, -7.992411108784951423 ) ) ;
#22303 = CARTESIAN_POINT ( 'NONE',  ( 170.2234770963711128, -10.92277846919187034, -10.92277846919209594 ) ) ;
#22304 = CARTESIAN_POINT ( 'NONE',  ( -87.02146317964813704, 10.86006974120160962, -18.50839211081806823 ) ) ;
#22305 = CARTESIAN_POINT ( 'NONE',  ( -192.9588430854689989, 10.23066800230742679, 10.23066800230749607 ) ) ;
#22306 = CARTESIAN_POINT ( 'NONE',  ( 19.06497207195981858, -38.31983398719616218, -18.24870850772777331 ) ) ;
#22307 = CARTESIAN_POINT ( 'NONE',  ( 199.0252590766962726, -6.209579518222142269, 19.01904426816868110 ) ) ;
#22308 = ADVANCED_FACE ( 'NONE', ( #21561 ), #9444, .T. ) ;
#22310 = CARTESIAN_POINT ( 'NONE',  ( -135.8532207217289738, 39.99999999999989342, 30.84685318188660474 ) ) ;
#22309 = CARTESIAN_POINT ( 'NONE',  ( 146.6084372240433709, 32.08495691632030145, 24.48358557860365181 ) ) ;
#22311 =( BOUNDED_SURFACE ( )  B_SPLINE_SURFACE ( 3, 2, ( 
 ( #18606, #22736, #12346 ),
 ( #20475, #16479, #10226 ),
 ( #8761, #385, #12218 ),
 ( #8492, #20340, #24605 ),
 ( #18335, #24340, #22477 ),
 ( #18468, #114, #20605 ),
 ( #16339, #6625, #8358 ),
 ( #8221, #2657, #24471 ),
 ( #6359, #6234, #20745 ),
 ( #4387, #14349, #4650 ),
 ( #14478, #12479, #16738 ),
 ( #10493, #12617, #654 ) ),
 .UNSPECIFIED., .F., .F., .F. ) 
 B_SPLINE_SURFACE_WITH_KNOTS ( ( 4, 2, 2, 2, 2, 4 ),
 ( 3, 3 ),
 ( 0.006022589392325605230, 0.01254516766564424401, 0.01580645680230356384, 0.01906774593896288367, 0.02559032421228152332, 0.03211290248560016297 ),
 ( 0.000000000000000000, 1.000000000000000000 ),
 .UNSPECIFIED. ) 
 GEOMETRIC_REPRESENTATION_ITEM ( )  RATIONAL_B_SPLINE_SURFACE ( (
 ( 1.000000000000000000, 0.9998834880171258988, 1.000000000000000000),
 ( 1.000000000000000000, 0.9998139205012247510, 1.000000000000000000),
 ( 1.000000000000000000, 0.9997315632444677691, 1.000000000000000000),
 ( 1.000000000000000000, 0.9996405464946958030, 1.000000000000000000),
 ( 1.000000000000000000, 0.9996155081776924023, 1.000000000000000000),
 ( 1.000000000000000000, 0.9995814087511104562, 1.000000000000000000),
 ( 1.000000000000000000, 0.9995724100939918921, 1.000000000000000000),
 ( 1.000000000000000000, 0.9995726760936894939, 1.000000000000000000),
 ( 1.000000000000000000, 0.9996103361817947341, 1.000000000000000000),
 ( 1.000000000000000000, 0.9997312749795597142, 1.000000000000000000),
 ( 1.000000000000000000, 0.9998135910915183500, 1.000000000000000000),
 ( 1.000000000000000000, 0.9998834880173385065, 1.000000000000000000) ) ) 
 REPRESENTATION_ITEM ( '' )  SURFACE ( )  );
#22312 = CARTESIAN_POINT ( 'NONE',  ( -91.56559293963834989, 40.53558337403654832, 16.03295912088756481 ) ) ;
#22313 = CARTESIAN_POINT ( 'NONE',  ( 23.46661716383107077, 42.82867125331087266, -23.32081713244353693 ) ) ;
#22314 = CARTESIAN_POINT ( 'NONE',  ( 200.0000000000000000, 19.99999999999996447, -40.00000000000002132 ) ) ;
#22315 = ORIENTED_EDGE ( 'NONE', *, *, #21627, .F. ) ;
#22316 = CARTESIAN_POINT ( 'NONE',  ( 3.854700064722255792, -24.62824689551980839, -44.60002223906906238 ) ) ;
#22317 = CARTESIAN_POINT ( 'NONE',  ( -62.79433447042003280, -24.94280497468228930, 11.74096317481567731 ) ) ;
#22318 = CARTESIAN_POINT ( 'NONE',  ( -105.4741150117366431, -7.943527260727707429, 19.77569912956141707 ) ) ;
#22319 = EDGE_CURVE ( 'NONE', #1888, #24643, #23321, .T. ) ;
#22320 = VERTEX_POINT ( 'NONE', #25700 ) ;
#22321 = CARTESIAN_POINT ( 'NONE',  ( 23.09861257792924505, 23.40165480222934846, -42.94075326233378576 ) ) ;
#22322 = B_SPLINE_CURVE_WITH_KNOTS ( 'NONE', 3,
 ( #23177, #20517, #20784, #14519, #4562, #4425, #2555, #10671, #7309, #21554, #25562, #960, #15423, #23673, #9314, #5453, #25684, #23550, #21427, #25305, #23798, #17546, #19549, #13554, #5321, #21681, #7432, #19674, #7182, #25814, #13061, #1335, #17421, #2953 ),
 .UNSPECIFIED., .F., .F.,
 ( 4, 2, 2, 2, 2, 2, 2, 2, 2, 2, 2, 2, 2, 2, 2, 2, 4 ),
 ( -5.298243351203664762E-05, 0.01887868273877483377, 0.02834451532491826659, 0.03071097347145414561, 0.03307743161799002463, 0.03544388976452590018, 0.03781034791106178267, 0.04254326420413354071, 0.04727618049720529875, 0.04964263864374118124, 0.05200909679027704985, 0.05674201308334873156, 0.05910847122988461405, 0.06029170030315258999, 0.06147492937642056593, 0.06620784566949247663, 0.07567367825563631190 ),
 .UNSPECIFIED. ) ;
#22323 = CARTESIAN_POINT ( 'NONE',  ( 200.0000000000002274, -14.59760583945227808, 12.17906594671359244 ) ) ;
#22324 = CARTESIAN_POINT ( 'NONE',  ( 2.332272417612619719, -24.49123061639008370, 44.41409500755982975 ) ) ;
#22325 = CARTESIAN_POINT ( 'NONE',  ( 22.37977766477551356, 23.55755712319015061, -43.15105302556542455 ) ) ;
#22326 = CARTESIAN_POINT ( 'NONE',  ( 199.0097193260481561, -3.097360908056462137, -19.75623422735097989 ) ) ;
#22327 = CARTESIAN_POINT ( 'NONE',  ( 73.43438319820711513, -28.18283897611635069, 9.843172589489940449 ) ) ;
#22328 = CARTESIAN_POINT ( 'NONE',  ( 153.3020327024398171, -28.42252382389432341, 11.77299484472919922 ) ) ;
#22329 = CARTESIAN_POINT ( 'NONE',  ( 130.8568914410475372, 1.429239637432775288E-13, -34.05028731879788495 ) ) ;
#22330 = CARTESIAN_POINT ( 'NONE',  ( -86.96347745069644475, 12.89780903124419353, -12.89780903124389333 ) ) ;
#22331 = CARTESIAN_POINT ( 'NONE',  ( 91.82158438592158234, 17.20528682183301683, 0.000000000000000000 ) ) ;
#22332 = AXIS2_PLACEMENT_3D ( 'NONE', #1932, #21877, #25883 ) ;
#22333 = AXIS2_PLACEMENT_3D ( 'NONE', #3511, #9626, #15224 ) ;
#22335 = CARTESIAN_POINT ( 'NONE',  ( 14.38125909742180752, 10.73282306404735387, -10.73282306404708919 ) ) ;
#22334 = CARTESIAN_POINT ( 'NONE',  ( -187.7699188115417996, 23.34606611631939899, -42.84915433765981874 ) ) ;
#22336 = CARTESIAN_POINT ( 'NONE',  ( -86.96347745069645896, 21.75974354311648895, -0.000000000000000000 ) ) ;
#22337 = CARTESIAN_POINT ( 'NONE',  ( 151.7948205124836534, -6.767089262349000656, -40.00000000000002132 ) ) ;
#22338 = CARTESIAN_POINT ( 'NONE',  ( 91.82158438592158234, 22.79471317813472098, 2.449293598294708485E-15 ) ) ;
#22339 = CARTESIAN_POINT ( 'NONE',  ( -259.2033419157646676, 2.741182173978444749E-13, -30.48217210827739621 ) ) ;
#22340 = CARTESIAN_POINT ( 'NONE',  ( -198.0356074513804572, 67.44298959253333692, 10.87444709760969452 ) ) ;
#22341 = CARTESIAN_POINT ( 'NONE',  ( 98.29820294273281434, -7.653668647304240125, 18.47759065023114644 ) ) ;
#22342 = CARTESIAN_POINT ( 'NONE',  ( -100.7734535825088500, 44.31723036834907958, -12.25131212657445801 ) ) ;
#22343 = ORIENTED_EDGE ( 'NONE', *, *, #3626, .T. ) ;
#22344 = CARTESIAN_POINT ( 'NONE',  ( 163.1118516004056573, -19.27778845538761132, -19.27778845538770724 ) ) ;
#22345 = CIRCLE ( 'NONE', #15114, 15.00000000000000178 ) ;
#22346 = CARTESIAN_POINT ( 'NONE',  ( -193.0908841288066071, -14.03723590834271739, -48.38979025835740799 ) ) ;
#22347 = CARTESIAN_POINT ( 'NONE',  ( 57.59792236341147031, 37.56421063658187620, -40.00000000000002132 ) ) ;
#22348 = VERTEX_POINT ( 'NONE', #11199 ) ;
#22349 = ORIENTED_EDGE ( 'NONE', *, *, #18883, .T. ) ;
#22350 = CARTESIAN_POINT ( 'NONE',  ( -86.96347745069645896, -12.89780903124382938, -43.67073346367985920 ) ) ;
#22351 = CARTESIAN_POINT ( 'NONE',  ( 67.90397382950679628, -28.69135535083399802, -14.12691053321092483 ) ) ;
#22352 = EDGE_CURVE ( 'NONE', #19642, #5232, #15257, .T. ) ;
#22353 = ORIENTED_EDGE ( 'NONE', *, *, #6054, .T. ) ;
#22354 = CARTESIAN_POINT ( 'NONE',  ( -162.0762913951020892, 1.694272876828294194, 0.000000000000000000 ) ) ;
#22355 = CARTESIAN_POINT ( 'NONE',  ( -97.73860346101268703, -20.89580782307320206, 8.185503820996688162 ) ) ;
#22356 = ORIENTED_EDGE ( 'NONE', *, *, #6146, .F. ) ;
#22357 = CARTESIAN_POINT ( 'NONE',  ( 200.0000000000001421, 16.60215271479902910, 9.252637072649047667 ) ) ;
#22358 = CIRCLE ( 'NONE', #7458, 5.000000000000004441 ) ;
#22359 = VECTOR ( 'NONE', #17326, 1000.000000000000000 ) ;
#22360 = DIRECTION ( 'NONE',  ( 0.9352143328346287365, -0.1355013631592235090, -0.3271292286584503994 ) ) ;
#22361 = CARTESIAN_POINT ( 'NONE',  ( 199.9999999999999432, -14.14213562373096345, -14.14213562373104871 ) ) ;
#22362 = CARTESIAN_POINT ( 'NONE',  ( -187.3037411061945079, -46.64555264106432730, -13.75782484033866915 ) ) ;
#22363 =( BOUNDED_SURFACE ( )  B_SPLINE_SURFACE ( 3, 3, ( 
 ( #9451, #5592, #17557, #17816, #13825, #18087, #2266, #16090, #8374, #21958, #2136, #249, #11835, #8110, #1738, #14229, #12104, #12364, #1875, #20229, #13962, #9847, #16496, #5993, #2008, #22369, #22096, #14100, #16227, #20362 ),
 ( #15955, #19954, #9978, #26238, #10374, #24220, #24621, #3732, #10246, #24357, #17950, #6121, #26097, #4145, #10113, #18213, #24082, #7833, #5856, #8239, #22229, #12238, #4005, #3871, #18356, #11972, #6252, #22496, #14365, #135 ),
 ( #6376, #16357, #4275, #20493, #24491, #18485, #266, #20097, #7972, #405, #10912, #19023, #20893, #8508, #4925, #12632, #14755, #2397, #25153, #932, #12495, #18622, #2928, #17146, #6774, #21018, #20759, #538, #12766, #14886 ),
 ( #2670, #4401, #20622, #10508, #802, #23026, #12902, #11037, #8643, #18888, #2801, #8907, #4801, #22626, #25021, #16625, #25280, #19147, #24756, #14495, #667, #4664, #6509, #10646, #14620, #17017, #9041, #13036, #6904, #22757 ),
 ( #23151, #4535, #6641, #10775, #16752, #18756, #2529, #24886, #15021, #21154, #22885, #8776, #16889, #15402, #7034, #17649, #9417, #1572, #7288, #3179, #11530, #15522, #3558, #23650, #25790, #9676, #21656, #9293, #7539, #11402 ),
 ( #23527, #17398, #11662, #19525, #5055, #25537, #1187, #3306, #1309, #25409, #21786, #5298, #1440, #13408, #25662, #1057, #13161, #21406, #11285, #13663, #21531, #19786, #15151, #13532, #17524, #23279, #7408, #21281, #5431, #3429 ),
 ( #3054, #19654, #17782, #11159, #9541, #15652, #23776, #5554, #19274, #9163, #5182, #13285, #17275, #7160, #23406, #15276, #19405, #8207, #10212, #26202, #24326, #22329, #5683, #11936, #11801, #4105, #12205, #5956, #19921, #16325 ) ),
 .UNSPECIFIED., .T., .F., .F. ) 
 B_SPLINE_SURFACE_WITH_KNOTS ( ( 4, 3, 4 ),
 ( 4, 2, 2, 2, 2, 2, 2, 2, 2, 2, 2, 2, 2, 2, 4 ),
 ( 0.000000000000000000, 0.5000000000000000000, 1.000000000000000000 ),
 ( 0.000000000000000000, 0.1357259735107005372, 0.1651108541090157700, 0.1944957347073310028, 0.3598804999793158710, 0.3867117631979620773, 0.4135430264166082281, 0.5789277916885930964, 0.6062785021374117456, 0.6336292125862302838, 0.8508620842112317728, 0.8814014469398914198, 0.9119408096685510667, 0.9559704048342755334, 1.000000000000000000 ),
 .UNSPECIFIED. ) 
 GEOMETRIC_REPRESENTATION_ITEM ( )  RATIONAL_B_SPLINE_SURFACE ( (
 ( 1.000000000000000000, 1.000000000000000000, 1.000000000000000000, 1.000000000000000000, 1.000000000000000000, 1.000000000000000000, 1.000000000000000000, 1.000000000000000000, 1.000000000000000000, 1.000000000000000000, 1.000000000000000000, 1.000000000000000000, 1.000000000000000000, 1.000000000000000000, 1.000000000000000000, 1.000000000000000000, 1.000000000000000000, 1.000000000000000000, 1.000000000000000000, 1.000000000000000000, 1.000000000000000000, 1.000000000000000000, 1.000000000000000000, 1.000000000000000000, 1.000000000000000000, 1.000000000000000000, 1.000000000000000000, 1.000000000000000000, 1.000000000000000000, 1.000000000000000000),
 ( 0.3333333333333333703, 0.3333333333333333703, 0.3333333333333333703, 0.3333333333333333703, 0.3333333333333333703, 0.3333333333333333703, 0.3333333333333333703, 0.3333333333333333703, 0.3333333333333333703, 0.3333333333333333703, 0.3333333333333333703, 0.3333333333333333703, 0.3333333333333333703, 0.3333333333333333703, 0.3333333333333333703, 0.3333333333333333703, 0.3333333333333333703, 0.3333333333333333703, 0.3333333333333333703, 0.3333333333333333703, 0.3333333333333333703, 0.3333333333333333703, 0.3333333333333333703, 0.3333333333333333703, 0.3333333333333333703, 0.3333333333333333703, 0.3333333333333333703, 0.3333333333333333703, 0.3333333333333333703, 0.3333333333333333703),
 ( 0.3333333333333333703, 0.3333333333333333703, 0.3333333333333333703, 0.3333333333333333703, 0.3333333333333333703, 0.3333333333333333703, 0.3333333333333333703, 0.3333333333333333703, 0.3333333333333333703, 0.3333333333333333703, 0.3333333333333333703, 0.3333333333333333703, 0.3333333333333333703, 0.3333333333333333703, 0.3333333333333333703, 0.3333333333333333703, 0.3333333333333333703, 0.3333333333333333703, 0.3333333333333333703, 0.3333333333333333703, 0.3333333333333333703, 0.3333333333333333703, 0.3333333333333333703, 0.3333333333333333703, 0.3333333333333333703, 0.3333333333333333703, 0.3333333333333333703, 0.3333333333333333703, 0.3333333333333333703, 0.3333333333333333703),
 ( 1.000000000000000000, 1.000000000000000000, 1.000000000000000000, 1.000000000000000000, 1.000000000000000000, 1.000000000000000000, 1.000000000000000000, 1.000000000000000000, 1.000000000000000000, 1.000000000000000000, 1.000000000000000000, 1.000000000000000000, 1.000000000000000000, 1.000000000000000000, 1.000000000000000000, 1.000000000000000000, 1.000000000000000000, 1.000000000000000000, 1.000000000000000000, 1.000000000000000000, 1.000000000000000000, 1.000000000000000000, 1.000000000000000000, 1.000000000000000000, 1.000000000000000000, 1.000000000000000000, 1.000000000000000000, 1.000000000000000000, 1.000000000000000000, 1.000000000000000000),
 ( 0.3333333333333333703, 0.3333333333333333703, 0.3333333333333333703, 0.3333333333333333703, 0.3333333333333333703, 0.3333333333333333703, 0.3333333333333333703, 0.3333333333333333703, 0.3333333333333333703, 0.3333333333333333703, 0.3333333333333333703, 0.3333333333333333703, 0.3333333333333333703, 0.3333333333333333703, 0.3333333333333333703, 0.3333333333333333703, 0.3333333333333333703, 0.3333333333333333703, 0.3333333333333333703, 0.3333333333333333703, 0.3333333333333333703, 0.3333333333333333703, 0.3333333333333333703, 0.3333333333333333703, 0.3333333333333333703, 0.3333333333333333703, 0.3333333333333333703, 0.3333333333333333703, 0.3333333333333333703, 0.3333333333333333703),
 ( 0.3333333333333333703, 0.3333333333333333703, 0.3333333333333333703, 0.3333333333333333703, 0.3333333333333333703, 0.3333333333333333703, 0.3333333333333333703, 0.3333333333333333703, 0.3333333333333333703, 0.3333333333333333703, 0.3333333333333333703, 0.3333333333333333703, 0.3333333333333333703, 0.3333333333333333703, 0.3333333333333333703, 0.3333333333333333703, 0.3333333333333333703, 0.3333333333333333703, 0.3333333333333333703, 0.3333333333333333703, 0.3333333333333333703, 0.3333333333333333703, 0.3333333333333333703, 0.3333333333333333703, 0.3333333333333333703, 0.3333333333333333703, 0.3333333333333333703, 0.3333333333333333703, 0.3333333333333333703, 0.3333333333333333703),
 ( 1.000000000000000000, 1.000000000000000000, 1.000000000000000000, 1.000000000000000000, 1.000000000000000000, 1.000000000000000000, 1.000000000000000000, 1.000000000000000000, 1.000000000000000000, 1.000000000000000000, 1.000000000000000000, 1.000000000000000000, 1.000000000000000000, 1.000000000000000000, 1.000000000000000000, 1.000000000000000000, 1.000000000000000000, 1.000000000000000000, 1.000000000000000000, 1.000000000000000000, 1.000000000000000000, 1.000000000000000000, 1.000000000000000000, 1.000000000000000000, 1.000000000000000000, 1.000000000000000000, 1.000000000000000000, 1.000000000000000000, 1.000000000000000000, 1.000000000000000000) ) ) 
 REPRESENTATION_ITEM ( '' )  SURFACE ( )  );
#22364 = CARTESIAN_POINT ( 'NONE',  ( -192.9588430854690273, -40.00000000000024158, 54.46834944101708231 ) ) ;
#22365 = CARTESIAN_POINT ( 'NONE',  ( -280.0000000000000568, 19.99999999999995737, 40.00000000000002132 ) ) ;
#22366 = CARTESIAN_POINT ( 'NONE',  ( 136.1360204305621266, 3.511608612530757068, -3.511608612530642937 ) ) ;
#22367 = CARTESIAN_POINT ( 'NONE',  ( 199.0224671581742371, 2.272106995489924230, 19.87442369886018767 ) ) ;
#22368 = AXIS2_PLACEMENT_3D ( 'NONE', #7317, #15431, #23558 ) ;
#22369 = CARTESIAN_POINT ( 'NONE',  ( 163.1118516004056573, 1.251511021549353291E-13, -27.26290988616872824 ) ) ;
#22370 = CARTESIAN_POINT ( 'NONE',  ( 184.8905102610680444, -3.509827109981123710E-14, 19.07866798485558490 ) ) ;
#22371 = CARTESIAN_POINT ( 'NONE',  ( 192.4448373802101173, 40.00000000000012790, -20.00000000003928236 ) ) ;
#22372 = DIRECTION ( 'NONE',  ( 0.000000000000000000, -0.000000000000000000, 1.000000000000000000 ) ) ;
#22373 = CARTESIAN_POINT ( 'NONE',  ( -91.56559293963834989, -12.25131212657492874, 12.25131212657477953 ) ) ;
#22374 = CARTESIAN_POINT ( 'NONE',  ( -213.1075012329537230, -13.71589010951915810, -40.00000000000002132 ) ) ;
#22375 = CARTESIAN_POINT ( 'NONE',  ( -192.9588430854690273, -10.23066800229550388, 66.79921049721887982 ) ) ;
#22376 = CARTESIAN_POINT ( 'NONE',  ( -89.92902785008669753, -8.734793929541526225, 20.17328762787284546 ) ) ;
#22377 = CARTESIAN_POINT ( 'NONE',  ( 22.82385994800819162, -47.01156385802200788, 13.83113328680604681 ) ) ;
#22378 = CARTESIAN_POINT ( 'NONE',  ( -56.48582580120560692, 39.99999999999991473, 9.153146818114004546 ) ) ;
#22379 = CARTESIAN_POINT ( 'NONE',  ( -208.1127848780264742, 39.99999999999979394, 55.00245453010936103 ) ) ;
#22380 = CARTESIAN_POINT ( 'NONE',  ( 136.1360204305621266, 3.511608612530704665, 3.511608612530695339 ) ) ;
#22381 = CARTESIAN_POINT ( 'NONE',  ( -259.2033419157646676, 6.730120644403426944, 6.730120644403592145 ) ) ;
#22382 = CARTESIAN_POINT ( 'NONE',  ( -189.5227851116908084, -18.00253723945785822, -43.46196956062684791 ) ) ;
#22383 = CARTESIAN_POINT ( 'NONE',  ( -105.3755690713226585, -12.89780903124383471, -43.67073346367985920 ) ) ;
#22384 = ORIENTED_EDGE ( 'NONE', *, *, #18249, .T. ) ;
#22385 = CARTESIAN_POINT ( 'NONE',  ( 192.4448373802101173, -42.42640687122053578, -14.14213562370360577 ) ) ;
#22386 = CARTESIAN_POINT ( 'NONE',  ( 0.000000000000000000, 4.898587196589405926E-15, 39.99999999999994316 ) ) ;
#22387 = CARTESIAN_POINT ( 'NONE',  ( 170.2234770963711128, 24.55285855007190321, 0.000000000000000000 ) ) ;
#22388 =( LENGTH_UNIT ( ) NAMED_UNIT ( * ) SI_UNIT ( .MILLI., .METRE. ) );
#22389 = CARTESIAN_POINT ( 'NONE',  ( -30.26275506840324070, -27.08623969584554558, -29.48230279907826912 ) ) ;
#22390 = CARTESIAN_POINT ( 'NONE',  ( -200.4318156386407850, -24.83634777282063766, -44.88237417767277293 ) ) ;
#22391 = ORIENTED_EDGE ( 'NONE', *, *, #24303, .T. ) ;
#22392 = ORIENTED_EDGE ( 'NONE', *, *, #1025, .F. ) ;
#22393 = CARTESIAN_POINT ( 'NONE',  ( 199.9999999999999716, 14.28780111431841782, 12.54737623376984956 ) ) ;
#22394 = CARTESIAN_POINT ( 'NONE',  ( 22.26816181513970250, -23.58015273002475709, 43.18156009806490658 ) ) ;
#22395 = CARTESIAN_POINT ( 'NONE',  ( -6.342283169556221623, 13.66521761902655818, 46.19215417243774624 ) ) ;
#22396 = AXIS2_PLACEMENT_3D ( 'NONE', #4894, #9012, #17117 ) ;
#22397 = ORIENTED_EDGE ( 'NONE', *, *, #536, .F. ) ;
#22398 = ORIENTED_EDGE ( 'NONE', *, *, #3689, .T. ) ;
#22399 = CARTESIAN_POINT ( 'NONE',  ( 151.7948205124836534, -33.23291073765550863, -40.00000000000002132 ) ) ;
#22400 = CARTESIAN_POINT ( 'NONE',  ( 199.0062089136474128, 7.336486126005011599, -18.60345363517511430 ) ) ;
#22401 = DIRECTION ( 'NONE',  ( 0.000000000000000000, 0.000000000000000000, 1.000000000000000000 ) ) ;
#22402 = DIRECTION ( 'NONE',  ( -1.000000000000000000, -1.836970198721030181E-16, -2.465190328815661892E-32 ) ) ;
#22403 = CARTESIAN_POINT ( 'NONE',  ( 146.6084372240433709, 40.00000000000010658, -5.374981219216549810 ) ) ;
#22404 = CARTESIAN_POINT ( 'NONE',  ( 169.9999999999999716, -115.7889608577475258, 82.50000000000000000 ) ) ;
#22405 = CARTESIAN_POINT ( 'NONE',  ( -656.9134821118512946, 39.94664452722312831, -2.129547589869284607 ) ) ;
#22406 = CARTESIAN_POINT ( 'NONE',  ( -362.0709805440841365, -4.857225732735059864E-14, 10.00000000000004796 ) ) ;
#22407 = CARTESIAN_POINT ( 'NONE',  ( 199.0155347402294410, 14.70064717653387554, 13.56132639103557125 ) ) ;
#22408 = CARTESIAN_POINT ( 'NONE',  ( -114.4388184736404952, 8.352332320009658417, 20.16431396440389534 ) ) ;
#22409 = CARTESIAN_POINT ( 'NONE',  ( -4.004886986945149552, -23.45685150724343160, -43.01537795656791019 ) ) ;
#22410 = CARTESIAN_POINT ( 'NONE',  ( -198.0356074513804572, -67.44298959253333692, -10.87444709761016348 ) ) ;
#22411 = VECTOR ( 'NONE', #20505, 1000.000000000000000 ) ;
#22412 = CARTESIAN_POINT ( 'NONE',  ( -99.29480781227051978, 20.48155342677154067, -8.934325994365337920 ) ) ;
#22413 = CARTESIAN_POINT ( 'NONE',  ( -30.26275506840322294, -57.76657404653985139, 1.198031551615709844 ) ) ;
#22414 = CARTESIAN_POINT ( 'NONE',  ( 98.29820294267423719, -14.14213562374330024, 14.14213562372619926 ) ) ;
#22415 = CARTESIAN_POINT ( 'NONE',  ( 136.1360204305621266, 24.77266263493104148, 24.77266263493145004 ) ) ;
#22416 = CARTESIAN_POINT ( 'NONE',  ( -105.3755690713226585, -18.24025645688355013, 40.00000000000002132 ) ) ;
#22417 = CARTESIAN_POINT ( 'NONE',  ( -716.9846540392142060, -52.49999999999991473, 52.49999999999999289 ) ) ;
#22418 = CARTESIAN_POINT ( 'NONE',  ( -30.26275506840323004, -41.69427246844629309, 40.00000000000002132 ) ) ;
#22419 = CARTESIAN_POINT ( 'NONE',  ( -105.2331094975916130, 16.94275695785337277, 13.19829893673040644 ) ) ;
#22420 = CARTESIAN_POINT ( 'NONE',  ( 200.0000000000000000, 39.99999999999985079, 20.00000000000052225 ) ) ;
#22421 = CARTESIAN_POINT ( 'NONE',  ( 0.2972598230769886718, 38.42060263243669027, -18.14793986248710667 ) ) ;
#22422 = CARTESIAN_POINT ( 'NONE',  ( -213.1075012329537230, 13.71589010951907817, -40.00000000000002132 ) ) ;
#22423 = ORIENTED_EDGE ( 'NONE', *, *, #7424, .F. ) ;
#22425 = VERTEX_POINT ( 'NONE', #3097 ) ;
#22424 = EDGE_CURVE ( 'NONE', #13885, #17229, #18784, .T. ) ;
#22426 = CARTESIAN_POINT ( 'NONE',  ( 4.995406935893288214, 15.24977328854832770, 0.000000000000000000 ) ) ;
#22427 = CARTESIAN_POINT ( 'NONE',  ( -103.9474983245023481, -8.027156558344637816, -20.15710290851495756 ) ) ;
#22428 = CARTESIAN_POINT ( 'NONE',  ( 57.59792236341147031, 39.99999999999990763, 37.56421063658199699 ) ) ;
#22429 = CARTESIAN_POINT ( 'NONE',  ( -238.4067589809705794, 28.96627169325354956, -28.96627169325289231 ) ) ;
#22430 = CARTESIAN_POINT ( 'NONE',  ( 180.0000000000000000, 2.292407966645821729E-14, -82.49999999999998579 ) ) ;
#22431 = CARTESIAN_POINT ( 'NONE',  ( -192.1167141818822017, -43.95739236919489912, -24.15421809699812172 ) ) ;
#22432 = LINE ( 'NONE', #12562, #15181 ) ;
#22433 = CARTESIAN_POINT ( 'NONE',  ( 199.9999999999999716, 16.82276630623001878, 8.840806072347076494 ) ) ;
#22434 = CARTESIAN_POINT ( 'NONE',  ( 199.9999999999999147, -18.52392551398779830, 4.314389638746997768 ) ) ;
#22435 = CARTESIAN_POINT ( 'NONE',  ( -162.0762913951020892, 29.48230308784799902, -29.48230308784730980 ) ) ;
#22436 = CARTESIAN_POINT ( 'NONE',  ( 170.2234770963711128, -10.92277846919187034, -10.92277846919209594 ) ) ;
#22437 = DIRECTION ( 'NONE',  ( 0.9698969544411725208, -0.09318942517750300469, -0.2249791741491306285 ) ) ;
#22438 = CARTESIAN_POINT ( 'NONE',  ( 146.6084372240433993, -3.357462877844280890E-13, 34.62501878078305850 ) ) ;
#22439 = CARTESIAN_POINT ( 'NONE',  ( -280.0000000000000568, -42.42640687119305198, 14.14213562373058686 ) ) ;
#22440 = DIRECTION ( 'NONE',  ( 1.000000000000000000, 1.836970198721030427E-16, -0.000000000000000000 ) ) ;
#22441 = CARTESIAN_POINT ( 'NONE',  ( 57.59792236341147031, -1.722363176415032004, -1.722363176415048880 ) ) ;
#22442 = CARTESIAN_POINT ( 'NONE',  ( 0.2972598230770027716, -38.42060263243656237, -18.14793986248737667 ) ) ;
#22443 = DIRECTION ( 'NONE',  ( 1.000000000000000000, 1.836970198721030181E-16, 0.000000000000000000 ) ) ;
#22445 = CARTESIAN_POINT ( 'NONE',  ( 57.59792236341147742, -1.230234673553095937E-13, 37.56421063658186199 ) ) ;
#22444 = CARTESIAN_POINT ( 'NONE',  ( -198.0356074513804572, 10.87444709761036066, -67.44298959253325165 ) ) ;
#22446 = CARTESIAN_POINT ( 'NONE',  ( 130.8568914410475088, 32.49135343045448820, 24.07718906446946860 ) ) ;
#22447 = CARTESIAN_POINT ( 'NONE',  ( 23.35901252181229637, 46.81387818480130392, -13.80180065670237788 ) ) ;
#22448 = CARTESIAN_POINT ( 'NONE',  ( -259.2033419157646676, -9.517827891722680178, -40.00000000000002132 ) ) ;
#22449 = ORIENTED_EDGE ( 'NONE', *, *, #22352, .T. ) ;
#22450 = CARTESIAN_POINT ( 'NONE',  ( 21.16156876808018339, -23.80729322913531121, -43.48822901267205054 ) ) ;
#22451 = CARTESIAN_POINT ( 'NONE',  ( -4.260882601032360384, -42.93997571557835613, 23.40615483283719556 ) ) ;
#22452 = APPLICATION_CONTEXT ( 'automotive_design' ) ;
#22453 = CARTESIAN_POINT ( 'NONE',  ( -105.3755690713226727, 18.24025645688350750, 2.449293598294708485E-15 ) ) ;
#22454 = VERTEX_POINT ( 'NONE', #19313 ) ;
#22455 = CARTESIAN_POINT ( 'NONE',  ( -192.1131556193065819, -48.19965519933759168, -14.00853984552894360 ) ) ;
#22456 = CARTESIAN_POINT ( 'NONE',  ( 163.1118516004056573, -19.27778845538761132, -19.27778845538770724 ) ) ;
#22457 = CARTESIAN_POINT ( 'NONE',  ( 22.01478053666890133, -13.87318432395561807, 47.29427690643639437 ) ) ;
#22458 = CARTESIAN_POINT ( 'NONE',  ( -1.624577210452443854, 18.12534649864440084, -43.75845733971287643 ) ) ;
#22459 = CARTESIAN_POINT ( 'NONE',  ( 199.0173355507466226, -15.87315179554041045, -12.16952887920782445 ) ) ;
#22460 = DIRECTION ( 'NONE',  ( 0.000000000000000000, 0.000000000000000000, 1.000000000000000000 ) ) ;
#22461 = CARTESIAN_POINT ( 'NONE',  ( 200.0000000000000000, 63.70262460423112572, -57.69613583541415380 ) ) ;
#22462 = CARTESIAN_POINT ( 'NONE',  ( -166.7090905288631291, -15.35183918172718442, 37.06261835973858609 ) ) ;
#22463 = CARTESIAN_POINT ( 'NONE',  ( -198.0356074513804572, 10.87444709761036066, -67.44298959253325165 ) ) ;
#22464 = CARTESIAN_POINT ( 'NONE',  ( -86.95492400940779021, -6.698385205267455511, 20.33918296375446744 ) ) ;
#22465 =( BOUNDED_CURVE ( )  B_SPLINE_CURVE ( 3, ( #14291, #10310, #21221, #23469 ),
 .UNSPECIFIED., .F., .F. ) 
 B_SPLINE_CURVE_WITH_KNOTS ( ( 4, 4 ),
 ( 0.004183487405659318259, 0.01388163286937179816 ),
 .UNSPECIFIED. ) 
 CURVE ( )  GEOMETRIC_REPRESENTATION_ITEM ( )  RATIONAL_B_SPLINE_CURVE ( ( 0.6809743333591583569, 0.7608653435686173472, 0.8672072324488978579, 1.000000000000000000 ) ) 
 REPRESENTATION_ITEM ( '' )  );
#22467 = CARTESIAN_POINT ( 'NONE',  ( 130.8568914410475088, 4.207082182989012153, 52.36146031193425188 ) ) ;
#22466 = CARTESIAN_POINT ( 'NONE',  ( -190.5535808404945044, 18.10342626500584728, -43.70553721440292350 ) ) ;
#22468 = CARTESIAN_POINT ( 'NONE',  ( -86.96347745069644475, -15.38646221621807442, 15.38646221621768184 ) ) ;
#22469 = CARTESIAN_POINT ( 'NONE',  ( 57.59792236341148453, -37.56421063658185489, -2.449293598294708485E-15 ) ) ;
#22470 = CARTESIAN_POINT ( 'NONE',  ( -192.9588430854690273, 54.46834944098218756, -40.00000000000002132 ) ) ;
#22471 = CARTESIAN_POINT ( 'NONE',  ( -238.4067589809705794, -3.369206980223063916E-14, -0.9644942799825824142 ) ) ;
#22472 = CARTESIAN_POINT ( 'NONE',  ( 146.6084372240433709, -24.48358557860329299, 32.08495691632052882 ) ) ;
#22473 = CARTESIAN_POINT ( 'NONE',  ( -210.0000000000000568, 82.50000000000008527, 52.49999999999980105 ) ) ;
#22474 = CARTESIAN_POINT ( 'NONE',  ( -86.96347745069644475, -12.89780903124395195, -12.89780903124416511 ) ) ;
#22475 = ORIENTED_EDGE ( 'NONE', *, *, #19475, .F. ) ;
#22476 = CARTESIAN_POINT ( 'NONE',  ( -208.1127848780265026, 10.60833733269537049, 10.60833733269544510 ) ) ;
#22477 = CARTESIAN_POINT ( 'NONE',  ( -99.31364972219382992, 8.164808577079744722, 20.79869444143179891 ) ) ;
#22478 = VERTEX_POINT ( 'NONE', #1096 ) ;
#22479 = CARTESIAN_POINT ( 'NONE',  ( 4.995406935893310418, -67.35176059880237176, 10.78321810387813429 ) ) ;
#22480 = CARTESIAN_POINT ( 'NONE',  ( 2.692156443669315724, -44.48799183653559197, -18.42752958144988895 ) ) ;
#22481 = ORIENTED_EDGE ( 'NONE', *, *, #15010, .F. ) ;
#22482 = CARTESIAN_POINT ( 'NONE',  ( -96.93773665438737908, -20.92028269119444062, 8.190703376740682273 ) ) ;
#22483 = PLANE ( 'NONE',  #4970 ) ;
#22484 = VECTOR ( 'NONE', #7111, 1000.000000000000000 ) ;
#22485 = EDGE_LOOP ( 'NONE', ( #8792, #5014 ) ) ;
#22486 = CARTESIAN_POINT ( 'NONE',  ( 200.0000000000000284, 9.630262036685882876, 16.38694142346205140 ) ) ;
#22487 = CARTESIAN_POINT ( 'NONE',  ( -211.2619052429883482, 0.000000000000000000, -75.00000000000000000 ) ) ;
#22488 = CARTESIAN_POINT ( 'NONE',  ( 151.7948205124836250, -23.49921654116339553, -23.49921654116350211 ) ) ;
#22489 = CARTESIAN_POINT ( 'NONE',  ( -166.3490736461147605, -36.43932733827825388, -19.13702016920204230 ) ) ;
#22490 = ADVANCED_FACE ( 'NONE', ( #25449 ), #9756, .T. ) ;
#22491 = CARTESIAN_POINT ( 'NONE',  ( -100.7734535825088500, -40.00000000000009948, 17.32597176626796909 ) ) ;
#22492 = CARTESIAN_POINT ( 'NONE',  ( 170.2234770963711128, -24.55285855007184281, 40.00000000000002132 ) ) ;
#22493 = CARTESIAN_POINT ( 'NONE',  ( -135.8532207217289738, -34.75652343174584757, -21.81201906317816253 ) ) ;
#22494 = CARTESIAN_POINT ( 'NONE',  ( -626.9846540392142060, 105.0000000000000000, 0.000000000000000000 ) ) ;
#22495 = EDGE_CURVE ( 'NONE', #14842, #18547, #12472, .T. ) ;
#22496 = CARTESIAN_POINT ( 'NONE',  ( 184.8905102610680444, -39.99999999999991473, -20.92133201514458207 ) ) ;
#22497 = CARTESIAN_POINT ( 'NONE',  ( -135.8532207217289738, -1.351063376314938213E-13, 30.84685318188645553 ) ) ;
#22498 = CARTESIAN_POINT ( 'NONE',  ( -213.1075012329537230, 39.99999999999992895, 13.71589010951925935 ) ) ;
#22499 = CARTESIAN_POINT ( 'NONE',  ( -135.8532207217289738, 9.153146818113548022, -40.00000000000002132 ) ) ;
#22500 = CARTESIAN_POINT ( 'NONE',  ( 146.6084372240433993, -3.800685668858652999, 3.800685668858636568 ) ) ;
#22501 = EDGE_CURVE ( 'NONE', #8967, #21371, #3564, .T. ) ;
#22502 = CARTESIAN_POINT ( 'NONE',  ( 19.06497207195982924, -54.19242893257843008, -2.449293598294708485E-15 ) ) ;
#22503 = EDGE_CURVE ( 'NONE', #3292, #6406, #7032, .T. ) ;
#22504 = CARTESIAN_POINT ( 'NONE',  ( -280.0000000000000568, 42.42640687119274645, 14.14213562373118194 ) ) ;
#22505 = CARTESIAN_POINT ( 'NONE',  ( -175.9234132812216842, 12.95567001274190133, 42.70618379781711837 ) ) ;
#22506 = DIRECTION ( 'NONE',  ( -1.000000000000000000, 1.836970198721030181E-16, 0.000000000000000000 ) ) ;
#22507 = CARTESIAN_POINT ( 'NONE',  ( 163.1118516004056573, 39.99999999999976552, 27.26290988616914746 ) ) ;
#22508 = CARTESIAN_POINT ( 'NONE',  ( 130.8568914410475088, -40.00000000000001421, 5.949712681206549725 ) ) ;
#22509 = CARTESIAN_POINT ( 'NONE',  ( -100.7734535825088500, 40.53558337403677569, -16.03295912088699993 ) ) ;
#22510 = CARTESIAN_POINT ( 'NONE',  ( 85.88436334084022405, -10.32541289738165524, 22.72801779375535958 ) ) ;
#22511 = CARTESIAN_POINT ( 'NONE',  ( -626.9846540392142060, 90.00000000000000000, -74.99999999999991473 ) ) ;
#22512 = CARTESIAN_POINT ( 'NONE',  ( -192.9588430854690273, -66.79921049724377724, 10.23066800231950069 ) ) ;
#22513 = EDGE_LOOP ( 'NONE', ( #18604, #3859, #12782, #5974 ) ) ;
#22514 = CARTESIAN_POINT ( 'NONE',  ( -30.26275506840324070, 1.198031551616030033, -1.198031551616006496 ) ) ;
#22515 = CARTESIAN_POINT ( 'NONE',  ( -190.0000000000000000, -52.49999999999972289, -82.49999999999998579 ) ) ;
#22516 = CARTESIAN_POINT ( 'NONE',  ( 91.82158438592156813, 17.20528682183302038, -40.00000000000002132 ) ) ;
#22517 = DIRECTION ( 'NONE',  ( -1.000000000000000000, -0.000000000000000000, -0.000000000000000000 ) ) ;
#22518 =( NAMED_UNIT ( * ) SI_UNIT ( $, .STERADIAN. ) SOLID_ANGLE_UNIT ( ) );
#22519 = EDGE_LOOP ( 'NONE', ( #8432, #3903 ) ) ;
#22520 = ORIENTED_EDGE ( 'NONE', *, *, #543, .T. ) ;
#22521 = CARTESIAN_POINT ( 'NONE',  ( 199.9999999999999432, 6.682224494514668933, 17.80490695329945439 ) ) ;
#22522 = LINE ( 'NONE', #26262, #12362 ) ;
#22523 = CARTESIAN_POINT ( 'NONE',  ( 23.37583784646054141, 23.33923448557714053, 42.85659535397683584 ) ) ;
#22524 = ORIENTED_EDGE ( 'NONE', *, *, #20455, .T. ) ;
#22525 = ORIENTED_EDGE ( 'NONE', *, *, #795, .F. ) ;
#22526 =( BOUNDED_SURFACE ( )  B_SPLINE_SURFACE ( 3, 3, ( 
 ( #16126, #26273, #9616, #20130, #25861, #26130, #1909, #26001, #15849, #8147, #23979, #17982, #21997, #3631, #11871, #11600, #19857, #3910, #9881, #1776, #3767, #19991, #7871, #10013, #1643, #9751, #4042, #2044, #15993, #35 ),
 ( #5892, #7606, #15721, #14000, #18121, #8011, #24256, #6029, #1509, #14136, #22267, #23846, #24390, #12141, #20265, #10151, #5625, #18254, #16261, #13731, #13596, #21857, #3502, #6157, #16662, #24528, #22532, #22664, #18525, #4436 ),
 ( #307, #14794, #20799, #2711, #20663, #577, #18391, #8546, #4573, #22925, #2571, #4179, #2298, #14266, #16531, #4313, #24929, #24794, #10545, #12670, #20528, #10816, #18656, #22403, #8684, #18796, #2175, #10685, #10282, #443 ),
 ( #12273, #6546, #20401, #14655, #12530, #2433, #12810, #16792, #22796, #24659, #6679, #16399, #4706, #14402, #20932, #168, #18929, #711, #8815, #16926, #8274, #6284, #12403, #10408, #6416, #8409, #14533, #19309, #25445, #23187 ),
 ( #3093, #7197, #972, #10952, #15434, #4967, #25317, #12942, #9326, #11439, #23064, #2844, #13445, #1353, #17313, #5214, #13076, #11074, #23318, #15312, #19058, #21565, #23438, #21191, #19188, #7320, #13318, #3338, #13198, #19435 ),
 ( #9076, #1222, #23561, #25574, #2963, #17182, #5093, #11195, #17437, #11319, #25060, #15190, #21057, #7076, #840, #21438, #19561, #5336, #9452, #6812, #14928, #1092, #4836, #8950, #21320, #9201, #3212, #17059, #25192, #6940 ),
 ( #15058, #10340, #12459, #6216, #18449, #7446, #21693, #3469, #4369, #8340, #23811, #16190, #14328, #226, #5593, #9713, #11568, #19686, #12203, #18315, #15686, #16323, #11701, #23685, #98, #21824, #1475, #2361, #13699, #25965 ) ),
 .UNSPECIFIED., .T., .F., .F. ) 
 B_SPLINE_SURFACE_WITH_KNOTS ( ( 4, 3, 4 ),
 ( 4, 2, 2, 2, 2, 2, 2, 2, 2, 2, 2, 2, 2, 2, 4 ),
 ( 0.000000000000000000, 0.5000000000000000000, 1.000000000000000000 ),
 ( 0.000000000000000000, 0.1357259735107005372, 0.1651108541090157700, 0.1944957347073310028, 0.3598804999793158710, 0.3867117631979620773, 0.4135430264166082281, 0.5789277916885930964, 0.6062785021374117456, 0.6336292125862302838, 0.8508620842112317728, 0.8814014469398914198, 0.9119408096685510667, 0.9559704048342755334, 1.000000000000000000 ),
 .UNSPECIFIED. ) 
 GEOMETRIC_REPRESENTATION_ITEM ( )  RATIONAL_B_SPLINE_SURFACE ( (
 ( 1.000000000000000000, 1.000000000000000000, 1.000000000000000000, 1.000000000000000000, 1.000000000000000000, 1.000000000000000000, 1.000000000000000000, 1.000000000000000000, 1.000000000000000000, 1.000000000000000000, 1.000000000000000000, 1.000000000000000000, 1.000000000000000000, 1.000000000000000000, 1.000000000000000000, 1.000000000000000000, 1.000000000000000000, 1.000000000000000000, 1.000000000000000000, 1.000000000000000000, 1.000000000000000000, 1.000000000000000000, 1.000000000000000000, 1.000000000000000000, 1.000000000000000000, 1.000000000000000000, 1.000000000000000000, 1.000000000000000000, 1.000000000000000000, 1.000000000000000000),
 ( 0.3333333333333333703, 0.3333333333333333703, 0.3333333333333333703, 0.3333333333333333703, 0.3333333333333333703, 0.3333333333333333703, 0.3333333333333333703, 0.3333333333333333703, 0.3333333333333333703, 0.3333333333333333703, 0.3333333333333333703, 0.3333333333333333703, 0.3333333333333333703, 0.3333333333333333703, 0.3333333333333333703, 0.3333333333333333703, 0.3333333333333333703, 0.3333333333333333703, 0.3333333333333333703, 0.3333333333333333703, 0.3333333333333333703, 0.3333333333333333703, 0.3333333333333333703, 0.3333333333333333703, 0.3333333333333333703, 0.3333333333333333703, 0.3333333333333333703, 0.3333333333333333703, 0.3333333333333333703, 0.3333333333333333703),
 ( 0.3333333333333333703, 0.3333333333333333703, 0.3333333333333333703, 0.3333333333333333703, 0.3333333333333333703, 0.3333333333333333703, 0.3333333333333333703, 0.3333333333333333703, 0.3333333333333333703, 0.3333333333333333703, 0.3333333333333333703, 0.3333333333333333703, 0.3333333333333333703, 0.3333333333333333703, 0.3333333333333333703, 0.3333333333333333703, 0.3333333333333333703, 0.3333333333333333703, 0.3333333333333333703, 0.3333333333333333703, 0.3333333333333333703, 0.3333333333333333703, 0.3333333333333333703, 0.3333333333333333703, 0.3333333333333333703, 0.3333333333333333703, 0.3333333333333333703, 0.3333333333333333703, 0.3333333333333333703, 0.3333333333333333703),
 ( 1.000000000000000000, 1.000000000000000000, 1.000000000000000000, 1.000000000000000000, 1.000000000000000000, 1.000000000000000000, 1.000000000000000000, 1.000000000000000000, 1.000000000000000000, 1.000000000000000000, 1.000000000000000000, 1.000000000000000000, 1.000000000000000000, 1.000000000000000000, 1.000000000000000000, 1.000000000000000000, 1.000000000000000000, 1.000000000000000000, 1.000000000000000000, 1.000000000000000000, 1.000000000000000000, 1.000000000000000000, 1.000000000000000000, 1.000000000000000000, 1.000000000000000000, 1.000000000000000000, 1.000000000000000000, 1.000000000000000000, 1.000000000000000000, 1.000000000000000000),
 ( 0.3333333333333333703, 0.3333333333333333703, 0.3333333333333333703, 0.3333333333333333703, 0.3333333333333333703, 0.3333333333333333703, 0.3333333333333333703, 0.3333333333333333703, 0.3333333333333333703, 0.3333333333333333703, 0.3333333333333333703, 0.3333333333333333703, 0.3333333333333333703, 0.3333333333333333703, 0.3333333333333333703, 0.3333333333333333703, 0.3333333333333333703, 0.3333333333333333703, 0.3333333333333333703, 0.3333333333333333703, 0.3333333333333333703, 0.3333333333333333703, 0.3333333333333333703, 0.3333333333333333703, 0.3333333333333333703, 0.3333333333333333703, 0.3333333333333333703, 0.3333333333333333703, 0.3333333333333333703, 0.3333333333333333703),
 ( 0.3333333333333333703, 0.3333333333333333703, 0.3333333333333333703, 0.3333333333333333703, 0.3333333333333333703, 0.3333333333333333703, 0.3333333333333333703, 0.3333333333333333703, 0.3333333333333333703, 0.3333333333333333703, 0.3333333333333333703, 0.3333333333333333703, 0.3333333333333333703, 0.3333333333333333703, 0.3333333333333333703, 0.3333333333333333703, 0.3333333333333333703, 0.3333333333333333703, 0.3333333333333333703, 0.3333333333333333703, 0.3333333333333333703, 0.3333333333333333703, 0.3333333333333333703, 0.3333333333333333703, 0.3333333333333333703, 0.3333333333333333703, 0.3333333333333333703, 0.3333333333333333703, 0.3333333333333333703, 0.3333333333333333703),
 ( 1.000000000000000000, 1.000000000000000000, 1.000000000000000000, 1.000000000000000000, 1.000000000000000000, 1.000000000000000000, 1.000000000000000000, 1.000000000000000000, 1.000000000000000000, 1.000000000000000000, 1.000000000000000000, 1.000000000000000000, 1.000000000000000000, 1.000000000000000000, 1.000000000000000000, 1.000000000000000000, 1.000000000000000000, 1.000000000000000000, 1.000000000000000000, 1.000000000000000000, 1.000000000000000000, 1.000000000000000000, 1.000000000000000000, 1.000000000000000000, 1.000000000000000000, 1.000000000000000000, 1.000000000000000000, 1.000000000000000000, 1.000000000000000000, 1.000000000000000000) ) ) 
 REPRESENTATION_ITEM ( '' )  SURFACE ( )  );
#22527 = CARTESIAN_POINT ( 'NONE',  ( -259.2033419157646676, -9.517827891722680178, 0.000000000000000000 ) ) ;
#22528 = CARTESIAN_POINT ( 'NONE',  ( 199.0135655005340425, -10.56572504866429973, -16.98073106299600710 ) ) ;
#22529 = CARTESIAN_POINT ( 'NONE',  ( -199.9999999999999716, -44.86878812508714276, 24.82633483071253622 ) ) ;
#22530 = CARTESIAN_POINT ( 'NONE',  ( -97.73860346099715457, -8.185503821079883835, -20.89580782303697859 ) ) ;
#22531 = VECTOR ( 'NONE', #19006, 1000.000000000000114 ) ;
#22532 = CARTESIAN_POINT ( 'NONE',  ( 170.2234770963711128, 39.99999999999980105, 24.55285855007229401 ) ) ;
#22533 = CARTESIAN_POINT ( 'NONE',  ( 170.2234770963711128, -2.259079968736224833E-13, 24.55285855007187124 ) ) ;
#22534 = LINE ( 'NONE', #20530, #9188 ) ;
#22535 = CYLINDRICAL_SURFACE ( 'NONE', #2627, 5.000000000000004441 ) ;
#22536 = CARTESIAN_POINT ( 'NONE',  ( 199.0196638708318631, 8.237985373594881366, 18.22956011771260165 ) ) ;
#22537 = CARTESIAN_POINT ( 'NONE',  ( -184.9729924864046779, 22.80024897326492450, 42.02333070177070340 ) ) ;
#22538 = CARTESIAN_POINT ( 'NONE',  ( 17.65190074000382126, -24.35922420887711226, -44.23515346911565871 ) ) ;
#22539 = CARTESIAN_POINT ( 'NONE',  ( 4.995406935893312195, -67.35176059882525124, -10.78321810390210445 ) ) ;
#22540 = CARTESIAN_POINT ( 'NONE',  ( -200.0000000000000284, 20.93268228684348387, 45.36622447512526435 ) ) ;
#22541 = CARTESIAN_POINT ( 'NONE',  ( -213.1075012329537230, 18.58567234101121102, 37.98287015391247223 ) ) ;
#22542 = LINE ( 'NONE', #18535, #1086 ) ;
#22543 = CARTESIAN_POINT ( 'NONE',  ( 184.8905102610680444, 14.79361573936375507, 14.79361573936398067 ) ) ;
#22544 = CARTESIAN_POINT ( 'NONE',  ( -100.7734535825088500, 22.67402823373189946, 40.00000000000002132 ) ) ;
#22545 = CARTESIAN_POINT ( 'NONE',  ( -162.0762913951020892, 1.198031840385732849, -1.198031840385733515 ) ) ;
#22546 = CARTESIAN_POINT ( 'NONE',  ( -162.0762913951020607, -41.69427287682838568, -2.449293598294708485E-15 ) ) ;
#22547 = CARTESIAN_POINT ( 'NONE',  ( -99.29480781227073294, 20.80016781325170427, -8.165122821357643446 ) ) ;
#22548 = CARTESIAN_POINT ( 'NONE',  ( 14.38125909742180220, 40.00000000000017764, -15.17850393972591760 ) ) ;
#22549 = CARTESIAN_POINT ( 'NONE',  ( 192.4448373802101173, 14.14213562370320076, -42.42640687122072762 ) ) ;
#22550 = CARTESIAN_POINT ( 'NONE',  ( -100.7734535825088358, -22.67402823373193499, 0.000000000000000000 ) ) ;
#22551 = ORIENTED_EDGE ( 'NONE', *, *, #3062, .T. ) ;
#22552 = CIRCLE ( 'NONE', #5527, 5.000000000000011546 ) ;
#22553 = ORIENTED_EDGE ( 'NONE', *, *, #17278, .T. ) ;
#22554 = VERTEX_POINT ( 'NONE', #1844 ) ;
#22555 = CARTESIAN_POINT ( 'NONE',  ( 146.6084372240433993, -34.62501878078303008, 0.000000000000000000 ) ) ;
#22556 = CARTESIAN_POINT ( 'NONE',  ( 158.3379117892987722, 10.98149362779600935, 26.51167085133962686 ) ) ;
#22557 = CARTESIAN_POINT ( 'NONE',  ( -30.26275506840325136, 57.76657404653985139, -1.198031551615314161 ) ) ;
#22558 = CARTESIAN_POINT ( 'NONE',  ( -114.4940140763995373, -20.58897208713957738, -7.440456728211662707 ) ) ;
#22559 = CARTESIAN_POINT ( 'NONE',  ( 199.9999999999999432, -20.00000000000006750, 0.000000000000000000 ) ) ;
#22560 = LINE ( 'NONE', #24687, #1171 ) ;
#22561 = CARTESIAN_POINT ( 'NONE',  ( 199.9999999999998863, 18.74710533595338546, 3.118879735276928855 ) ) ;
#22562 = CARTESIAN_POINT ( 'NONE',  ( 199.9999999999999432, 3.553227108789564159, -18.66636905392490675 ) ) ;
#22563 = CARTESIAN_POINT ( 'NONE',  ( 192.4448373802101173, -14.14213562375826605, -42.42640687116518450 ) ) ;
#22564 = CARTESIAN_POINT ( 'NONE',  ( -259.2033419157646676, -49.83842185052040463, 6.730120644403092101 ) ) ;
#22565 = FACE_OUTER_BOUND ( 'NONE', #14389, .T. ) ;
#22566 = CARTESIAN_POINT ( 'NONE',  ( 57.59792236341147031, 40.00000000000042633, -37.56421063658144277 ) ) ;
#22567 = CARTESIAN_POINT ( 'NONE',  ( -192.9588430854690273, -38.51493924976957572, 18.05360324515410397 ) ) ;
#22568 = EDGE_CURVE ( 'NONE', #7623, #13247, #5970, .T. ) ;
#22569 = CARTESIAN_POINT ( 'NONE',  ( -16.41532015099270225, 12.95569205221179487, 42.70629200725615959 ) ) ;
#22570 = CARTESIAN_POINT ( 'NONE',  ( -162.0762913951020892, 1.198031840385716418, 1.198031840385750169 ) ) ;
#22571 = CARTESIAN_POINT ( 'NONE',  ( -100.7734535825088500, -40.53558337403669753, -16.03295912088728770 ) ) ;
#22572 = CARTESIAN_POINT ( 'NONE',  ( 199.0189648287746991, 9.496445123477679218, 17.61199005508735738 ) ) ;
#22574 = CARTESIAN_POINT ( 'NONE',  ( 57.59792236341147031, 39.99999999999990763, 37.56421063658199699 ) ) ;
#22573 = CARTESIAN_POINT ( 'NONE',  ( 184.8905102610680444, 13.49065550809826952, -13.49065550809790359 ) ) ;
#22575 = CARTESIAN_POINT ( 'NONE',  ( 170.2234770963711128, 39.20704971665372796, 17.36149277827039583 ) ) ;
#22576 = CARTESIAN_POINT ( 'NONE',  ( 25.62979979003352682, 42.16299361907574905, -22.88075396656789806 ) ) ;
#22577 = CARTESIAN_POINT ( 'NONE',  ( 130.8568914410475372, 5.949712681206715814, 2.449293598294708485E-15 ) ) ;
#22578 = CARTESIAN_POINT ( 'NONE',  ( 19.06497207195981503, -14.19242893257840166, 0.000000000000000000 ) ) ;
#22579 = CARTESIAN_POINT ( 'NONE',  ( 151.7948205124836250, -23.49921654116339553, -23.49921654116350211 ) ) ;
#22580 = CARTESIAN_POINT ( 'NONE',  ( -5.152948516943141044, -46.60473671797108608, 13.74948675458158753 ) ) ;
#22581 = CIRCLE ( 'NONE', #19180, 30.00000000000000355 ) ;
#22582 = CARTESIAN_POINT ( 'NONE',  ( -105.3755690713226585, 18.24025645688349684, 40.00000000000002132 ) ) ;
#22583 = EDGE_CURVE ( 'NONE', #23054, #13433, #19791, .T. ) ;
#22584 = ORIENTED_EDGE ( 'NONE', *, *, #24446, .F. ) ;
#22585 = CARTESIAN_POINT ( 'NONE',  ( 4.990269915386266852, 24.74342916192447817, -44.75621547178034376 ) ) ;
#22586 = AXIS2_PLACEMENT_3D ( 'NONE', #12277, #10286, #19994 ) ;
#22587 = CARTESIAN_POINT ( 'NONE',  ( -135.8532207217289738, -6.472252184284190690, -6.472252184284188914 ) ) ;
#22588 = DIRECTION ( 'NONE',  ( 1.000000000000000000, 0.000000000000000000, 0.000000000000000000 ) ) ;
#22589 = ADVANCED_FACE ( 'NONE', ( #14202 ), #2108, .T. ) ;
#22590 = CARTESIAN_POINT ( 'NONE',  ( -3.434479974377871780, 17.93814274724503122, -43.30650750418230643 ) ) ;
#22591 = CARTESIAN_POINT ( 'NONE',  ( 199.0145894657785846, -12.18649378798404470, -15.86093292504746621 ) ) ;
#22592 = CARTESIAN_POINT ( 'NONE',  ( -65.65510974524528365, -24.89665924127696783, -9.107311025939324622 ) ) ;
#22593 = CARTESIAN_POINT ( 'NONE',  ( 159.7744820660626885, -25.95909830917692673, 10.75261058663734026 ) ) ;
#22594 = CARTESIAN_POINT ( 'NONE',  ( -189.2667921706068626, -17.97629039507247484, 43.39860407294408873 ) ) ;
#22595 = CARTESIAN_POINT ( 'NONE',  ( -213.1075012329537230, 9.698598906450543566, -9.698598906450348167 ) ) ;
#22596 = CARTESIAN_POINT ( 'NONE',  ( 170.0000000000000000, 24.25569233607184216, 6.285860131565298659 ) ) ;
#22597 = VECTOR ( 'NONE', #2524, 1000.000000000000114 ) ;
#22599 = CARTESIAN_POINT ( 'NONE',  ( 146.6084372240433709, 3.800685668858042821, 52.76785682606522698 ) ) ;
#22598 = CARTESIAN_POINT ( 'NONE',  ( -195.1685814578629561, 14.09692187699488031, -48.78510996054859561 ) ) ;
#22600 = CARTESIAN_POINT ( 'NONE',  ( 14.38125909742180752, 10.73282306404735387, -10.73282306404708919 ) ) ;
#22601 = CARTESIAN_POINT ( 'NONE',  ( 4.995406935893309530, -55.24977328856464709, 40.00000000000002132 ) ) ;
#22602 = CARTESIAN_POINT ( 'NONE',  ( 136.1360204305621551, 4.966164525587085876, 40.00000000000002132 ) ) ;
#22603 = CARTESIAN_POINT ( 'NONE',  ( -192.9588430854690273, -39.99999999999991473, -14.46834944100011633 ) ) ;
#22604 = CARTESIAN_POINT ( 'NONE',  ( -56.48582580120559271, 21.81201906317768291, 21.81201906317777173 ) ) ;
#22605 = CARTESIAN_POINT ( 'NONE',  ( -162.0762913951020892, -29.48230308784744125, -29.48230308784792442 ) ) ;
#22606 = ADVANCED_BREP_SHAPE_REPRESENTATION ( '', ( #8975, #21058 ), #2358 ) ;
#22607 = DIRECTION ( 'NONE',  ( 1.000000000000000000, 0.000000000000000000, 0.000000000000000000 ) ) ;
#22608 = VERTEX_POINT ( 'NONE', #25797 ) ;
#22609 = CARTESIAN_POINT ( 'NONE',  ( -238.4067589809705794, 0.6820004457912757223, 0.6820004457913219076 ) ) ;
#22610 = CARTESIAN_POINT ( 'NONE',  ( -189.4799804244526626, -13.88847367996405069, -47.39666776706570062 ) ) ;
#22611 = CONTEXT_DEPENDENT_SHAPE_REPRESENTATION ( #12936, #8268 ) ;
#22612 = CARTESIAN_POINT ( 'NONE',  ( -238.4067589809705794, -0.6820004458488042598, 57.25054294077229855 ) ) ;
#22613 = CARTESIAN_POINT ( 'NONE',  ( -3.117754532602394324, -43.38723640139033222, -17.97158175134525493 ) ) ;
#22614 = ORIENTED_EDGE ( 'NONE', *, *, #25555, .F. ) ;
#22615 = CARTESIAN_POINT ( 'NONE',  ( -93.02511667906844650, -20.82219708225688493, 8.169918093965387484 ) ) ;
#22616 = CARTESIAN_POINT ( 'NONE',  ( -87.02160135033209087, -10.86113943608616239, -18.50856326151600939 ) ) ;
#22617 = VERTEX_POINT ( 'NONE', #20196 ) ;
#22618 = CARTESIAN_POINT ( 'NONE',  ( 199.9999999999998863, 18.50936851023984886, -4.296315843485498220 ) ) ;
#22619 = VECTOR ( 'NONE', #11455, 1000.000000000000000 ) ;
#22620 = DIRECTION ( 'NONE',  ( -1.000000000000000000, -0.000000000000000000, -0.000000000000000000 ) ) ;
#22621 = CARTESIAN_POINT ( 'NONE',  ( -190.7346372394394791, -47.78727444206358399, -13.94676542151541021 ) ) ;
#22622 = CARTESIAN_POINT ( 'NONE',  ( 163.1118516004056573, -39.99999999999990052, -27.26290988616886679 ) ) ;
#22623 = CARTESIAN_POINT ( 'NONE',  ( 146.6084372240433709, 5.374981219216996564, 40.00000000000002132 ) ) ;
#22624 = CARTESIAN_POINT ( 'NONE',  ( -105.3755690713226727, -15.38646221621807619, 15.38646221621768362 ) ) ;
#22625 = CARTESIAN_POINT ( 'NONE',  ( 199.0244464070843833, -3.263486543644114946, 19.73887645897787735 ) ) ;
#22626 = CARTESIAN_POINT ( 'NONE',  ( -56.48582580120558561, -1.205267837095813407E-13, 30.84685318188644132 ) ) ;
#22627 = CARTESIAN_POINT ( 'NONE',  ( 151.7948205124836534, 40.00000000000002842, 6.767089262349174739 ) ) ;
#22628 = LINE ( 'NONE', #12497, #7030 ) ;
#22629 = CARTESIAN_POINT ( 'NONE',  ( -259.2033419157646676, 9.517827891722584255, -0.000000000000000000 ) ) ;
#22630 = CARTESIAN_POINT ( 'NONE',  ( 130.8568914410475088, -5.949712681206664300, -40.00000000000002132 ) ) ;
#22631 = CARTESIAN_POINT ( 'NONE',  ( -208.1127848780264742, 17.67593391476624021, 38.89260858015742883 ) ) ;
#22632 = CARTESIAN_POINT ( 'NONE',  ( -208.1127848780265026, 1.189126717069624012E-13, -15.00245453012669472 ) ) ;
#22633 = CARTESIAN_POINT ( 'NONE',  ( -626.9846540392142060, 28.28427124746186294, -34.99999999999999289 ) ) ;
#22634 = CARTESIAN_POINT ( 'NONE',  ( -208.1127848780264742, 40.00000000000055422, -55.00245453014380814 ) ) ;
#22635 = CARTESIAN_POINT ( 'NONE',  ( -198.0356074513804572, -2.321818583541004323E-13, 55.37879056873073580 ) ) ;
#22636 = CARTESIAN_POINT ( 'NONE',  ( 199.0261966595921592, -11.26051109717869458, 16.53566845662597729 ) ) ;
#22637 = CARTESIAN_POINT ( 'NONE',  ( -138.9613193425335282, -29.42718875726419014, -10.11110876495210675 ) ) ;
#22638 = FACE_OUTER_BOUND ( 'NONE', #23967, .T. ) ;
#22639 = CARTESIAN_POINT ( 'NONE',  ( -100.7734535825088500, -40.53558337403669753, -16.03295912088728770 ) ) ;
#22640 = ORIENTED_EDGE ( 'NONE', *, *, #18344, .T. ) ;
#22641 = CARTESIAN_POINT ( 'NONE',  ( 163.1118516004056573, -19.27778845538787422, 19.27778845538743724 ) ) ;
#22642 = CARTESIAN_POINT ( 'NONE',  ( -678.9461782662789346, 90.00000000000000000, -29.99999999999836220 ) ) ;
#22643 = CARTESIAN_POINT ( 'NONE',  ( -259.2033419157646676, -30.48217210827744239, -2.449293598294708485E-15 ) ) ;
#22644 = ADVANCED_FACE ( 'NONE', ( #9682 ), #1976, .T. ) ;
#22645 = CARTESIAN_POINT ( 'NONE',  ( -114.5523123854248553, 19.58652998792704736, -9.959192389756811536 ) ) ;
#22646 = CARTESIAN_POINT ( 'NONE',  ( -198.0356074513804572, 15.37879056873067007, 0.000000000000000000 ) ) ;
#22647 = ORIENTED_EDGE ( 'NONE', *, *, #16786, .F. ) ;
#22648 = EDGE_LOOP ( 'NONE', ( #15711, #3325, #4858, #23926, #1859, #1722, #19979, #3821, #13939 ) ) ;
#22649 = DIRECTION ( 'NONE',  ( 0.000000000000000000, 1.000000000000000000, 0.000000000000000000 ) ) ;
#22650 = CARTESIAN_POINT ( 'NONE',  ( -88.37877758184959021, 8.575405934490602178, -19.92653024479352908 ) ) ;
#22651 = CARTESIAN_POINT ( 'NONE',  ( 11.38508063393684466, 24.83994849155569540, 44.88728980639523769 ) ) ;
#22652 = ADVANCED_FACE ( 'NONE', ( #8078 ), #18787, .T. ) ;
#22653 = VERTEX_POINT ( 'NONE', #8449 ) ;
#22654 = VERTEX_POINT ( 'NONE', #345 ) ;
#22655 = CARTESIAN_POINT ( 'NONE',  ( -192.9588430854690273, -18.05360324515454096, 38.51493924976936967 ) ) ;
#22656 = CARTESIAN_POINT ( 'NONE',  ( 199.0202851408366485, -18.72068532052425383, -7.046142524300833543 ) ) ;
#22657 = CARTESIAN_POINT ( 'NONE',  ( -716.9846540392142060, -52.49999999999972999, -82.49999999999998579 ) ) ;
#22658 = EDGE_CURVE ( 'NONE', #25214, #17033, #5917, .T. ) ;
#22659 = EDGE_CURVE ( 'NONE', #4726, #8524, #7355, .T. ) ;
#22660 = CARTESIAN_POINT ( 'NONE',  ( -192.9588430854689989, 10.23066800230742679, 10.23066800230749607 ) ) ;
#22661 = CARTESIAN_POINT ( 'NONE',  ( -208.1127848780264742, 38.89260858015732936, -17.67593391476642140 ) ) ;
#22662 = CARTESIAN_POINT ( 'NONE',  ( -199.9999999999997726, -24.82633483071077762, 44.86878812508861358 ) ) ;
#22663 = DIRECTION ( 'NONE',  ( 1.000000000000000000, 0.000000000000000000, 0.000000000000000000 ) ) ;
#22664 = CARTESIAN_POINT ( 'NONE',  ( 184.8905102610680444, 39.99999999999983658, 20.92133201514485563 ) ) ;
#22665 = CARTESIAN_POINT ( 'NONE',  ( -162.0762913951020892, -1.202636532414034422E-14, -1.694272876828323948 ) ) ;
#22666 = CARTESIAN_POINT ( 'NONE',  ( -626.9846540392140923, 26.45751311064577749, 30.00000000000005329 ) ) ;
#22667 = DIRECTION ( 'NONE',  ( -1.000000000000000000, -0.000000000000000000, -0.000000000000000000 ) ) ;
#22668 = CARTESIAN_POINT ( 'NONE',  ( 199.0054653064281922, 16.25946365448332998, -11.63817148238572940 ) ) ;
#22669 = CARTESIAN_POINT ( 'NONE',  ( -187.8778500559390636, 17.82355023088775070, 43.02985669704477090 ) ) ;
#22670 = CARTESIAN_POINT ( 'NONE',  ( 0.2972598230769976091, -10.13633138497465147, -10.13633138497482733 ) ) ;
#22671 = CARTESIAN_POINT ( 'NONE',  ( -105.4741150117365009, 19.60045294981777531, -8.366608964619008049 ) ) ;
#22672 = CARTESIAN_POINT ( 'NONE',  ( 130.8568914410475088, 24.07718906446891793, 32.49135343045489321 ) ) ;
#22673 = CARTESIAN_POINT ( 'NONE',  ( -575.0231298121445889, 90.00000000000000000, 29.99999999999825206 ) ) ;
#22674 = CARTESIAN_POINT ( 'NONE',  ( -238.4067589809705794, -28.96627169325303797, -28.96627169325349627 ) ) ;
#22675 = CARTESIAN_POINT ( 'NONE',  ( -661.4640049366287258, 44.59621196335826454, 6.044506261930657764 ) ) ;
#22676 = CARTESIAN_POINT ( 'NONE',  ( -86.96347745069645896, 21.75974354311648895, -0.000000000000000000 ) ) ;
#22677 = PLANE ( 'NONE',  #13417 ) ;
#22678 = CARTESIAN_POINT ( 'NONE',  ( -105.3755690713226869, 21.75974354311648540, -0.000000000000000000 ) ) ;
#22679 = CARTESIAN_POINT ( 'NONE',  ( -599.8456638329612360, 39.19767421272204189, -22.10842335695227590 ) ) ;
#22680 = CARTESIAN_POINT ( 'NONE',  ( 170.2234770963711128, 40.00000000000021316, -15.44714144992773797 ) ) ;
#22681 = CARTESIAN_POINT ( 'NONE',  ( 199.0138805921241953, -11.07098026833737414, -16.66790957460414901 ) ) ;
#22682 = CARTESIAN_POINT ( 'NONE',  ( 155.1206158682454657, -11.51471166709265503, 27.79897307351014746 ) ) ;
#22683 = ORIENTED_EDGE ( 'NONE', *, *, #7052, .F. ) ;
#22684 = ORIENTED_EDGE ( 'NONE', *, *, #16318, .F. ) ;
#22685 = CARTESIAN_POINT ( 'NONE',  ( 184.8905102610680444, -20.92133201514440799, 0.000000000000000000 ) ) ;
#22686 = ADVANCED_FACE ( 'NONE', ( #24698 ), #13864, .T. ) ;
#22687 = CARTESIAN_POINT ( 'NONE',  ( 164.1122551457367251, 10.10009781492405523, 24.38379312608499561 ) ) ;
#22688 = CARTESIAN_POINT ( 'NONE',  ( 0.2972598230769959993, 38.42060263243713081, -38.42060263243619289 ) ) ;
#22689 = CARTESIAN_POINT ( 'NONE',  ( -114.7538884075660235, -21.97380054625780232, -2.777513412063746578 ) ) ;
#22690 = CARTESIAN_POINT ( 'NONE',  ( -193.0908841288064934, -44.14257353178373222, -24.29092413197459521 ) ) ;
#22691 = CARTESIAN_POINT ( 'NONE',  ( -114.4364955367322949, 8.644468109217019247, 20.04994829327305794 ) ) ;
#22692 = CARTESIAN_POINT ( 'NONE',  ( 199.9999999999999716, -5.826418053481885906, -18.09029720167993105 ) ) ;
#22693 = CARTESIAN_POINT ( 'NONE',  ( 163.1118516004056573, -19.27778845539181063, -37.29075403953176959 ) ) ;
#22694 = DIRECTION ( 'NONE',  ( 0.000000000000000000, 0.000000000000000000, 1.000000000000000000 ) ) ;
#22695 = CARTESIAN_POINT ( 'NONE',  ( -109.1264249741459622, 13.72187187123908814, -33.12752917269256159 ) ) ;
#22696 = CARTESIAN_POINT ( 'NONE',  ( 170.2234770963711128, 39.99999999999980105, 24.55285855007229401 ) ) ;
#22697 = CARTESIAN_POINT ( 'NONE',  ( -91.56559293963836410, 16.03295912088692177, 16.03295912088721664 ) ) ;
#22698 = CARTESIAN_POINT ( 'NONE',  ( 146.6084372240433993, 34.62501878078308692, 0.000000000000000000 ) ) ;
#22699 = CARTESIAN_POINT ( 'NONE',  ( 170.2234770963711128, -17.36149277827010096, 17.36149277826970660 ) ) ;
#22700 = CARTESIAN_POINT ( 'NONE',  ( 130.8568914410475372, 24.07718906447243867, -24.07718906447216156 ) ) ;
#22701 = CARTESIAN_POINT ( 'NONE',  ( 199.0082414334414125, 19.98886982631870524, -0.5857068698800287354 ) ) ;
#22703 = CARTESIAN_POINT ( 'NONE',  ( 170.2234770963711128, -40.00000000000004263, 15.44714144992801685 ) ) ;
#22702 = CARTESIAN_POINT ( 'NONE',  ( 151.7948205124836250, 4.785054706301759886, -4.785054706301612448 ) ) ;
#22704 = CARTESIAN_POINT ( 'NONE',  ( -56.48582580120559982, 21.81201906317729922, 34.75652343174635917 ) ) ;
#22705 = CARTESIAN_POINT ( 'NONE',  ( 19.94008347559388028, 47.92933869853938234, -13.96811062196751863 ) ) ;
#22706 = CARTESIAN_POINT ( 'NONE',  ( -105.3755690713226585, -21.75974354311652448, -40.00000000000002132 ) ) ;
#22707 = CARTESIAN_POINT ( 'NONE',  ( -56.48582580120559271, -6.472252184284187138, -6.472252184284199572 ) ) ;
#22708 = CARTESIAN_POINT ( 'NONE',  ( -162.0762913951021176, 41.69427287672986182, 40.00000000000002132 ) ) ;
#22709 = CARTESIAN_POINT ( 'NONE',  ( -7.233308327735402443, -42.27575367454439714, 17.51119053154051031 ) ) ;
#22710 = CARTESIAN_POINT ( 'NONE',  ( -208.1127848780264742, 55.00245453014418473, 40.00000000000002132 ) ) ;
#22711 = VERTEX_POINT ( 'NONE', #6785 ) ;
#22712 = CARTESIAN_POINT ( 'NONE',  ( 21.98945382326336428, 23.63684424402695328, -43.25809532770859533 ) ) ;
#22713 = CARTESIAN_POINT ( 'NONE',  ( -213.1075012329537230, -18.58567234101155208, 37.98287015391234434 ) ) ;
#22714 = DIRECTION ( 'NONE',  ( 0.000000000000000000, 1.000000000000000000, 0.000000000000000000 ) ) ;
#22715 = CARTESIAN_POINT ( 'NONE',  ( 6.202588567995411140, 14.15973318134927439, -49.19971320597417730 ) ) ;
#22716 = CARTESIAN_POINT ( 'NONE',  ( 200.0000000000000568, -10.82911035642265141, 15.62521814345774196 ) ) ;
#22717 = CARTESIAN_POINT ( 'NONE',  ( -192.9588430854689989, 10.23066800230756712, -10.23066800230735396 ) ) ;
#22718 = CARTESIAN_POINT ( 'NONE',  ( -77.62874474886855580, -21.73921449502670811, 3.805079090745403736 ) ) ;
#22719 = CARTESIAN_POINT ( 'NONE',  ( 199.9999999999998863, 13.43021917686961331, -13.43983678748323918 ) ) ;
#22720 = CARTESIAN_POINT ( 'NONE',  ( -188.6890294954570493, -23.53287096354458185, 43.11788624869836184 ) ) ;
#22721 = CARTESIAN_POINT ( 'NONE',  ( 192.4448373802101173, -39.99999999999977973, -19.99999999996102673 ) ) ;
#22722 = CARTESIAN_POINT ( 'NONE',  ( -56.48582580120559271, -6.472252184284276844, 6.472252184284108978 ) ) ;
#22723 = CARTESIAN_POINT ( 'NONE',  ( 184.8905102610680444, 20.92133201514447194, 40.00000000000002132 ) ) ;
#22725 = CARTESIAN_POINT ( 'NONE',  ( 4.995406935893286438, 67.35176059880245703, -10.78321810387767066 ) ) ;
#22724 = CARTESIAN_POINT ( 'NONE',  ( -190.0144721488044581, 13.91469502168346040, -47.57279682960905376 ) ) ;
#22726 = CARTESIAN_POINT ( 'NONE',  ( 200.0000000000000000, 14.14213562373041455, 42.42640687119311593 ) ) ;
#22727 = ADVANCED_FACE ( 'NONE', ( #813 ), #4941, .F. ) ;
#22728 = CARTESIAN_POINT ( 'NONE',  ( 192.4448373802101173, -19.99999999996056843, -40.00000000000002132 ) ) ;
#22729 = CARTESIAN_POINT ( 'NONE',  ( -105.3755690713226585, 18.24025645688349684, 40.00000000000002132 ) ) ;
#22730 = CARTESIAN_POINT ( 'NONE',  ( -162.0762913951021176, -40.00000000000003553, -1.694272876828743168 ) ) ;
#22731 = CARTESIAN_POINT ( 'NONE',  ( 57.59792236341147031, 26.56190807104693619, -30.00663442387692115 ) ) ;
#22732 = CARTESIAN_POINT ( 'NONE',  ( 146.6084372240433993, -3.800685668858596156, -3.800685668858692967 ) ) ;
#22733 = CARTESIAN_POINT ( 'NONE',  ( -105.3755690713226727, 15.38646221621793231, -15.38646221621779020 ) ) ;
#22734 = ORIENTED_EDGE ( 'NONE', *, *, #12425, .T. ) ;
#22735 = CARTESIAN_POINT ( 'NONE',  ( -86.96347745069644475, -43.67073346367983788, 12.89780903124397149 ) ) ;
#22736 = CARTESIAN_POINT ( 'NONE',  ( -105.4732637872234449, 8.153770687239065396, 19.68494377761417979 ) ) ;
#22737 = CONTEXT_DEPENDENT_SHAPE_REPRESENTATION ( #26190, #24650 ) ;
#22738 = CARTESIAN_POINT ( 'NONE',  ( 192.4448373802100889, -14.14213562370313682, 14.14213562370301958 ) ) ;
#22739 = CARTESIAN_POINT ( 'NONE',  ( -3.336279363873598580, -43.33179396957120133, -17.94861674415379937 ) ) ;
#22740 = ADVANCED_FACE ( 'NONE', ( #415 ), #20922, .T. ) ;
#22741 = ORIENTED_EDGE ( 'NONE', *, *, #26271, .F. ) ;
#22742 = CARTESIAN_POINT ( 'NONE',  ( -100.7734535825088358, -22.67402823373193499, 0.000000000000000000 ) ) ;
#22743 = CARTESIAN_POINT ( 'NONE',  ( -199.9999999999997726, -24.82633483071077762, 44.86878812508861358 ) ) ;
#22745 = ORIENTED_EDGE ( 'NONE', *, *, #11104, .T. ) ;
#22744 = EDGE_CURVE ( 'NONE', #4688, #12615, #19989, .T. ) ;
#22746 =( BOUNDED_SURFACE ( )  B_SPLINE_SURFACE ( 3, 2, ( 
 ( #5637, #21366, #5258 ),
 ( #23729, #19738, #11616 ),
 ( #2060, #16010, #54 ),
 ( #16143, #24277, #16545 ),
 ( #22014, #2316, #14282 ),
 ( #2192, #18407, #6046 ),
 ( #22419, #10424, #26146 ),
 ( #3785, #12025, #18542 ),
 ( #8165, #14151, #20546 ),
 ( #8289, #24544, #11887 ),
 ( #18001, #5773, #3927 ),
 ( #10029, #22283, #20008 ),
 ( #4057, #18139, #12159 ),
 ( #1793, #26287, #7890 ),
 ( #10300, #20145, #182 ),
 ( #24406, #20281, #16416 ),
 ( #14417, #24136, #8026 ),
 ( #6299, #5908, #10166 ) ),
 .UNSPECIFIED., .F., .F., .T. ) 
 B_SPLINE_SURFACE_WITH_KNOTS ( ( 4, 2, 2, 2, 2, 2, 2, 2, 4 ),
 ( 3, 3 ),
 ( 0.04072677052481911419, 0.04791560376915927899, 0.04971281208024432019, 0.05151002039132936139, 0.05510443701349943685, 0.06229327025783959471, 0.06409047856892463590, 0.06588768688000967710, 0.06948210350217975950 ),
 ( 0.000000000000000000, 1.000000000000000000 ),
 .UNSPECIFIED. ) 
 GEOMETRIC_REPRESENTATION_ITEM ( )  RATIONAL_B_SPLINE_SURFACE ( (
 ( 1.000000000000000000, 0.9548354691836614672, 1.000000000000000000),
 ( 1.000000000000000000, 0.9525322272685073921, 1.000000000000000000),
 ( 1.000000000000000000, 0.9507090889564540070, 1.000000000000000000),
 ( 1.000000000000000000, 0.9491274412103997138, 1.000000000000000000),
 ( 1.000000000000000000, 0.9488458704368275543, 1.000000000000000000),
 ( 1.000000000000000000, 0.9483593260462360730, 1.000000000000000000),
 ( 1.000000000000000000, 0.9481536719786518574, 1.000000000000000000),
 ( 1.000000000000000000, 0.9476504944683689091, 1.000000000000000000),
 ( 1.000000000000000000, 0.9474672089150538712, 1.000000000000000000),
 ( 1.000000000000000000, 0.9473824172973602797, 1.000000000000000000),
 ( 1.000000000000000000, 0.9479352605727494607, 1.000000000000000000),
 ( 1.000000000000000000, 0.9493585436777139952, 1.000000000000000000),
 ( 1.000000000000000000, 0.9496800152430581177, 1.000000000000000000),
 ( 1.000000000000000000, 0.9503966249792042964, 1.000000000000000000),
 ( 1.000000000000000000, 0.9507930042074207444, 1.000000000000000000),
 ( 1.000000000000000000, 0.9520783074840074578, 1.000000000000000000),
 ( 1.000000000000000000, 0.9530652555250912483, 1.000000000000000000),
 ( 1.000000000000000000, 0.9541700777564556812, 1.000000000000000000) ) ) 
 REPRESENTATION_ITEM ( '' )  SURFACE ( )  );
#22747 = VECTOR ( 'NONE', #6557, 1000.000000000000000 ) ;
#22748 = CARTESIAN_POINT ( 'NONE',  ( 199.9999999999998295, 14.29413690760092592, -12.53266873553815053 ) ) ;
#22749 = CARTESIAN_POINT ( 'NONE',  ( 12.01361943528961085, 14.17591515420136972, -49.30661675909291830 ) ) ;
#22750 = CARTESIAN_POINT ( 'NONE',  ( -56.48582580120558561, -1.205267837095813407E-13, 30.84685318188644132 ) ) ;
#22751 = CARTESIAN_POINT ( 'NONE',  ( -86.96347745069644475, 18.24025645688350750, 40.00000000000002132 ) ) ;
#22752 = CARTESIAN_POINT ( 'NONE',  ( -91.56559293963834989, -16.03295912088728414, 16.03295912088688269 ) ) ;
#22753 = CARTESIAN_POINT ( 'NONE',  ( 199.0147602753770855, 15.66021538362855381, 12.44349737331557648 ) ) ;
#22754 = VECTOR ( 'NONE', #3242, 1000.000000000000000 ) ;
#22755 = AXIS2_PLACEMENT_3D ( 'NONE', #25766, #19376, #19123 ) ;
#22756 = CARTESIAN_POINT ( 'NONE',  ( -56.48582580120558561, -50.09629031063971638, 6.472252184283745713 ) ) ;
#22757 = CARTESIAN_POINT ( 'NONE',  ( 199.9999999999999432, -3.553951640073651008E-14, 19.99999999999992539 ) ) ;
#22758 = CARTESIAN_POINT ( 'NONE',  ( -56.48582580120560692, 40.00000000000004263, -9.153146818113443217 ) ) ;
#22759 = FACE_OUTER_BOUND ( 'NONE', #15585, .T. ) ;
#22760 = FACE_BOUND ( 'NONE', #16284, .T. ) ;
#22761 = CARTESIAN_POINT ( 'NONE',  ( 91.82158438592159655, -22.79471317813468545, -40.00000000000002132 ) ) ;
#22762 = CARTESIAN_POINT ( 'NONE',  ( 146.6084372240433709, 24.48358557860311180, 32.08495691632071356 ) ) ;
#22763 = CARTESIAN_POINT ( 'NONE',  ( -716.9846540392142060, 66.50000000000009948, 71.50000000000005684 ) ) ;
#22764 = CARTESIAN_POINT ( 'NONE',  ( -110.1003821002792620, 15.15067674040053092, -13.36729751623248497 ) ) ;
#22765 = CARTESIAN_POINT ( 'NONE',  ( -259.2033419157646676, 40.00000000000029843, -30.48217210827696988 ) ) ;
#22766 = CARTESIAN_POINT ( 'NONE',  ( 57.59792236341149163, -40.00000000000014211, 37.56421063658172699 ) ) ;
#22767 = CARTESIAN_POINT ( 'NONE',  ( 199.0259813356335883, -9.719824439858887999, 17.48565896982476175 ) ) ;
#22768 = CARTESIAN_POINT ( 'NONE',  ( 73.43468099484965705, -12.96803874020848468, 26.88834960806370233 ) ) ;
#22769 = DIRECTION ( 'NONE',  ( 0.000000000000000000, -1.000000000000000000, 0.000000000000000000 ) ) ;
#22770 = CARTESIAN_POINT ( 'NONE',  ( -91.56559293963834989, -12.25131212657492874, 12.25131212657477953 ) ) ;
#22771 = ORIENTED_EDGE ( 'NONE', *, *, #4790, .F. ) ;
#22772 = CARTESIAN_POINT ( 'NONE',  ( -188.2995950289363805, 23.44932284466059969, -43.00522595870931752 ) ) ;
#22773 = CARTESIAN_POINT ( 'NONE',  ( 137.0939645874030361, 30.33050608226201206, -12.56330697291247844 ) ) ;
#22774 = CARTESIAN_POINT ( 'NONE',  ( 57.59792236341147031, 2.435789363418170872, -40.00000000000002132 ) ) ;
#22775 = CARTESIAN_POINT ( 'NONE',  ( -86.86493150571121191, -19.77569912839188149, -7.943527260495856446 ) ) ;
#22776 = CARTESIAN_POINT ( 'NONE',  ( -716.9846540392142060, 52.50000000000007816, -52.49999999999999289 ) ) ;
#22777 = SHAPE_REPRESENTATION_RELATIONSHIP ( 'NONE' , 'NONE' ,  #14572, #16278 ) ;
#22778 = ORIENTED_EDGE ( 'NONE', *, *, #24745, .T. ) ;
#22779 = AXIS2_PLACEMENT_3D ( 'NONE', #8367, #4761, #10871 ) ;
#22780 = ORIENTED_EDGE ( 'NONE', *, *, #20881, .T. ) ;
#22781 = AXIS2_PLACEMENT_3D ( 'NONE', #11850, #13976, #1489 ) ;
#22782 = CARTESIAN_POINT ( 'NONE',  ( 199.9999999999999716, -7.851686492350575364, 17.31563863434756101 ) ) ;
#22783 = CARTESIAN_POINT ( 'NONE',  ( -86.86493150571128297, 7.943527260495892861, -19.77569912839186372 ) ) ;
#22784 = CARTESIAN_POINT ( 'NONE',  ( 23.37583784646053786, 13.80085822091002790, 46.80752016581961072 ) ) ;
#22785 = ORIENTED_EDGE ( 'NONE', *, *, #24291, .F. ) ;
#22786 = ORIENTED_EDGE ( 'NONE', *, *, #14776, .F. ) ;
#22787 = CARTESIAN_POINT ( 'NONE',  ( 170.2234770963711128, -17.36149277826985937, -17.36149277826995174 ) ) ;
#22788 = CARTESIAN_POINT ( 'NONE',  ( 199.0258314272957421, -17.94308652430182605, 8.851303907023687856 ) ) ;
#22789 = CARTESIAN_POINT ( 'NONE',  ( -105.2276019244893916, -17.02339403573614263, -13.16689311108276783 ) ) ;
#22790 = AXIS2_PLACEMENT_3D ( 'NONE', #1310, #17276, #15653 ) ;
#22791 = CARTESIAN_POINT ( 'NONE',  ( -86.96347745069644475, -15.38646221621796073, 41.18208027870593924 ) ) ;
#22792 = DIRECTION ( 'NONE',  ( 0.000000000000000000, 0.000000000000000000, 1.000000000000000000 ) ) ;
#22793 = CARTESIAN_POINT ( 'NONE',  ( -109.0492076899303555, 7.884024499252893476E-13, -35.99236577015783212 ) ) ;
#22794 = EDGE_CURVE ( 'NONE', #24345, #8862, #16106, .T. ) ;
#22795 = DIRECTION ( 'NONE',  ( 1.000000000000000000, 1.836970198721030181E-16, -0.000000000000000000 ) ) ;
#22796 = CARTESIAN_POINT ( 'NONE',  ( -135.8532207217289738, 3.005970985514575011E-13, -30.84685318188645553 ) ) ;
#22797 = CARTESIAN_POINT ( 'NONE',  ( 57.59792236341146321, 40.00000000000000711, 2.435789363418579434 ) ) ;
#22798 = CARTESIAN_POINT ( 'NONE',  ( 180.0000000000000000, -61.50000000000001421, -66.50000000000005684 ) ) ;
#22799 = DIRECTION ( 'NONE',  ( 0.000000000000000000, -1.000000000000000000, 0.000000000000000000 ) ) ;
#22800 = CARTESIAN_POINT ( 'NONE',  ( 199.0068982850735608, 19.44025291972790370, -4.682182605709538592 ) ) ;
#22801 = CARTESIAN_POINT ( 'NONE',  ( -173.7925187076908458, 12.78856575072571644, 41.93431653926056413 ) ) ;
#22802 = CARTESIAN_POINT ( 'NONE',  ( 200.0000000000000000, -42.42640687119290988, 14.14213562373064903 ) ) ;
#22803 = CARTESIAN_POINT ( 'NONE',  ( -97.72675010090438263, 8.987772175319268086, 20.56394680065916347 ) ) ;
#22804 = CARTESIAN_POINT ( 'NONE',  ( 0.2972598230770048811, -10.13633138497510089, 66.70487387989852834 ) ) ;
#22805 = CARTESIAN_POINT ( 'NONE',  ( -210.0000000000000284, 75.52305771588336825, -68.47933392563552957 ) ) ;
#22806 = CARTESIAN_POINT ( 'NONE',  ( -86.96347745069645896, 43.67073346367988762, -12.89780903124366418 ) ) ;
#22807 = CARTESIAN_POINT ( 'NONE',  ( -641.7033821489691263, 31.87133642205515471, 31.77436929086892903 ) ) ;
#22808 = CARTESIAN_POINT ( 'NONE',  ( -56.48582580120559982, 9.153146818113574668, 40.00000000000002132 ) ) ;
#22809 = VECTOR ( 'NONE', #14902, 1000.000000000000114 ) ;
#22810 = CARTESIAN_POINT ( 'NONE',  ( 146.6084372240433709, 3.800685668858042821, 52.76785682606522698 ) ) ;
#22811 = CARTESIAN_POINT ( 'NONE',  ( 91.82158438592158234, 17.20528682183301683, 0.000000000000000000 ) ) ;
#22812 = CARTESIAN_POINT ( 'NONE',  ( -593.2054431927236919, 44.05607902751195581, 9.473706874029589997 ) ) ;
#22813 = CARTESIAN_POINT ( 'NONE',  ( 146.6084372240433709, -39.99999999999993605, -5.374981219217395356 ) ) ;
#22814 = CARTESIAN_POINT ( 'NONE',  ( 199.0116092925779014, -7.071658929006641614, -18.70726711289027833 ) ) ;
#22815 = CARTESIAN_POINT ( 'NONE',  ( 158.3379117892986869, -10.98149362779657601, 26.51167085133944923 ) ) ;
#22816 = EDGE_LOOP ( 'NONE', ( #11487, #5116, #13776, #15635 ) ) ;
#22817 = ORIENTED_EDGE ( 'NONE', *, *, #16786, .T. ) ;
#22818 = ORIENTED_EDGE ( 'NONE', *, *, #21816, .T. ) ;
#22819 = CARTESIAN_POINT ( 'NONE',  ( -162.0762913951021176, 41.69427287672986182, 40.00000000000002132 ) ) ;
#22820 = CARTESIAN_POINT ( 'NONE',  ( 149.5797498300189261, 12.18602109748300855, 29.41965740490887526 ) ) ;
#22821 = CARTESIAN_POINT ( 'NONE',  ( -198.0356074513804572, 67.44298959250878056, -10.87444709758402261 ) ) ;
#22822 = CARTESIAN_POINT ( 'NONE',  ( -114.7755410848894968, -22.09261867841506799, 1.384971738882752268 ) ) ;
#22823 = AXIS2_PLACEMENT_3D ( 'NONE', #15852, #10018, #21859 ) ;
#22824 = EDGE_CURVE ( 'NONE', #6964, #16641, #17911, .T. ) ;
#22825 = CARTESIAN_POINT ( 'NONE',  ( -126.6834156231701769, -9.107266674874638923, 24.89646324320183979 ) ) ;
#22826 = CARTESIAN_POINT ( 'NONE',  ( -86.95488169845610571, 6.698970622310091549, -20.33891803571749435 ) ) ;
#22827 = CARTESIAN_POINT ( 'NONE',  ( 200.0000000000001137, 2.164978928433492822, -18.87806096587463855 ) ) ;
#22828 = LINE ( 'NONE', #4605, #6225 ) ;
#22829 = CARTESIAN_POINT ( 'NONE',  ( 200.0000000000000000, -14.14213562373046784, -42.42640687119298804 ) ) ;
#22830 = CARTESIAN_POINT ( 'NONE',  ( 4.995406935893293543, -10.78321810388990265, -10.78321810389009272 ) ) ;
#22831 = CARTESIAN_POINT ( 'NONE',  ( -211.2619052429883482, 0.000000000000000000, 0.000000000000000000 ) ) ;
#22832 = CARTESIAN_POINT ( 'NONE',  ( 146.6084372240433709, 39.99999999999968026, 34.62501878078347772 ) ) ;
#22833 = DIRECTION ( 'NONE',  ( 0.2259624731720737134, 0.9741360072997814479, 0.000000000000000000 ) ) ;
#22834 = CARTESIAN_POINT ( 'NONE',  ( -220.0000000000000284, 71.50000000000002842, -66.50000000000005684 ) ) ;
#22835 = CARTESIAN_POINT ( 'NONE',  ( 136.1360204305621266, -24.77266263493116583, -24.77266263493127951 ) ) ;
#22836 = EDGE_CURVE ( 'NONE', #25302, #17336, #18661, .T. ) ;
#22837 = EDGE_CURVE ( 'NONE', #6926, #7299, #12454, .T. ) ;
#22838 = CARTESIAN_POINT ( 'NONE',  ( -259.2033419157646676, -21.55415060305854524, 21.55415060305827524 ) ) ;
#22839 = CARTESIAN_POINT ( 'NONE',  ( -213.1075012329537230, -13.71589010951915810, 0.000000000000000000 ) ) ;
#22841 = CARTESIAN_POINT ( 'NONE',  ( 14.38125909742180930, 39.99999999999982947, 55.17850393971022527 ) ) ;
#22840 = CARTESIAN_POINT ( 'NONE',  ( 136.1360204305621551, -53.05693388239309627, -3.511608612531332163 ) ) ;
#22842 = CARTESIAN_POINT ( 'NONE',  ( 22.72189371635671051, 43.05215026464217232, -23.48424859981733448 ) ) ;
#22843 = CARTESIAN_POINT ( 'NONE',  ( 192.4448373802101173, -20.00000000003938538, -40.00000000000002132 ) ) ;
#22844 = CARTESIAN_POINT ( 'NONE',  ( -135.8532207217289738, -6.472252184284287502, 50.09629031063965243 ) ) ;
#22845 = CARTESIAN_POINT ( 'NONE',  ( -86.96347745069644475, 18.24025645688350750, 40.00000000000002132 ) ) ;
#22846 = CARTESIAN_POINT ( 'NONE',  ( -4.439300432583282330, -46.85201324744756590, 13.79990882516902317 ) ) ;
#22847 = CARTESIAN_POINT ( 'NONE',  ( 146.6084372240433709, 5.374981219216996564, 40.00000000000002132 ) ) ;
#22848 = ORIENTED_EDGE ( 'NONE', *, *, #21822, .T. ) ;
#22849 = CARTESIAN_POINT ( 'NONE',  ( 98.29820294268191105, -7.653668647302824368, -18.47759065022797031 ) ) ;
#22850 = CARTESIAN_POINT ( 'NONE',  ( -575.0231298121466352, 90.00000000000000000, -30.00000000000202505 ) ) ;
#22851 = CARTESIAN_POINT ( 'NONE',  ( -5.296937277128574095, -17.72975434250267313, 42.80341339121885369 ) ) ;
#22852 = CARTESIAN_POINT ( 'NONE',  ( -4.810655158401165643, 17.78437748361197990, -42.93528531927893255 ) ) ;
#22853 = CARTESIAN_POINT ( 'NONE',  ( 199.0202851408366485, -18.72068532052425383, -7.046142524300833543 ) ) ;
#22854 = CARTESIAN_POINT ( 'NONE',  ( -105.3755690713226727, -15.38646221621807619, 15.38646221621768362 ) ) ;
#22855 = CARTESIAN_POINT ( 'NONE',  ( -190.0000000000000000, 66.50000000000009948, 66.50000000000005684 ) ) ;
#22856 = CARTESIAN_POINT ( 'NONE',  ( -87.10560006382534937, 2.727320883003452767, 21.31071338414146865 ) ) ;
#22857 = CARTESIAN_POINT ( 'NONE',  ( -188.2871287166303773, -13.82723289751392137, 46.98614659774630553 ) ) ;
#22858 = CARTESIAN_POINT ( 'NONE',  ( 170.2234770963711128, 17.36149277826980253, 17.36149277827007253 ) ) ;
#22859 = CARTESIAN_POINT ( 'NONE',  ( 163.1118516004056573, -47.56205970284945295, -9.006482792074823607 ) ) ;
#22860 = CARTESIAN_POINT ( 'NONE',  ( -192.9588430854689989, -10.23066800230742501, -10.23066800230756712 ) ) ;
#22862 = CARTESIAN_POINT ( 'NONE',  ( 192.4448373802100889, 14.14213562370330379, -14.14213562370292365 ) ) ;
#22861 = CARTESIAN_POINT ( 'NONE',  ( 192.4448373802100889, 14.14213562375873678, 14.14213562375894817 ) ) ;
#22863 = CARTESIAN_POINT ( 'NONE',  ( -100.7734535825088358, -16.03295912088728770, 16.03295912088687913 ) ) ;
#22864 = CARTESIAN_POINT ( 'NONE',  ( 57.59792236341148453, -37.56421063658185489, -40.00000000000002132 ) ) ;
#22865 = CARTESIAN_POINT ( 'NONE',  ( -56.48582580120559271, -9.153146818113595984, 0.000000000000000000 ) ) ;
#22866 = CARTESIAN_POINT ( 'NONE',  ( -259.2033419157646676, -1.473088368616265084E-13, 9.517827891722632216 ) ) ;
#22867 = CARTESIAN_POINT ( 'NONE',  ( -198.0356074513804572, 39.15871834505912119, -17.40982414986464377 ) ) ;
#22868 = CARTESIAN_POINT ( 'NONE',  ( -99.31267923334560521, 20.62886818714807191, -8.544756979537151409 ) ) ;
#22869 = CARTESIAN_POINT ( 'NONE',  ( 91.82158438592159655, -16.11829626346125011, -16.11829626346154853 ) ) ;
#22870 = CARTESIAN_POINT ( 'NONE',  ( 192.4448373802101173, 42.42640687122070631, 14.14213562370331623 ) ) ;
#22871 = EDGE_LOOP ( 'NONE', ( #14083, #18679 ) ) ;
#22872 = CARTESIAN_POINT ( 'NONE',  ( -238.4067589809705794, 57.25054294077225592, 0.6820004458485544596 ) ) ;
#22873 = CARTESIAN_POINT ( 'NONE',  ( -188.7701102708080612, -13.85300071690466872, -47.15821026576311681 ) ) ;
#22874 = CARTESIAN_POINT ( 'NONE',  ( -213.1075012329537230, 18.58567234101121102, 37.98287015391247223 ) ) ;
#22875 = CARTESIAN_POINT ( 'NONE',  ( -4.076660308449338466, -42.99426297939334773, -23.44206949513785787 ) ) ;
#22876 = EDGE_LOOP ( 'NONE', ( #24068, #4594 ) ) ;
#22877 = CARTESIAN_POINT ( 'NONE',  ( -105.2054292635175727, 15.19799821370213522, 15.19799821370241943 ) ) ;
#22878 = CARTESIAN_POINT ( 'NONE',  ( -114.4364955367319823, -8.644468109212290585, -20.04994829327477035 ) ) ;
#22879 = CARTESIAN_POINT ( 'NONE',  ( 200.0000000000003126, 15.08009544811998204, -11.56244146370294779 ) ) ;
#22880 = CARTESIAN_POINT ( 'NONE',  ( 17.76569288431003812, 14.04863394049499981, -48.46476365406677189 ) ) ;
#22881 = CARTESIAN_POINT ( 'NONE',  ( -105.3755690713226727, 18.24025645688350750, 2.449293598294708485E-15 ) ) ;
#22882 = CARTESIAN_POINT ( 'NONE',  ( 163.1118516004056573, -19.27778845538787422, 19.27778845538743724 ) ) ;
#22883 = CARTESIAN_POINT ( 'NONE',  ( 199.0142490642952566, 16.24935999037262846, 11.66321269349018941 ) ) ;
#22884 = CARTESIAN_POINT ( 'NONE',  ( 4.995406935893297984, -39.06748935135205869, 17.50105314357158193 ) ) ;
#22885 = CARTESIAN_POINT ( 'NONE',  ( -100.7734535825088500, 39.99999999999994316, 17.32597176626825686 ) ) ;
#22886 = CARTESIAN_POINT ( 'NONE',  ( -100.7734535825088500, 40.00000000000008527, -22.67402823373177512 ) ) ;
#22887 = CARTESIAN_POINT ( 'NONE',  ( -1.258540240222682849, 47.88180740053044815, -13.96099832920784145 ) ) ;
#22888 = CARTESIAN_POINT ( 'NONE',  ( 170.2234770963711128, -15.44714144992812699, -40.00000000000002132 ) ) ;
#22889 = CARTESIAN_POINT ( 'NONE',  ( -604.2904488564438452, 34.85647621512581651, 19.62648268795706130 ) ) ;
#22890 = CARTESIAN_POINT ( 'NONE',  ( -198.0356074513804572, -55.37879056871328487, -40.00000000000002132 ) ) ;
#22891 = CARTESIAN_POINT ( 'NONE',  ( -91.56559293963834989, -12.25131212657492874, 12.25131212657477953 ) ) ;
#22892 = FACE_OUTER_BOUND ( 'NONE', #20787, .T. ) ;
#22893 = ADVANCED_FACE ( 'NONE', ( #14847 ), #6415, .T. ) ;
#22894 = CARTESIAN_POINT ( 'NONE',  ( -105.2958943009977446, 11.44501736924781099, -18.12177707671771998 ) ) ;
#22895 = CARTESIAN_POINT ( 'NONE',  ( -162.0762913951021176, 40.00000000000042633, -41.69427287672947102 ) ) ;
#22896 = CARTESIAN_POINT ( 'NONE',  ( -91.56559293963836410, 39.99999999999994316, 17.32597176626825330 ) ) ;
#22897 = CARTESIAN_POINT ( 'NONE',  ( 199.0262910934941942, -12.18938195246538037, 15.86593956234834479 ) ) ;
#22898 = DIRECTION ( 'NONE',  ( -1.000000000000000000, 0.000000000000000000, 0.000000000000000000 ) ) ;
#22899 = CARTESIAN_POINT ( 'NONE',  ( -259.2033419157646676, -6.730120644403663199, 6.730120644403451813 ) ) ;
#22900 = CARTESIAN_POINT ( 'NONE',  ( -238.4067589809705794, -28.96627169325343942, 28.96627169325309126 ) ) ;
#22901 = ORIENTED_EDGE ( 'NONE', *, *, #11242, .T. ) ;
#22903 = CARTESIAN_POINT ( 'NONE',  ( -189.2428623074473819, 23.64699222226093411, -43.27185639470894074 ) ) ;
#22902 = CARTESIAN_POINT ( 'NONE',  ( -91.56559293963836410, 16.03295912088692177, 16.03295912088721664 ) ) ;
#22904 = CARTESIAN_POINT ( 'NONE',  ( 149.5797498300188977, 29.41965740490885750, -12.18602109748323592 ) ) ;
#22905 = CARTESIAN_POINT ( 'NONE',  ( 130.8568914410475088, 34.05028731879790627, -40.00000000000002132 ) ) ;
#22906 = AXIS2_PLACEMENT_3D ( 'NONE', #21319, #16925, #25190 ) ;
#22907 = CARTESIAN_POINT ( 'NONE',  ( -105.2274175719510367, 13.17695787001530761, 17.01505826703009205 ) ) ;
#22908 = CARTESIAN_POINT ( 'NONE',  ( -200.0000000000000000, -60.00000000000011369, 7.960204194457800407E-15 ) ) ;
#22909 = EDGE_LOOP ( 'NONE', ( #6566, #3456, #5701, #22640 ) ) ;
#22910 = ORIENTED_EDGE ( 'NONE', *, *, #4274, .T. ) ;
#22911 = CARTESIAN_POINT ( 'NONE',  ( 23.37394308801977871, -13.80096434448300613, 46.80823611210190904 ) ) ;
#22912 = LINE ( 'NONE', #14911, #3038 ) ;
#22913 = CARTESIAN_POINT ( 'NONE',  ( 23.38399212876434419, 13.80022400692476836, 46.80460545930715455 ) ) ;
#22914 = ORIENTED_EDGE ( 'NONE', *, *, #6480, .T. ) ;
#22915 = EDGE_LOOP ( 'NONE', ( #12624, #22392, #15701, #25750 ) ) ;
#22916 = CARTESIAN_POINT ( 'NONE',  ( 146.6084372240433709, -52.76785682606516303, 3.800685668858563737 ) ) ;
#22917 = CARTESIAN_POINT ( 'NONE',  ( 199.0227232939661519, -19.93874224789216143, -1.638880401382246443 ) ) ;
#22918 = CARTESIAN_POINT ( 'NONE',  ( -110.0960685945546231, -2.528047301428510085, 20.07406508575495607 ) ) ;
#22919 = CARTESIAN_POINT ( 'NONE',  ( 136.1360204305621551, -24.77266263493126885, 31.79587985999256006 ) ) ;
#22920 = CARTESIAN_POINT ( 'NONE',  ( -280.0000000000000000, -14.14213562373098831, -14.14213562373098654 ) ) ;
#22921 = CARTESIAN_POINT ( 'NONE',  ( -100.7734535825088500, 40.00000000000008527, -22.67402823373177512 ) ) ;
#22922 = CARTESIAN_POINT ( 'NONE',  ( -200.0000000000000000, -19.96680831879894669, 45.63305559644814480 ) ) ;
#22923 = EDGE_CURVE ( 'NONE', #3897, #4688, #19054, .T. ) ;
#22924 = PLANE ( 'NONE',  #3764 ) ;
#22925 = CARTESIAN_POINT ( 'NONE',  ( -105.3755690713226585, 40.00000000000019185, -18.24025645688310249 ) ) ;
#22926 = CARTESIAN_POINT ( 'NONE',  ( -198.0356074513804572, 40.00000000000056843, -55.37879056871282302 ) ) ;
#22927 = CARTESIAN_POINT ( 'NONE',  ( -656.9692583454861960, 39.98845026487703080, -1.092349456584704948 ) ) ;
#22928 = CARTESIAN_POINT ( 'NONE',  ( -87.11144460356582897, -17.02335282540412109, -13.16693477525666367 ) ) ;
#22929 = CARTESIAN_POINT ( 'NONE',  ( 199.0111318983613842, 19.03723981379789265, 6.131360352008743853 ) ) ;
#22930 = CIRCLE ( 'NONE', #15311, 29.99999999999999289 ) ;
#22931 = CARTESIAN_POINT ( 'NONE',  ( -188.3120147333419254, 13.82877842034795712, 46.99495896211607260 ) ) ;
#22932 = CARTESIAN_POINT ( 'NONE',  ( -198.0356074513804572, -10.87444709759714634, -10.87444709759729911 ) ) ;
#22933 = DIRECTION ( 'NONE',  ( 1.000000000000000000, -1.836970198721030181E-16, -0.000000000000000000 ) ) ;
#22934 = CARTESIAN_POINT ( 'NONE',  ( 151.7948205124836250, -4.785054706301671068, 4.785054706301645311 ) ) ;
#22935 = FACE_OUTER_BOUND ( 'NONE', #8170, .T. ) ;
#22936 = CARTESIAN_POINT ( 'NONE',  ( 0.2972598230769923355, 18.14793986248751168, -38.42060263243650553 ) ) ;
#22937 = CARTESIAN_POINT ( 'NONE',  ( -200.0000000000000568, 47.96425349429458151, -15.65821854886104880 ) ) ;
#22938 = DIRECTION ( 'NONE',  ( -0.01051738777840045304, 0.3656191333263374976, 0.9307051272556827737 ) ) ;
#22939 = CARTESIAN_POINT ( 'NONE',  ( -91.56559293963834989, 12.25131212657428748, 44.31723036834913643 ) ) ;
#22940 = CARTESIAN_POINT ( 'NONE',  ( -192.9588430854690273, -14.46834944099973264, 40.00000000000002132 ) ) ;
#22941 = CARTESIAN_POINT ( 'NONE',  ( -592.0016308006249801, 44.98679260217947018, -1.246943552952227696 ) ) ;
#22942 = VERTEX_POINT ( 'NONE', #12666 ) ;
#22943 = ADVANCED_BREP_SHAPE_REPRESENTATION ( '', ( #8434, #21058 ), #4479 ) ;
#22944 = CARTESIAN_POINT ( 'NONE',  ( 184.8905102610680444, 2.362515690532070066E-13, -19.07866798485558490 ) ) ;
#22945 = CARTESIAN_POINT ( 'NONE',  ( -726.9846540392142060, 66.50000000000009948, -61.50000000000004974 ) ) ;
#22946 = CARTESIAN_POINT ( 'NONE',  ( 118.9130007099545878, -10.68958087202361718, 25.80693111732275113 ) ) ;
#22947 = VERTEX_POINT ( 'NONE', #14790 ) ;
#22948 = ORIENTED_EDGE ( 'NONE', *, *, #25089, .F. ) ;
#22949 = CARTESIAN_POINT ( 'NONE',  ( -86.96347745069644475, 18.24025645688350750, 40.00000000000002132 ) ) ;
#22950 = CARTESIAN_POINT ( 'NONE',  ( -200.0000000000000000, 0.000000000000000000, 0.000000000000000000 ) ) ;
#22951 = VECTOR ( 'NONE', #12507, 1000.000000000000000 ) ;
#22952 = CARTESIAN_POINT ( 'NONE',  ( -105.3394646353531954, -20.62740382080770729, -5.712077376962630737 ) ) ;
#22953 = DIRECTION ( 'NONE',  ( 0.9698969544411814026, 0.09318942518809772424, -0.2249791741447042526 ) ) ;
#22954 = CARTESIAN_POINT ( 'NONE',  ( 91.82158438592158234, 7.693928927950222250E-14, -17.20528682183300262 ) ) ;
#22955 = CARTESIAN_POINT ( 'NONE',  ( 199.9999999999999716, 14.88808753490056880, -11.80862348214050606 ) ) ;
#22956 =( REPRESENTATION_RELATIONSHIP ('NONE','NONE', #23888, #14572 ) REPRESENTATION_RELATIONSHIP_WITH_TRANSFORMATION ( #12618 )SHAPE_REPRESENTATION_RELATIONSHIP( ) );
#22957 = CARTESIAN_POINT ( 'NONE',  ( -726.9846540392142060, 52.50000000000007816, 52.49999999999999289 ) ) ;
#22958 = CARTESIAN_POINT ( 'NONE',  ( -238.4067589809705794, 0.6820004457912851592, -0.6820004457913123597 ) ) ;
#22959 = CARTESIAN_POINT ( 'NONE',  ( -198.0356074513804572, -10.87444709759714634, -10.87444709759729911 ) ) ;
#22960 = CYLINDRICAL_SURFACE ( 'NONE', #13134, 69.99999999999994316 ) ;
#22961 = CARTESIAN_POINT ( 'NONE',  ( 91.82158438592156813, 39.99999999999986500, 17.20528682183341473 ) ) ;
#22962 = CARTESIAN_POINT ( 'NONE',  ( 0.2972598230769976091, -10.13633138497465147, -10.13633138497482733 ) ) ;
#22963 = CARTESIAN_POINT ( 'NONE',  ( -198.0356074513804572, -15.37879056873074290, 0.000000000000000000 ) ) ;
#22964 = CARTESIAN_POINT ( 'NONE',  ( -135.8532207217289738, -6.472252184284287502, 50.09629031063965243 ) ) ;
#22965 = CARTESIAN_POINT ( 'NONE',  ( 19.06497207195982568, -38.31983398719646061, 38.31983398719606271 ) ) ;
#22966 = CARTESIAN_POINT ( 'NONE',  ( 199.0110640845461489, 19.08185933734193895, 5.992088389419413019 ) ) ;
#22967 = CIRCLE ( 'NONE', #6811, 10.00000000000004796 ) ;
#22969 = CARTESIAN_POINT ( 'NONE',  ( 130.8568914410475372, 1.429239637432775288E-13, -34.05028731879788495 ) ) ;
#22968 = CARTESIAN_POINT ( 'NONE',  ( 57.59792236341147031, -30.00663442387662627, -26.56190807104723461 ) ) ;
#22970 = CARTESIAN_POINT ( 'NONE',  ( 44.46627453574045319, 36.79413088008411137, -15.24062802596003507 ) ) ;
#22971 = CARTESIAN_POINT ( 'NONE',  ( 130.8568914410475372, -34.05028731879786363, 0.000000000000000000 ) ) ;
#22972 = CARTESIAN_POINT ( 'NONE',  ( 91.82158438592158234, -12.16597498397761967, -12.16597498397768007 ) ) ;
#22973 = CARTESIAN_POINT ( 'NONE',  ( 184.8905102610680444, -20.92133201514440799, 40.00000000000002132 ) ) ;
#22974 = ORIENTED_EDGE ( 'NONE', *, *, #6967, .T. ) ;
#22975 = ADVANCED_FACE ( 'NONE', ( #16922 ), #16788, .F. ) ;
#22976 = CARTESIAN_POINT ( 'NONE',  ( -2.004660104900875872, -43.67474423982626774, 18.09067139730424500 ) ) ;
#22977 = CARTESIAN_POINT ( 'NONE',  ( 151.7948205124836534, -33.23291073765550863, 40.00000000000002132 ) ) ;
#22978 = ORIENTED_EDGE ( 'NONE', *, *, #25921, .T. ) ;
#22979 = LINE ( 'NONE', #19109, #25545 ) ;
#22980 = EDGE_CURVE ( 'NONE', #2033, #16316, #19560, .T. ) ;
#22981 = CARTESIAN_POINT ( 'NONE',  ( -162.0762913951020892, 1.198031840385716418, 1.198031840385750169 ) ) ;
#22982 = CARTESIAN_POINT ( 'NONE',  ( -4.061681315507533974, -23.44498947467614514, 42.99867639910929995 ) ) ;
#22983 = CARTESIAN_POINT ( 'NONE',  ( 19.06497207195980792, 10.03556273973433299, 10.03556273973436319 ) ) ;
#22984 = EDGE_CURVE ( 'NONE', #18786, #14909, #21988, .T. ) ;
#22985 = EDGE_CURVE ( 'NONE', #1721, #2983, #16585, .T. ) ;
#22986 = CARTESIAN_POINT ( 'NONE',  ( -4.022465846214347884, 13.82902411340800519, -46.99661175925213996 ) ) ;
#22987 = CARTESIAN_POINT ( 'NONE',  ( 199.0248198352711313, -19.48551319141294869, 4.538181572781159190 ) ) ;
#22988 = CARTESIAN_POINT ( 'NONE',  ( 192.4448373802100889, -14.14213562375896061, 14.14213562375865330 ) ) ;
#22989 = DIRECTION ( 'NONE',  ( 1.000000000000000000, 0.000000000000000000, 0.000000000000000000 ) ) ;
#22990 =( NAMED_UNIT ( * ) SI_UNIT ( $, .STERADIAN. ) SOLID_ANGLE_UNIT ( ) );
#22991 = CARTESIAN_POINT ( 'NONE',  ( -188.4702232936913333, -13.83721295434360421, 47.05182887786764923 ) ) ;
#22992 = CARTESIAN_POINT ( 'NONE',  ( 14.38125909742181285, -10.73282306404712472, -10.73282306404731301 ) ) ;
#22993 = CARTESIAN_POINT ( 'NONE',  ( 163.1118516004056573, 19.27778845539212327, 37.29075403953164169 ) ) ;
#22994 = CARTESIAN_POINT ( 'NONE',  ( 0.2972598230769938343, 10.13633138497486286, -10.13633138497461594 ) ) ;
#22995 = CARTESIAN_POINT ( 'NONE',  ( -135.8532207217289738, 34.75652343174625258, -21.81201906317744132 ) ) ;
#22997 = CARTESIAN_POINT ( 'NONE',  ( 163.1118516004056573, 37.29075403953132906, 19.27778845539275565 ) ) ;
#22996 = DIRECTION ( 'NONE',  ( 0.7071067811865440200, 0.7071067811865511255, 0.000000000000000000 ) ) ;
#22998 = CARTESIAN_POINT ( 'NONE',  ( -198.0356074513804572, 39.15871834505887250, 17.40982414986519089 ) ) ;
#22999 = CARTESIAN_POINT ( 'NONE',  ( -192.9588430854689989, -14.46834944099973086, 0.000000000000000000 ) ) ;
#23000 = CARTESIAN_POINT ( 'NONE',  ( 19.06497207195980792, 14.19242893257840699, -40.00000000000002132 ) ) ;
#23001 = CARTESIAN_POINT ( 'NONE',  ( 19.06497207195980792, 66.60410523465817789, 10.03556273973446800 ) ) ;
#23002 = DIRECTION ( 'NONE',  ( 0.000000000000000000, 1.000000000000000000, 0.000000000000000000 ) ) ;
#23003 = CARTESIAN_POINT ( 'NONE',  ( -100.7734535825088358, -12.25131212657475643, -12.25131212657495539 ) ) ;
#23004 = VECTOR ( 'NONE', #2919, 1000.000000000000000 ) ;
#23005 = CARTESIAN_POINT ( 'NONE',  ( -187.3036811847820786, 42.71162014089968295, -23.25512365539639958 ) ) ;
#23006 = VERTEX_POINT ( 'NONE', #11069 ) ;
#23007 = CARTESIAN_POINT ( 'NONE',  ( 130.8568914410475088, -24.07718906446910623, 32.49135343045471558 ) ) ;
#23008 = CIRCLE ( 'NONE', #3439, 5.000000000000004441 ) ;
#23009 = VECTOR ( 'NONE', #8823, 1000.000000000000000 ) ;
#23010 = AXIS2_PLACEMENT_3D ( 'NONE', #5077, #17416, #21302 ) ;
#23011 = CARTESIAN_POINT ( 'NONE',  ( -93.02511667906952653, -20.82219708225693466, -8.169918093965536698 ) ) ;
#23012 = CONTEXT_DEPENDENT_SHAPE_REPRESENTATION ( #25338, #2329 ) ;
#23013 = AXIS2_PLACEMENT_3D ( 'NONE', #1122, #2265, #10243 ) ;
#23014 = CARTESIAN_POINT ( 'NONE',  ( 136.1360204305621266, -3.511608612530682905, 3.511608612530666917 ) ) ;
#23015 = CARTESIAN_POINT ( 'NONE',  ( 4.155455573178285178, -44.65020969900605508, -18.49472242011575673 ) ) ;
#23016 = ORIENTED_EDGE ( 'NONE', *, *, #1673, .F. ) ;
#23017 = CARTESIAN_POINT ( 'NONE',  ( 136.1360204305621266, -35.03383547441293899, 0.000000000000000000 ) ) ;
#23018 = CARTESIAN_POINT ( 'NONE',  ( -87.13361725327074225, -15.19799821270840035, -15.19799821270843765 ) ) ;
#23019 = CARTESIAN_POINT ( 'NONE',  ( 199.9999999999998010, 5.803429233430792422, -18.09525674440013177 ) ) ;
#23020 = FACE_OUTER_BOUND ( 'NONE', #3717, .T. ) ;
#23021 = CARTESIAN_POINT ( 'NONE',  ( 19.06497207195980792, 54.19242893257843718, 2.449293598294708485E-15 ) ) ;
#23022 = CARTESIAN_POINT ( 'NONE',  ( -91.56559293963834989, -44.31723036834885932, -12.25131212657538171 ) ) ;
#23023 = CARTESIAN_POINT ( 'NONE',  ( 199.0075440639197666, 19.83040477280651714, -2.587228267588620234 ) ) ;
#23024 = AXIS2_PLACEMENT_3D ( 'NONE', #14749, #6503, #6768 ) ;
#23025 = CARTESIAN_POINT ( 'NONE',  ( 151.7948205124836534, -33.06932595376376582, 23.49921654115996006 ) ) ;
#23026 = CARTESIAN_POINT ( 'NONE',  ( -198.0356074513804572, -2.321818583541004323E-13, 55.37879056873073580 ) ) ;
#23027 = CARTESIAN_POINT ( 'NONE',  ( -135.8532207217289738, 39.99999999999989342, 30.84685318188660474 ) ) ;
#23028 = DIRECTION ( 'NONE',  ( 0.000000000000000000, 0.000000000000000000, 1.000000000000000000 ) ) ;
#23029 = CARTESIAN_POINT ( 'NONE',  ( -213.1075012329536946, -53.71589010951918652, -2.449293598294708485E-15 ) ) ;
#23031 = CARTESIAN_POINT ( 'NONE',  ( 170.2234770963711128, 17.36149277827004411, -17.36149277826983095 ) ) ;
#23030 = CARTESIAN_POINT ( 'NONE',  ( 22.86726691379337595, -17.87269271907613444, -43.14849715852183465 ) ) ;
#23032 = CARTESIAN_POINT ( 'NONE',  ( 184.8905102610680444, -19.07866798485555293, -2.449293598294708485E-15 ) ) ;
#23033 = CARTESIAN_POINT ( 'NONE',  ( -91.56559293963836410, 16.03295912088714203, -16.03295912088699282 ) ) ;
#23034 = CARTESIAN_POINT ( 'NONE',  ( 125.5832160019860169, -11.61997419108375063, -28.05309928653998242 ) ) ;
#23035 = CARTESIAN_POINT ( 'NONE',  ( -114.5444905533168338, 9.939131763671985809, -19.55376799566989732 ) ) ;
#23036 = CARTESIAN_POINT ( 'NONE',  ( -280.0000000000000000, 1.605030083646939673E-13, -20.00000000000001421 ) ) ;
#23037 = CARTESIAN_POINT ( 'NONE',  ( -100.7734535825088358, -16.03295912088706743, -16.03295912088710296 ) ) ;
#23038 = CARTESIAN_POINT ( 'NONE',  ( -105.2054292635175585, 21.49321519473984665, 5.610018989487960791E-28 ) ) ;
#23039 = CARTESIAN_POINT ( 'NONE',  ( -210.0000000000000284, -52.49999999999992895, -52.49999999999999289 ) ) ;
#23040 = CARTESIAN_POINT ( 'NONE',  ( -86.96347745069644475, -12.89780903124413491, 12.89780903124398037 ) ) ;
#23041 = ORIENTED_EDGE ( 'NONE', *, *, #8764, .T. ) ;
#23043 = CARTESIAN_POINT ( 'NONE',  ( -17.28139728232450878, 39.07633224428969498, -20.85871090880913670 ) ) ;
#23042 = CARTESIAN_POINT ( 'NONE',  ( -56.48582580120559271, 6.472252184284121412, 6.472252184284244869 ) ) ;
#23044 = DIRECTION ( 'NONE',  ( -1.000000000000000000, 1.836970198721030181E-16, 0.000000000000000000 ) ) ;
#23045 = CARTESIAN_POINT ( 'NONE',  ( -86.96347745069644475, -18.24025645688354302, -2.449293598294708485E-15 ) ) ;
#23046 = CARTESIAN_POINT ( 'NONE',  ( -114.7537493279933187, 13.57142477590316254, -17.50316801958423341 ) ) ;
#23047 = CARTESIAN_POINT ( 'NONE',  ( -238.4067589809705794, 0.6820004457912851592, -0.6820004457913123597 ) ) ;
#23048 =( LENGTH_UNIT ( ) NAMED_UNIT ( * ) SI_UNIT ( .MILLI., .METRE. ) );
#23049 = VERTEX_POINT ( 'NONE', #19184 ) ;
#23050 = EDGE_LOOP ( 'NONE', ( #9769, #23972 ) ) ;
#23051 = AXIS2_PLACEMENT_3D ( 'NONE', #1586, #9689, #15796 ) ;
#23052 = CARTESIAN_POINT ( 'NONE',  ( 199.9999999999999432, -13.00408651859840958, 13.88070474188551451 ) ) ;
#23053 = CARTESIAN_POINT ( 'NONE',  ( -211.2619052429883482, 0.000000000000000000, 0.000000000000000000 ) ) ;
#23054 = VERTEX_POINT ( 'NONE', #20928 ) ;
#23055 = ORIENTED_EDGE ( 'NONE', *, *, #25999, .F. ) ;
#23056 = CARTESIAN_POINT ( 'NONE',  ( -162.0762913951021176, 1.198031840315997298, 57.76657433523996588 ) ) ;
#23057 = CARTESIAN_POINT ( 'NONE',  ( 199.0252366630825520, -19.04991887513223503, 6.114737037930856545 ) ) ;
#23058 = CARTESIAN_POINT ( 'NONE',  ( -114.7755410848759112, 1.384971738882062819, 22.09261867840957194 ) ) ;
#23059 = CARTESIAN_POINT ( 'NONE',  ( 199.9999999999999432, -14.14213562373096345, -14.14213562373104871 ) ) ;
#23060 = DIRECTION ( 'NONE',  ( -1.000000000000000000, 0.000000000000000000, 0.000000000000000000 ) ) ;
#23061 = CARTESIAN_POINT ( 'NONE',  ( -105.3755690713226585, 39.99999999999993605, 18.24025645688366737 ) ) ;
#23062 = DIRECTION ( 'NONE',  ( 1.000000000000000000, 1.836970198721030181E-16, 0.000000000000000000 ) ) ;
#23063 = CARTESIAN_POINT ( 'NONE',  ( -86.86578273022547592, -8.153770686795120071, -19.68494377654086236 ) ) ;
#23064 = CARTESIAN_POINT ( 'NONE',  ( -100.7734535825088500, -39.99999999999986500, -17.32597176626853397 ) ) ;
#23065 = CARTESIAN_POINT ( 'NONE',  ( 130.8568914410475372, -3.326198072800416995E-13, 34.05028731879788495 ) ) ;
#23066 = CARTESIAN_POINT ( 'NONE',  ( -87.10945906665416771, 16.83914111323053220, 13.33429271096284729 ) ) ;
#23067 = CIRCLE ( 'NONE', #11550, 5.000000000000004441 ) ;
#23068 = DIRECTION ( 'NONE',  ( 1.000000000000000000, 1.836970198721030181E-16, 0.000000000000000000 ) ) ;
#23069 = CARTESIAN_POINT ( 'NONE',  ( 199.0091071337781159, 19.93120984291649478, 1.649067560610785854 ) ) ;
#23070 = CARTESIAN_POINT ( 'NONE',  ( -190.0144222803081675, 23.79986276084134289, 43.47820992357743819 ) ) ;
#23071 = CARTESIAN_POINT ( 'NONE',  ( -162.0762913951020892, -1.198031840385767266, -1.198031840385758384 ) ) ;
#23072 = CARTESIAN_POINT ( 'NONE',  ( -89.92902785008925548, 8.734793929541238455, 20.17328762787341034 ) ) ;
#23073 = CARTESIAN_POINT ( 'NONE',  ( 19.06497207195981858, -10.03556273973469715, 66.60410523465813526 ) ) ;
#23074 = CARTESIAN_POINT ( 'NONE',  ( -82.30220482034327745, -18.51665893431350085, 7.992411108785186791 ) ) ;
#23075 = CARTESIAN_POINT ( 'NONE',  ( -100.7734535825088500, 16.03295912088740494, -40.53558337403661938 ) ) ;
#23076 = CARTESIAN_POINT ( 'NONE',  ( -661.7304433267322565, 44.80254769115845903, 4.254228907715386754 ) ) ;
#23077 = CARTESIAN_POINT ( 'NONE',  ( 170.2234770963711128, 24.55285855007190676, 40.00000000000002132 ) ) ;
#23078 = CARTESIAN_POINT ( 'NONE',  ( -56.48582580120559982, 21.81201906317729922, 34.75652343174635917 ) ) ;
#23079 = CARTESIAN_POINT ( 'NONE',  ( -100.7734535825088500, 22.67402823373189946, 40.00000000000002132 ) ) ;
#23080 = CARTESIAN_POINT ( 'NONE',  ( -626.9846540392142060, 28.28427124746186294, -34.99999999999999289 ) ) ;
#23081 = VERTEX_POINT ( 'NONE', #17053 ) ;
#23082 = CARTESIAN_POINT ( 'NONE',  ( -192.9588430854690273, -39.99999999999991473, -14.46834944100011633 ) ) ;
#23083 = CARTESIAN_POINT ( 'NONE',  ( -105.4741150117383341, -8.366608964593364561, -19.60045294982747777 ) ) ;
#23084 = ADVANCED_FACE ( 'NONE', ( #20793, #2564 ), #6675, .F. ) ;
#23085 = CARTESIAN_POINT ( 'NONE',  ( 130.1167162091012983, -12.15076864148480418, 29.33455044752945895 ) ) ;
#23086 = ORIENTED_EDGE ( 'NONE', *, *, #9009, .F. ) ;
#23087 = VERTEX_POINT ( 'NONE', #3463 ) ;
#23088 = ORIENTED_EDGE ( 'NONE', *, *, #19475, .T. ) ;
#23089 = CARTESIAN_POINT ( 'NONE',  ( 192.4448373802101173, 19.99999999996063949, 40.00000000000002132 ) ) ;
#23090 = ADVANCED_FACE ( 'NONE', ( #15811 ), #5714, .T. ) ;
#23091 = FACE_OUTER_BOUND ( 'NONE', #26264, .T. ) ;
#23092 = EDGE_CURVE ( 'NONE', #17459, #14871, #15555, .T. ) ;
#23093 = CARTESIAN_POINT ( 'NONE',  ( -105.2833435977218812, -20.98775841734472181, -4.389626034958370226 ) ) ;
#23094 = CARTESIAN_POINT ( 'NONE',  ( 151.7948205124836250, -23.49921654116339553, -23.49921654116350211 ) ) ;
#23095 = CARTESIAN_POINT ( 'NONE',  ( -280.0000000000000568, -40.00000000000000000, -20.00000000000015277 ) ) ;
#23096 = CARTESIAN_POINT ( 'NONE',  ( 200.0000000000001705, 5.211075256460824257, -18.27473396828003871 ) ) ;
#23097 = CARTESIAN_POINT ( 'NONE',  ( 199.9999999999999716, 3.398245514232853814, -18.69524394795535827 ) ) ;
#23098 = CARTESIAN_POINT ( 'NONE',  ( -198.0356074513804572, -17.40982414986427429, -39.15871834505933435 ) ) ;
#23099 = CARTESIAN_POINT ( 'NONE',  ( 19.06497207195981147, -10.03556273973425483, -10.03556273973443247 ) ) ;
#23100 = CYLINDRICAL_SURFACE ( 'NONE', #16529, 5.000000000000004441 ) ;
#23101 = CARTESIAN_POINT ( 'NONE',  ( 163.1118516004056573, 1.658263919738574066E-13, -12.73709011382475254 ) ) ;
#23102 = CARTESIAN_POINT ( 'NONE',  ( 163.1118516004056573, 19.27778845538753316, 19.27778845538783870 ) ) ;
#23103 = CARTESIAN_POINT ( 'NONE',  ( 17.75917311731579673, 14.04884443869898014, 48.46615948699193410 ) ) ;
#23104 = CARTESIAN_POINT ( 'NONE',  ( -192.9588430854690273, -10.23066800229550388, 66.79921049721887982 ) ) ;
#23105 = CARTESIAN_POINT ( 'NONE',  ( 199.0123650023721495, 18.11534524532891766, 8.488184440863852487 ) ) ;
#23107 = CARTESIAN_POINT ( 'NONE',  ( 0.2972598230769957217, -4.999556039334937811E-14, 14.33493731733933352 ) ) ;
#23106 = CARTESIAN_POINT ( 'NONE',  ( -213.1075012329537230, -18.58567234101102272, -37.98287015391260013 ) ) ;
#23108 = CARTESIAN_POINT ( 'NONE',  ( 19.06497207195980792, 14.19242893257840699, -40.00000000000002132 ) ) ;
#23109 = CARTESIAN_POINT ( 'NONE',  ( -198.0356074513804572, 10.87444709758468875, 67.44298959250869530 ) ) ;
#23110 = CARTESIAN_POINT ( 'NONE',  ( -86.96347745069644475, -21.75974354311652093, 40.00000000000002132 ) ) ;
#23111 = ORIENTED_EDGE ( 'NONE', *, *, #5075, .T. ) ;
#23112 = CARTESIAN_POINT ( 'NONE',  ( 11.28112952475396469, -44.87390167240484118, 18.58737866931859983 ) ) ;
#23113 = CARTESIAN_POINT ( 'NONE',  ( -86.96347745069644475, -21.75974354311652093, -40.00000000000002132 ) ) ;
#23114 = CARTESIAN_POINT ( 'NONE',  ( 170.0000000000000000, -24.95097643316997704, 0.000000000000000000 ) ) ;
#23115 = CARTESIAN_POINT ( 'NONE',  ( -280.0000000000000000, 14.14213562373088351, 14.14213562373098654 ) ) ;
#23116 = CARTESIAN_POINT ( 'NONE',  ( 14.38125909742181818, -40.00000000000007816, 15.17850393972619649 ) ) ;
#23117 = CARTESIAN_POINT ( 'NONE',  ( -82.26903151907711731, 19.50325165503522840, 5.351754661224573439 ) ) ;
#23118 = CARTESIAN_POINT ( 'NONE',  ( -39.81953879993444190, 16.38089232947213958, -32.18669035976384407 ) ) ;
#23119 = CARTESIAN_POINT ( 'NONE',  ( 199.0263730241462099, -14.60190056250242030, 13.67829565473005715 ) ) ;
#23120 = CARTESIAN_POINT ( 'NONE',  ( -192.9588430854690273, 38.51493924976913519, 18.05360324515490333 ) ) ;
#23121 = CARTESIAN_POINT ( 'NONE',  ( -82.26531528646586366, -19.58553546193898853, 5.040628272971080293 ) ) ;
#23122 = CARTESIAN_POINT ( 'NONE',  ( 190.0000000000000000, -52.49999999999992895, -52.49999999999999289 ) ) ;
#23123 = CARTESIAN_POINT ( 'NONE',  ( -195.5008451366654469, -18.44412755964216899, 44.52806290062937222 ) ) ;
#23124 = CARTESIAN_POINT ( 'NONE',  ( -56.48582580120559271, 6.472252184284121412, 6.472252184284244869 ) ) ;
#23125 = EDGE_CURVE ( 'NONE', #10668, #22320, #3849, .T. ) ;
#23126 = CARTESIAN_POINT ( 'NONE',  ( -91.56559293963836410, 16.03295912088714203, -16.03295912088699282 ) ) ;
#23127 = CARTESIAN_POINT ( 'NONE',  ( -162.0762913951020892, 1.198031840385732849, -1.198031840385733515 ) ) ;
#23128 = CARTESIAN_POINT ( 'NONE',  ( -192.9588430854690273, 18.05360324515473280, -38.51493924976924177 ) ) ;
#23130 = CARTESIAN_POINT ( 'NONE',  ( 0.2972598230769959993, 38.42060263243713081, -38.42060263243619289 ) ) ;
#23129 = CARTESIAN_POINT ( 'NONE',  ( -56.48582580120559982, 34.75652343174628101, -21.81201906317743067 ) ) ;
#23131 = CARTESIAN_POINT ( 'NONE',  ( 14.38125909742181108, 39.01709431150961649, -39.01709431150867147 ) ) ;
#23132 = CARTESIAN_POINT ( 'NONE',  ( 57.59792236341147031, 37.56421063658187620, -40.00000000000002132 ) ) ;
#23133 = CARTESIAN_POINT ( 'NONE',  ( -100.7734535825088358, -16.03295912088706743, -16.03295912088710296 ) ) ;
#23134 = DIRECTION ( 'NONE',  ( 0.000000000000000000, -1.000000000000000000, 0.000000000000000000 ) ) ;
#23135 = CARTESIAN_POINT ( 'NONE',  ( -91.56559293963836410, -12.25131212657524138, 44.31723036834888774 ) ) ;
#23136 = EDGE_CURVE ( 'NONE', #2697, #18845, #9368, .T. ) ;
#23137 = CARTESIAN_POINT ( 'NONE',  ( -188.8753211508393690, 43.29880796194926518, -17.93495349242721204 ) ) ;
#23138 = EDGE_LOOP ( 'NONE', ( #4062, #4816, #22048, #21215 ) ) ;
#23139 = CARTESIAN_POINT ( 'NONE',  ( 200.0000000000000000, -14.14213562373106114, 42.42640687119278908 ) ) ;
#23140 = CARTESIAN_POINT ( 'NONE',  ( -87.13361725327074225, -15.19799821270840390, -15.19799821270844120 ) ) ;
#23141 = CARTESIAN_POINT ( 'NONE',  ( -30.26275506840322649, -29.48230279907810925, 29.48230279907778950 ) ) ;
#23142 = CARTESIAN_POINT ( 'NONE',  ( -77.90022806219018037, -20.16431395584817210, -8.352332316461392736 ) ) ;
#23143 = ORIENTED_EDGE ( 'NONE', *, *, #18340, .T. ) ;
#23144 = CARTESIAN_POINT ( 'NONE',  ( -105.3942160150412519, 19.19970061689178564, 9.473065214623858310 ) ) ;
#23145 = CARTESIAN_POINT ( 'NONE',  ( 199.9999999999998863, 9.229831349313808886, -16.61069465220444386 ) ) ;
#23146 = CARTESIAN_POINT ( 'NONE',  ( 160.9163046357249129, -125.7889608577475684, -49.61140153332242875 ) ) ;
#23147 = CARTESIAN_POINT ( 'NONE',  ( -198.0356074513804572, 55.37879056873070027, 2.449293598294708485E-15 ) ) ;
#23148 = CARTESIAN_POINT ( 'NONE',  ( 83.11963132832433132, 9.001241435325864515, -24.42551322443806683 ) ) ;
#23149 = CARTESIAN_POINT ( 'NONE',  ( 199.0145894300637792, 15.86095929198710586, 12.18642508278280623 ) ) ;
#23150 = CARTESIAN_POINT ( 'NONE',  ( 163.1118516004056573, -37.29075403953166301, 19.27778845539196695 ) ) ;
#23151 = CARTESIAN_POINT ( 'NONE',  ( -280.0000000000000568, 39.99999999999990763, 20.00000000000015987 ) ) ;
#23152 = CARTESIAN_POINT ( 'NONE',  ( 146.6084372240433709, 40.00000000000003553, 5.374981219217116468 ) ) ;
#23153 = FACE_OUTER_BOUND ( 'NONE', #18507, .T. ) ;
#23154 = CARTESIAN_POINT ( 'NONE',  ( -162.0762913951020892, -41.69427287672991866, -40.00000000000002132 ) ) ;
#23156 = CARTESIAN_POINT ( 'NONE',  ( -91.56559293963836410, 16.03295912088714203, -16.03295912088699282 ) ) ;
#23155 = CARTESIAN_POINT ( 'NONE',  ( 27.55177309529138441, -22.48880744266456588, -41.56868263114530748 ) ) ;
#23157 = CARTESIAN_POINT ( 'NONE',  ( -86.96347745069643054, -18.24025645688353947, 40.00000000000002132 ) ) ;
#23158 = CARTESIAN_POINT ( 'NONE',  ( -56.48582580120559271, 6.472252184284211118, -6.472252184284153387 ) ) ;
#23159 = CARTESIAN_POINT ( 'NONE',  ( 146.6084372240433993, -3.357462877844280890E-13, 34.62501878078305850 ) ) ;
#23160 = CARTESIAN_POINT ( 'NONE',  ( -114.7248266913118897, 17.87714126013195326, -12.97729011815941469 ) ) ;
#23161 = CARTESIAN_POINT ( 'NONE',  ( -208.1127848780264742, -39.99999999999990763, -15.00245453012711394 ) ) ;
#23162 = CARTESIAN_POINT ( 'NONE',  ( -198.0356074513804572, 10.87444709759714989, 10.87444709759722450 ) ) ;
#23163 = CARTESIAN_POINT ( 'NONE',  ( -295.0000000000000568, -4.857225732735059864E-14, 0.000000000000000000 ) ) ;
#23164 = CARTESIAN_POINT ( 'NONE',  ( -30.26275506840325136, 29.48230279907760121, 27.08623969584625613 ) ) ;
#23165 = CARTESIAN_POINT ( 'NONE',  ( -162.0762913951021176, 27.08623940707598265, 29.48230308784781428 ) ) ;
#23166 = ADVANCED_FACE ( 'NONE', ( #21688 ), #25691, .F. ) ;
#23167 = ORIENTED_EDGE ( 'NONE', *, *, #18683, .T. ) ;
#23169 = CARTESIAN_POINT ( 'NONE',  ( -70.35386311751949506, 22.51194464734792433, -10.19784241718953588 ) ) ;
#23168 = CARTESIAN_POINT ( 'NONE',  ( -86.94949953272028154, 19.08279132442754644, -9.637191076863791395 ) ) ;
#23170 = CARTESIAN_POINT ( 'NONE',  ( 156.1979191798868101, 27.38417834433190379, -11.34289806466565764 ) ) ;
#23171 = CARTESIAN_POINT ( 'NONE',  ( -259.2033419157646676, 9.517827891722582478, 40.00000000000002132 ) ) ;
#23172 = FACE_OUTER_BOUND ( 'NONE', #22214, .T. ) ;
#23173 = CARTESIAN_POINT ( 'NONE',  ( -197.4154352061690645, 49.11380478896982282, -14.14666496776101212 ) ) ;
#23174 = ORIENTED_EDGE ( 'NONE', *, *, #22319, .F. ) ;
#23175 = ORIENTED_EDGE ( 'NONE', *, *, #11555, .F. ) ;
#23176 = CARTESIAN_POINT ( 'NONE',  ( 199.9999999999999716, -9.646513317630143192, 16.38616289770262568 ) ) ;
#23177 = CARTESIAN_POINT ( 'NONE',  ( 98.29820294267312875, 7.653668647304333383, -18.47759065023115355 ) ) ;
#23178 = CARTESIAN_POINT ( 'NONE',  ( -190.1760717698206520, 43.55712811720382405, -23.85870456570982157 ) ) ;
#23179 = ORIENTED_EDGE ( 'NONE', *, *, #22233, .T. ) ;
#23180 = CARTESIAN_POINT ( 'NONE',  ( 199.0234090143162859, -20.00365258984362882, 0.1656111763342176801 ) ) ;
#23181 = LINE ( 'NONE', #2562, #509 ) ;
#23182 = CARTESIAN_POINT ( 'NONE',  ( 163.1118516004056573, -19.27778845538761132, -19.27778845538770724 ) ) ;
#23183 = CARTESIAN_POINT ( 'NONE',  ( 192.4448373802100889, -14.14213562375876698, -14.14213562375885047 ) ) ;
#23184 = CARTESIAN_POINT ( 'NONE',  ( 163.1118516004056573, 40.00000000000000711, 12.73709011382489642 ) ) ;
#23185 = CARTESIAN_POINT ( 'NONE',  ( -99.21568817060988010, 6.094032021297641100E-14, -22.67402823373191723 ) ) ;
#23186 = FACE_BOUND ( 'NONE', #19806, .T. ) ;
#23187 = CARTESIAN_POINT ( 'NONE',  ( 199.9999999999999432, 2.486775779033024914E-13, -19.99999999999992539 ) ) ;
#23188 = AXIS2_PLACEMENT_3D ( 'NONE', #12260, #17970, #26258 ) ;
#23189 = CARTESIAN_POINT ( 'NONE',  ( -259.2033419157646676, -39.99999999999975131, -30.48217210827782608 ) ) ;
#23190 = CARTESIAN_POINT ( 'NONE',  ( -82.25253345620868117, 16.60364765899479167, 11.48998332232444852 ) ) ;
#23191 = CARTESIAN_POINT ( 'NONE',  ( -199.9999999999999147, -14.17215463606695280, 49.28189405767609088 ) ) ;
#23192 = CARTESIAN_POINT ( 'NONE',  ( 199.0130717410369812, 17.47129959974107294, 9.736724163761770967 ) ) ;
#23193 = CARTESIAN_POINT ( 'NONE',  ( -208.1127848780265026, -10.60833733269551971, 10.60833733269537049 ) ) ;
#23194 = CARTESIAN_POINT ( 'NONE',  ( -162.0762913951021176, -29.48230308784793152, 27.08623940707591515 ) ) ;
#23195 = CARTESIAN_POINT ( 'NONE',  ( -188.7701069479165881, -47.15820909662600968, 13.85300054332501851 ) ) ;
#23196 = CARTESIAN_POINT ( 'NONE',  ( 170.0000000000000000, 3.122849337825751958E-14, 0.000000000000000000 ) ) ;
#23197 = CARTESIAN_POINT ( 'NONE',  ( -77.90255099906769942, 20.29001641120678201, -8.064892378658056415 ) ) ;
#23198 = VECTOR ( 'NONE', #25486, 1000.000000000000114 ) ;
#23199 = CARTESIAN_POINT ( 'NONE',  ( 0.2972598230770100991, -38.42060263243632079, -38.42060263243699580 ) ) ;
#23200 = CARTESIAN_POINT ( 'NONE',  ( -200.0000000000000000, 48.59548038928832625, -14.89048929005512001 ) ) ;
#23201 = CARTESIAN_POINT ( 'NONE',  ( 23.37394308801977871, 23.33966569535068203, 42.85717664514594816 ) ) ;
#23202 = ORIENTED_EDGE ( 'NONE', *, *, #7796, .T. ) ;
#23203 = CARTESIAN_POINT ( 'NONE',  ( -91.56559293963834989, 40.53558337403654832, 16.03295912088756481 ) ) ;
#23204 = CARTESIAN_POINT ( 'NONE',  ( -612.0709805440841365, 9.999999999999969802, 0.000000000000000000 ) ) ;
#23205 = CARTESIAN_POINT ( 'NONE',  ( -612.2848868978584278, 31.86264369326284651, -31.78304153250905628 ) ) ;
#23206 = ORIENTED_EDGE ( 'NONE', *, *, #17937, .T. ) ;
#23207 = CARTESIAN_POINT ( 'NONE',  ( 4.995406935893298872, 5.820775922023080204E-13, -55.24977328854835434 ) ) ;
#23208 = CARTESIAN_POINT ( 'NONE',  ( 199.0075023815175825, 2.710256083316576081, -19.82277908217579920 ) ) ;
#23209 = CARTESIAN_POINT ( 'NONE',  ( -716.9846540392142060, 66.50000000000009948, 66.50000000000005684 ) ) ;
#23210 = VECTOR ( 'NONE', #12299, 1000.000000000000000 ) ;
#23211 = VECTOR ( 'NONE', #17188, 1000.000000000000000 ) ;
#23212 = VERTEX_POINT ( 'NONE', #5330 ) ;
#23213 = EDGE_LOOP ( 'NONE', ( #3105, #20385, #1502, #16847 ) ) ;
#23214 = ORIENTED_EDGE ( 'NONE', *, *, #19887, .T. ) ;
#23215 = CARTESIAN_POINT ( 'NONE',  ( 136.1360204305621266, 4.966164525587089429, 2.449293598294708485E-15 ) ) ;
#23216 = CIRCLE ( 'NONE', #24027, 30.00000000000000000 ) ;
#23217 = CARTESIAN_POINT ( 'NONE',  ( -77.90255099906769942, -20.04994828523962269, 8.644468104261498809 ) ) ;
#23218 =( BOUNDED_SURFACE ( )  B_SPLINE_SURFACE ( 3, 2, ( 
 ( #19298, #9190, #17303 ),
 ( #23427, #3199, #11307 ),
 ( #19426, #13809, #26352 ),
 ( #22351, #24344, #20345 ),
 ( #6108, #14216, #13686 ),
 ( #1861, #21943, #4129 ),
 ( #20213, #3992, #3719 ),
 ( #11958, #11821, #15803 ),
 ( #19939, #9696, #7958 ),
 ( #24067, #12091, #5977 ),
 ( #26083, #9832, #21807 ),
 ( #7818, #18071, #1724 ),
 ( #22082, #9965, #23928 ),
 ( #8093, #14085, #1991 ),
 ( #15934, #3580, #5843 ),
 ( #12223, #26222, #20083 ),
 ( #17936, #121, #10097 ),
 ( #13947, #3855, #19809 ),
 ( #17803, #18199, #2122 ),
 ( #25949, #5703, #16076 ),
 ( #24204, #22216, #16213 ),
 ( #1595, #10230, #16344 ),
 ( #18339, #8226, #5579 ),
 ( #11683, #7690, #12892 ),
 ( #6628, #12481, #10495 ),
 ( #24607, #24742, #10901 ),
 ( #24476, #656, #2517 ),
 ( #19013, #20879, #10764 ),
 ( #8763, #10632, #6763 ),
 ( #4788, #18608, #791 ),
 ( #4652, #18743, #14352 ),
 ( #387, #524, #8496 ),
 ( #12349, #20608, #10360 ),
 ( #21006, #23015, #16878 ),
 ( #6238, #22480, #4259 ),
 ( #16609, #12620, #6497 ),
 ( #8629, #8895, #2788 ),
 ( #14745, #22613, #20478 ),
 ( #6361, #2251, #14608 ),
 ( #2383, #22739, #18470 ),
 ( #4522, #251, #20748 ),
 ( #24873, #25010, #4389 ),
 ( #14875, #16740, #8360 ),
 ( #14480, #12755, #16481 ),
 ( #22875, #2659, #18876 ),
 ( #21270, #3044, #11521 ),
 ( #7151, #5172, #1299 ),
 ( #17136, #21522, #3171 ),
 ( #17514, #25269, #11392 ),
 ( #7399, #9409, #5420 ),
 ( #25653, #15512, #25143 ),
 ( #13276, #7019, #23642 ),
 ( #5290, #15393, #15140 ),
 ( #23396, #23270, #921 ),
 ( #5045, #21145, #19394 ),
 ( #9150, #23518, #17389 ),
 ( #11151, #19266, #6894 ),
 ( #1048, #13521, #13152 ),
 ( #3419, #17265, #25400 ),
 ( #3296, #23142, #21647 ) ),
 .UNSPECIFIED., .F., .F., .F. ) 
 B_SPLINE_SURFACE_WITH_KNOTS ( ( 4, 2, 2, 2, 2, 2, 2, 2, 2, 2, 2, 2, 2, 2, 2, 2, 2, 2, 2, 2, 2, 2, 2, 2, 2, 2, 2, 2, 2, 4 ),
 ( 3, 3 ),
 ( -6.934549977324728988E-05, 0.02465257023823467716, 0.04937448597624260332, 0.07409640171425052602, 0.08027688064875250495, 0.08066316058215888818, 0.08085630054886207285, 0.08090458554053786555, 0.08095287053221367213, 0.08104944051556525753, 0.08182200038237799622, 0.08336712011600350136, 0.08645735958325448389, 0.09263783851775647671, 0.09881831745225845565, 0.1019085569195094521, 0.1049987963867604346, 0.1111792753212624274, 0.1173597542557644063, 0.1177460341891707896, 0.1179391741558739742, 0.1179874591475497669, 0.1180357441392255735, 0.1181323141225771589, 0.1189048739893898976, 0.1204499937230154027, 0.1235402331902663853, 0.1482621489282743010, 0.1729840646662822445, 0.1977059804042901603 ),
 ( 0.000000000000000000, 1.000000000000000000 ),
 .UNSPECIFIED. ) 
 GEOMETRIC_REPRESENTATION_ITEM ( )  RATIONAL_B_SPLINE_SURFACE ( (
 ( 1.000000000000000000, 1.000000000000000000, 1.000000000000000000),
 ( 1.000000000000000000, 0.9999975583951711267, 1.000000000000000000),
 ( 1.000000000000000000, 0.9982436956960243357, 1.000000000000000000),
 ( 1.000000000000000000, 0.9910288481552835815, 1.000000000000000000),
 ( 1.000000000000000000, 0.9855714588524815412, 1.000000000000000000),
 ( 1.000000000000000000, 0.9705958323307124491, 1.000000000000000000),
 ( 1.000000000000000000, 0.9610788543728796540, 1.000000000000000000),
 ( 1.000000000000000000, 0.9462867046313782060, 1.000000000000000000),
 ( 1.000000000000000000, 0.9431828180755336133, 1.000000000000000000),
 ( 1.000000000000000000, 0.9397240291170312343, 1.000000000000000000),
 ( 1.000000000000000000, 0.9395199791396151578, 1.000000000000000000),
 ( 1.000000000000000000, 0.9392130141387098341, 1.000000000000000000),
 ( 1.000000000000000000, 0.9391105441324959502, 1.000000000000000000),
 ( 1.000000000000000000, 0.9389822709566335579, 1.000000000000000000),
 ( 1.000000000000000000, 0.9389566070380604978, 1.000000000000000000),
 ( 1.000000000000000000, 0.9389052606279734148, 1.000000000000000000),
 ( 1.000000000000000000, 0.9388799835492064316, 1.000000000000000000),
 ( 1.000000000000000000, 0.9388039637710021701, 1.000000000000000000),
 ( 1.000000000000000000, 0.9387533729070449695, 1.000000000000000000),
 ( 1.000000000000000000, 0.9382988607466934416, 1.000000000000000000),
 ( 1.000000000000000000, 0.9379005790853075508, 1.000000000000000000),
 ( 1.000000000000000000, 0.9367237203702429849, 1.000000000000000000),
 ( 1.000000000000000000, 0.9359625442026195952, 1.000000000000000000),
 ( 1.000000000000000000, 0.9337619511408732365, 1.000000000000000000),
 ( 1.000000000000000000, 0.9324064515427972211, 1.000000000000000000),
 ( 1.000000000000000000, 0.9287106072117489175, 1.000000000000000000),
 ( 1.000000000000000000, 0.9267422912951360781, 1.000000000000000000),
 ( 1.000000000000000000, 0.9239539123014891553, 1.000000000000000000),
 ( 1.000000000000000000, 0.9231338493909951870, 1.000000000000000000),
 ( 1.000000000000000000, 0.9228496048506062976, 1.000000000000000000),
 ( 1.000000000000000000, 0.9229135694615097085, 1.000000000000000000),
 ( 1.000000000000000000, 0.9233494155302127693, 1.000000000000000000),
 ( 1.000000000000000000, 0.9237209353787610988, 1.000000000000000000),
 ( 1.000000000000000000, 0.9252744993865242851, 1.000000000000000000),
 ( 1.000000000000000000, 0.9268968421605615626, 1.000000000000000000),
 ( 1.000000000000000000, 0.9311673748452381494, 1.000000000000000000),
 ( 1.000000000000000000, 0.9338157035272729445, 1.000000000000000000),
 ( 1.000000000000000000, 0.9370733336298818772, 1.000000000000000000),
 ( 1.000000000000000000, 0.9372665829346543687, 1.000000000000000000),
 ( 1.000000000000000000, 0.9375588533504843891, 1.000000000000000000),
 ( 1.000000000000000000, 0.9376566762263829347, 1.000000000000000000),
 ( 1.000000000000000000, 0.9377794499114591176, 1.000000000000000000),
 ( 1.000000000000000000, 0.9378038842964694366, 1.000000000000000000),
 ( 1.000000000000000000, 0.9378536652368906212, 1.000000000000000000),
 ( 1.000000000000000000, 0.9378785472098781772, 1.000000000000000000),
 ( 1.000000000000000000, 0.9379531676447521171, 1.000000000000000000),
 ( 1.000000000000000000, 0.9380028806225367832, 1.000000000000000000),
 ( 1.000000000000000000, 0.9384499917948696535, 1.000000000000000000),
 ( 1.000000000000000000, 0.9388452506063797998, 1.000000000000000000),
 ( 1.000000000000000000, 0.9400245377240861178, 1.000000000000000000),
 ( 1.000000000000000000, 0.9408020798628555781, 1.000000000000000000),
 ( 1.000000000000000000, 0.9431089717075972212, 1.000000000000000000),
 ( 1.000000000000000000, 0.9446123105951095278, 1.000000000000000000),
 ( 1.000000000000000000, 0.9578370004751587397, 1.000000000000000000),
 ( 1.000000000000000000, 0.9674308273347622666, 1.000000000000000000),
 ( 1.000000000000000000, 0.9828254127553104347, 1.000000000000000000),
 ( 1.000000000000000000, 0.9886239107120774472, 1.000000000000000000),
 ( 1.000000000000000000, 0.9967564037641253316, 1.000000000000000000),
 ( 1.000000000000000000, 0.9990872413564623189, 1.000000000000000000),
 ( 1.000000000000000000, 0.9997813423572990965, 1.000000000000000000) ) ) 
 REPRESENTATION_ITEM ( '' )  SURFACE ( )  );
#23219 = FACE_OUTER_BOUND ( 'NONE', #9056, .T. ) ;
#23220 = CARTESIAN_POINT ( 'NONE',  ( 200.0000000000002274, -18.85575486854367355, -2.482946933799725642 ) ) ;
#23221 = AXIS2_PLACEMENT_3D ( 'NONE', #15127, #17251, #2502 ) ;
#23222 = DIRECTION ( 'NONE',  ( 0.000000000000000000, 0.000000000000000000, 1.000000000000000000 ) ) ;
#23223 = CARTESIAN_POINT ( 'NONE',  ( -77.90255099906777048, -8.064892378658553795, -20.29001641120655464 ) ) ;
#23224 = CARTESIAN_POINT ( 'NONE',  ( 184.8905102610680444, 14.79361573936375507, 14.79361573936398067 ) ) ;
#23225 = CARTESIAN_POINT ( 'NONE',  ( -77.55640685876515761, -15.64922766773196905, -15.64922766773223195 ) ) ;
#23226 = CARTESIAN_POINT ( 'NONE',  ( 184.8905102610680444, 2.362515690532070066E-13, -19.07866798485558490 ) ) ;
#23227 = CARTESIAN_POINT ( 'NONE',  ( -96.93773665438786225, -8.190703376741039321, 20.92028269119429496 ) ) ;
#23228 = CARTESIAN_POINT ( 'NONE',  ( -30.26275506840324070, -1.694272468446265112, 0.000000000000000000 ) ) ;
#23229 = CARTESIAN_POINT ( 'NONE',  ( 163.1118516004056573, -37.29075403953139300, -19.27778845539249630 ) ) ;
#23230 = CARTESIAN_POINT ( 'NONE',  ( 199.0061349475965358, 18.46602535085470009, -7.668765344048432908 ) ) ;
#23231 = EDGE_CURVE ( 'NONE', #4265, #17928, #7700, .T. ) ;
#23233 = CARTESIAN_POINT ( 'NONE',  ( 200.0000000000000000, 39.99999999999999289, 20.00000000000007105 ) ) ;
#23232 = CARTESIAN_POINT ( 'NONE',  ( -162.0762913951021176, -27.08623940707584055, -29.48230308784799547 ) ) ;
#23234 = CONICAL_SURFACE ( 'NONE', #277, 20.53474504356812247, 0.7853981633974447263 ) ;
#23235 = CARTESIAN_POINT ( 'NONE',  ( 4.995406935893288214, 15.24977328854832770, 0.000000000000000000 ) ) ;
#23236 = CARTESIAN_POINT ( 'NONE',  ( -192.9588430854690273, -18.05360324515454096, 38.51493924976936967 ) ) ;
#23237 = CARTESIAN_POINT ( 'NONE',  ( 199.9999999999999432, -20.00000000000006750, 0.000000000000000000 ) ) ;
#23238 = VERTEX_POINT ( 'NONE', #1345 ) ;
#23239 = CARTESIAN_POINT ( 'NONE',  ( 22.72189371636348554, -43.05215026464009043, 23.48424859981480495 ) ) ;
#23240 = CARTESIAN_POINT ( 'NONE',  ( -238.4067589809705794, 40.96449428006337001, -40.00000000000002132 ) ) ;
#23241 = DIRECTION ( 'NONE',  ( -1.000000000000000000, 0.000000000000000000, 0.000000000000000000 ) ) ;
#23242 = AXIS2_PLACEMENT_3D ( 'NONE', #12779, #16764, #12915 ) ;
#23243 = VECTOR ( 'NONE', #3738, 1000.000000000000000 ) ;
#23244 = CARTESIAN_POINT ( 'NONE',  ( 146.6084372240433993, 3.800685668858676980, 3.800685668858667210 ) ) ;
#23245 = CARTESIAN_POINT ( 'NONE',  ( -208.1127848780264742, -40.00000000000011369, 15.00245453012655439 ) ) ;
#23246 = CARTESIAN_POINT ( 'NONE',  ( -77.62680886784242773, 21.74967759987069371, 3.755764534306124336 ) ) ;
#23247 = CARTESIAN_POINT ( 'NONE',  ( 23.37394308801976806, -13.80096434448233111, -46.80823611210209378 ) ) ;
#23248 = CARTESIAN_POINT ( 'NONE',  ( 199.0262110011730954, -16.45735938206000171, 11.37817034370231006 ) ) ;
#23249 = CARTESIAN_POINT ( 'NONE',  ( -135.8532207217289738, -6.472252184284280396, 6.472252184284099208 ) ) ;
#23250 = CARTESIAN_POINT ( 'NONE',  ( -86.86493150571051558, -19.77569912838786337, 7.943527260504712473 ) ) ;
#23251 = CARTESIAN_POINT ( 'NONE',  ( -314.0000000000000568, -4.605747634845933236E-14, -20.53474504356812247 ) ) ;
#23252 = CARTESIAN_POINT ( 'NONE',  ( -238.4067589809705794, -0.6820004457913680929, 0.6820004457913170226 ) ) ;
#23253 = CARTESIAN_POINT ( 'NONE',  ( 163.1118516004056573, -2.556006622855449647E-13, 27.26290988616872824 ) ) ;
#23254 = CARTESIAN_POINT ( 'NONE',  ( -208.1127848780265026, -10.60833733269551971, 10.60833733269537049 ) ) ;
#23255 = CARTESIAN_POINT ( 'NONE',  ( -87.02115643451061544, 10.85297647555737299, -18.51269039639787906 ) ) ;
#23256 = CARTESIAN_POINT ( 'NONE',  ( -198.0356074513804572, 17.40982414986501325, -39.15871834505897198 ) ) ;
#23258 = CARTESIAN_POINT ( 'NONE',  ( -86.96347745069644475, 41.18208027870576871, 15.38646221621837107 ) ) ;
#23257 = CARTESIAN_POINT ( 'NONE',  ( 57.59792236341147031, 1.722363176415040886, 1.722363176415060426 ) ) ;
#23259 = CARTESIAN_POINT ( 'NONE',  ( -30.26275506840324070, 1.198031551616724366, -57.76657404653984429 ) ) ;
#23260 = CARTESIAN_POINT ( 'NONE',  ( 91.82158438592158234, 22.79471317813472453, -40.00000000000002132 ) ) ;
#23261 = CARTESIAN_POINT ( 'NONE',  ( -280.0000000000000000, -14.14213562373098831, -14.14213562373098654 ) ) ;
#23262 = AXIS2_PLACEMENT_3D ( 'NONE', #13894, #9510, #23741 ) ;
#23263 = CARTESIAN_POINT ( 'NONE',  ( -213.1075012329537230, -8.703598725189323045E-14, 13.71589010951911902 ) ) ;
#23264 = CARTESIAN_POINT ( 'NONE',  ( -198.0356074513804572, -39.15871834505931304, 17.40982414986437377 ) ) ;
#23265 = CARTESIAN_POINT ( 'NONE',  ( -187.3036811847508716, 46.64553187114688626, -13.75782060302973164 ) ) ;
#23266 = ORIENTED_EDGE ( 'NONE', *, *, #13921, .T. ) ;
#23267 = CARTESIAN_POINT ( 'NONE',  ( -56.48582580120559271, 21.81201906317768291, 21.81201906317777173 ) ) ;
#23268 = CARTESIAN_POINT ( 'NONE',  ( -99.29480781227208297, -20.80016781325152664, -8.165122821357817529 ) ) ;
#23269 = CARTESIAN_POINT ( 'NONE',  ( 0.2972598230769923355, 18.14793986248697166, 38.42060263243675422 ) ) ;
#23270 = CARTESIAN_POINT ( 'NONE',  ( -16.37606550806730610, -39.75508062642441587, -16.46709356883193109 ) ) ;
#23271 = ORIENTED_EDGE ( 'NONE', *, *, #2567, .T. ) ;
#23272 = CARTESIAN_POINT ( 'NONE',  ( -166.3490444791802929, -36.43931842067700444, 19.13701437385558535 ) ) ;
#23273 = CARTESIAN_POINT ( 'NONE',  ( 200.0000000000000000, 2.939587388390868306, -18.77290383772223592 ) ) ;
#23274 = CARTESIAN_POINT ( 'NONE',  ( 23.54890483848385330, -23.30407993985125259, 42.80335737019169073 ) ) ;
#23275 = CARTESIAN_POINT ( 'NONE',  ( 170.2234770963711128, -24.55285855007184281, -40.00000000000002132 ) ) ;
#23276 = CARTESIAN_POINT ( 'NONE',  ( 44.65795722941690116, 15.21593185910654000, -36.73450905838434721 ) ) ;
#23277 = CARTESIAN_POINT ( 'NONE',  ( 199.0089741461167989, 19.95552976068599804, 1.321036586804004820 ) ) ;
#23278 = CARTESIAN_POINT ( 'NONE',  ( -56.48582580120559982, -21.81201906317804173, 34.75652343174591152 ) ) ;
#23279 = CARTESIAN_POINT ( 'NONE',  ( 163.1118516004056573, 40.00000000000014921, -27.26290988616858968 ) ) ;
#23280 = FACE_BOUND ( 'NONE', #6243, .T. ) ;
#23281 = CARTESIAN_POINT ( 'NONE',  ( -200.0000000000000853, -24.82633483071228753, -44.86878812508721381 ) ) ;
#23282 = CARTESIAN_POINT ( 'NONE',  ( 146.6084372240433709, -5.374981219216942385, -40.00000000000002132 ) ) ;
#23284 = CARTESIAN_POINT ( 'NONE',  ( -600.2449649317687772, 37.61268920114236636, 13.74386906026104249 ) ) ;
#23283 = CARTESIAN_POINT ( 'NONE',  ( 22.75856136761844795, -17.88529938203868497, -43.17893233522190144 ) ) ;
#23285 = CARTESIAN_POINT ( 'NONE',  ( -208.1127848780264742, -15.00245453012673202, 40.00000000000002132 ) ) ;
#23286 = CARTESIAN_POINT ( 'NONE',  ( 0.2972598230769923355, 18.14793986248697166, 38.42060263243675422 ) ) ;
#23287 = CARTESIAN_POINT ( 'NONE',  ( 0.2972598230769956662, 40.00000000000058975, -54.33493731733894094 ) ) ;
#23288 = CARTESIAN_POINT ( 'NONE',  ( -114.4364955367327354, 8.644468109209578088, -20.04994829327644723 ) ) ;
#23289 = CARTESIAN_POINT ( 'NONE',  ( -135.8532207217289738, -40.00000000000014211, 9.153146818113153671 ) ) ;
#23290 = CARTESIAN_POINT ( 'NONE',  ( 199.0258842571097375, -9.142960865851959440, 17.79628948870135829 ) ) ;
#23291 = CARTESIAN_POINT ( 'NONE',  ( 164.1121284987796969, -24.38383377897543980, -10.10011465390285323 ) ) ;
#23292 = CARTESIAN_POINT ( 'NONE',  ( -280.0000000000000568, 14.14213562373038968, 42.42640687119305198 ) ) ;
#23293 = CARTESIAN_POINT ( 'NONE',  ( -198.0356074513804572, -10.87444709760996986, 67.44298959253333692 ) ) ;
#23294 = ORIENTED_EDGE ( 'NONE', *, *, #25019, .F. ) ;
#23296 = CARTESIAN_POINT ( 'NONE',  ( -4.915070467874492088, 46.68718905935151753, -13.76630780994186765 ) ) ;
#23295 = CARTESIAN_POINT ( 'NONE',  ( -350.0000000000001137, -4.857225732735059864E-14, 0.000000000000000000 ) ) ;
#23297 = CARTESIAN_POINT ( 'NONE',  ( 91.82158438592156813, 17.20528682183302038, 40.00000000000002132 ) ) ;
#23298 = CARTESIAN_POINT ( 'NONE',  ( -317.0000000000000568, -4.467814962633844109E-14, 31.79780246617542616 ) ) ;
#23299 = CARTESIAN_POINT ( 'NONE',  ( -200.4317933031551320, 49.29858032309928717, -14.17468109412842914 ) ) ;
#23300 = DIRECTION ( 'NONE',  ( 1.000000000000000000, 0.000000000000000000, 0.000000000000000000 ) ) ;
#23301 = ORIENTED_EDGE ( 'NONE', *, *, #9941, .T. ) ;
#23302 = ORIENTED_EDGE ( 'NONE', *, *, #23310, .F. ) ;
#23303 = CARTESIAN_POINT ( 'NONE',  ( 0.2972598230769976091, -10.13633138497479180, 10.13633138497468522 ) ) ;
#23304 = CARTESIAN_POINT ( 'NONE',  ( -210.0000000000000284, 52.49999999999988631, -82.49999999999998579 ) ) ;
#23305 = CARTESIAN_POINT ( 'NONE',  ( 146.6084372240433993, 1.478241399363601114E-13, -34.62501878078305850 ) ) ;
#23306 = EDGE_CURVE ( 'NONE', #14180, #11718, #16163, .T. ) ;
#23307 = VERTEX_POINT ( 'NONE', #13438 ) ;
#23308 = CARTESIAN_POINT ( 'NONE',  ( 199.9999999999998579, 2.934899133129863280, 18.78102297366244500 ) ) ;
#23309 = DIRECTION ( 'NONE',  ( 0.000000000000000000, -1.000000000000000000, 0.000000000000000000 ) ) ;
#23310 = EDGE_CURVE ( 'NONE', #11587, #17229, #10150, .T. ) ;
#23311 = CARTESIAN_POINT ( 'NONE',  ( 91.82158438592158234, -12.16597498400057198, 44.40256751092329779 ) ) ;
#23312 = CARTESIAN_POINT ( 'NONE',  ( -716.9846540392142060, -66.50000000000001421, 66.50000000000005684 ) ) ;
#23313 = CARTESIAN_POINT ( 'NONE',  ( 0.2972598230769956662, 39.99999999999983658, 54.33493731733950938 ) ) ;
#23314 = CYLINDRICAL_SURFACE ( 'NONE', #8774, 5.000000000000004441 ) ;
#23315 = EDGE_CURVE ( 'NONE', #15801, #1596, #1470, .T. ) ;
#23316 = EDGE_CURVE ( 'NONE', #13098, #7186, #1250, .T. ) ;
#23317 = DIRECTION ( 'NONE',  ( 1.000000000000000000, 1.303213150798907793E-16, 2.465190328815661892E-32 ) ) ;
#23318 = CARTESIAN_POINT ( 'NONE',  ( 19.06497207195982924, -39.99999999999945288, -54.19242893257885640 ) ) ;
#23319 = CARTESIAN_POINT ( 'NONE',  ( 130.8568914410475372, 8.880724697947696879E-14, -5.949712681206690945 ) ) ;
#23320 = CARTESIAN_POINT ( 'NONE',  ( 14.38125909742181285, -10.73282306404727393, 10.73282306404716380 ) ) ;
#23321 = LINE ( 'NONE', #17317, #13978 ) ;
#23322 = CARTESIAN_POINT ( 'NONE',  ( -200.4317933031552457, 14.17468109412838295, 49.29858032309917348 ) ) ;
#23323 = CYLINDRICAL_SURFACE ( 'NONE', #14263, 30.00000000000000355 ) ;
#23324 = AXIS2_PLACEMENT_3D ( 'NONE', #18049, #3834, #3695 ) ;
#23325 = CARTESIAN_POINT ( 'NONE',  ( 210.0000000000000284, 71.50000000000009948, -66.50000000000005684 ) ) ;
#23326 = FACE_OUTER_BOUND ( 'NONE', #3356, .T. ) ;
#23327 = CARTESIAN_POINT ( 'NONE',  ( -82.25678930351507745, -16.86921253968544221, 11.09265870503258000 ) ) ;
#23328 =( BOUNDED_SURFACE ( )  B_SPLINE_SURFACE ( 3, 3, ( 
 ( #17995, #20002, #9892, #11132, #17242, #8874, #22717, #18991, #23249, #22854, #6475, #13002, #20854, #25120, #10605, #14852, #10743, #18717, #2767, #10876, #13131, #6872, #4494, #14589, #12597, #14986, #14722, #4629, #22988, #18854 ),
 ( #4893, #634, #502, #6602, #24850, #20726, #23120, #8609, #2634, #21250, #2494, #19116, #16718, #12732, #12868, #8740, #16858, #5024, #24989, #6997, #21122, #768, #15118, #6740, #4764, #3025, #16984, #19246, #20986, #1028 ),
 ( #2900, #11006, #899, #9010, #17116, #25246, #9127, #25686, #12206, #9942, #18050, #5685, #26203, #20327, #17784, #7939, #1705, #16057, #20064, #24048, #12071, #5825, #13789, #13927, #10078, #6219, #3835, #25929, #11937, #1840 ),
 ( #22199, #24327, #14066, #5957, #3974, #2104, #4107, #17918, #24183, #22063, #20190, #14332, #22330, #23909, #10213, #1972, #15914, #21925, #1575, #18318, #4243, #18183, #26333, #8074, #9678, #101, #16193, #9813, #6091, #14198 ),
 ( #8208, #16326, #24454, #7669, #3697, #22463, #12333, #15782, #11802, #26061, #19922, #7799, #2773, #4770, #20732, #18860, #16863, #229, #6481, #12602, #14464, #4499, #2500, #8880, #2364, #10611, #4372, #8343, #12875, #6876 ),
 ( #774, #20858, #10343, #4899, #18453, #2641, #10478, #18592, #18723, #14593, #507, #20589, #10749, #16991, #12738, #370, #24588, #25126, #8613, #16464, #20991, #16724, #24855, #6607, #14727, #22859, #6748, #14992, #6344, #20461 ),
 ( #641, #4636, #10883, #22595, #12462, #18997, #8745, #23127, #8474, #2235, #16592, #24724, #24995, #22722, #14860, #22994, #15379, #3280, #3156, #23502, #11137, #2905, #1415, #9267, #23382, #7137, #19631, #19499, #5156, #5276 ) ),
 .UNSPECIFIED., .T., .F., .T. ) 
 B_SPLINE_SURFACE_WITH_KNOTS ( ( 4, 3, 4 ),
 ( 4, 2, 2, 2, 2, 2, 2, 2, 2, 2, 2, 2, 2, 2, 4 ),
 ( 0.000000000000000000, 0.5000000000000000000, 1.000000000000000000 ),
 ( 0.000000000000000000, 0.1357259735107005372, 0.1651108541090157700, 0.1944957347073310028, 0.3598804999793158710, 0.3867117631979620773, 0.4135430264166082281, 0.5789277916885930964, 0.6062785021374117456, 0.6336292125862302838, 0.8508620842112317728, 0.8814014469398914198, 0.9119408096685510667, 0.9559704048342755334, 1.000000000000000000 ),
 .UNSPECIFIED. ) 
 GEOMETRIC_REPRESENTATION_ITEM ( )  RATIONAL_B_SPLINE_SURFACE ( (
 ( 1.000000000000000000, 1.000000000000000000, 1.000000000000000000, 1.000000000000000000, 1.000000000000000000, 1.000000000000000000, 1.000000000000000000, 1.000000000000000000, 1.000000000000000000, 1.000000000000000000, 1.000000000000000000, 1.000000000000000000, 1.000000000000000000, 1.000000000000000000, 1.000000000000000000, 1.000000000000000000, 1.000000000000000000, 1.000000000000000000, 1.000000000000000000, 1.000000000000000000, 1.000000000000000000, 1.000000000000000000, 1.000000000000000000, 1.000000000000000000, 1.000000000000000000, 1.000000000000000000, 1.000000000000000000, 1.000000000000000000, 1.000000000000000000, 1.000000000000000000),
 ( 0.3333333333333333703, 0.3333333333333333703, 0.3333333333333333703, 0.3333333333333333703, 0.3333333333333333703, 0.3333333333333333703, 0.3333333333333333703, 0.3333333333333333703, 0.3333333333333333703, 0.3333333333333333703, 0.3333333333333333703, 0.3333333333333333703, 0.3333333333333333703, 0.3333333333333333703, 0.3333333333333333703, 0.3333333333333333703, 0.3333333333333333703, 0.3333333333333333703, 0.3333333333333333703, 0.3333333333333333703, 0.3333333333333333703, 0.3333333333333333703, 0.3333333333333333703, 0.3333333333333333703, 0.3333333333333333703, 0.3333333333333333703, 0.3333333333333333703, 0.3333333333333333703, 0.3333333333333333703, 0.3333333333333333703),
 ( 0.3333333333333333703, 0.3333333333333333703, 0.3333333333333333703, 0.3333333333333333703, 0.3333333333333333703, 0.3333333333333333703, 0.3333333333333333703, 0.3333333333333333703, 0.3333333333333333703, 0.3333333333333333703, 0.3333333333333333703, 0.3333333333333333703, 0.3333333333333333703, 0.3333333333333333703, 0.3333333333333333703, 0.3333333333333333703, 0.3333333333333333703, 0.3333333333333333703, 0.3333333333333333703, 0.3333333333333333703, 0.3333333333333333703, 0.3333333333333333703, 0.3333333333333333703, 0.3333333333333333703, 0.3333333333333333703, 0.3333333333333333703, 0.3333333333333333703, 0.3333333333333333703, 0.3333333333333333703, 0.3333333333333333703),
 ( 1.000000000000000000, 1.000000000000000000, 1.000000000000000000, 1.000000000000000000, 1.000000000000000000, 1.000000000000000000, 1.000000000000000000, 1.000000000000000000, 1.000000000000000000, 1.000000000000000000, 1.000000000000000000, 1.000000000000000000, 1.000000000000000000, 1.000000000000000000, 1.000000000000000000, 1.000000000000000000, 1.000000000000000000, 1.000000000000000000, 1.000000000000000000, 1.000000000000000000, 1.000000000000000000, 1.000000000000000000, 1.000000000000000000, 1.000000000000000000, 1.000000000000000000, 1.000000000000000000, 1.000000000000000000, 1.000000000000000000, 1.000000000000000000, 1.000000000000000000),
 ( 0.3333333333333333703, 0.3333333333333333703, 0.3333333333333333703, 0.3333333333333333703, 0.3333333333333333703, 0.3333333333333333703, 0.3333333333333333703, 0.3333333333333333703, 0.3333333333333333703, 0.3333333333333333703, 0.3333333333333333703, 0.3333333333333333703, 0.3333333333333333703, 0.3333333333333333703, 0.3333333333333333703, 0.3333333333333333703, 0.3333333333333333703, 0.3333333333333333703, 0.3333333333333333703, 0.3333333333333333703, 0.3333333333333333703, 0.3333333333333333703, 0.3333333333333333703, 0.3333333333333333703, 0.3333333333333333703, 0.3333333333333333703, 0.3333333333333333703, 0.3333333333333333703, 0.3333333333333333703, 0.3333333333333333703),
 ( 0.3333333333333333703, 0.3333333333333333703, 0.3333333333333333703, 0.3333333333333333703, 0.3333333333333333703, 0.3333333333333333703, 0.3333333333333333703, 0.3333333333333333703, 0.3333333333333333703, 0.3333333333333333703, 0.3333333333333333703, 0.3333333333333333703, 0.3333333333333333703, 0.3333333333333333703, 0.3333333333333333703, 0.3333333333333333703, 0.3333333333333333703, 0.3333333333333333703, 0.3333333333333333703, 0.3333333333333333703, 0.3333333333333333703, 0.3333333333333333703, 0.3333333333333333703, 0.3333333333333333703, 0.3333333333333333703, 0.3333333333333333703, 0.3333333333333333703, 0.3333333333333333703, 0.3333333333333333703, 0.3333333333333333703),
 ( 1.000000000000000000, 1.000000000000000000, 1.000000000000000000, 1.000000000000000000, 1.000000000000000000, 1.000000000000000000, 1.000000000000000000, 1.000000000000000000, 1.000000000000000000, 1.000000000000000000, 1.000000000000000000, 1.000000000000000000, 1.000000000000000000, 1.000000000000000000, 1.000000000000000000, 1.000000000000000000, 1.000000000000000000, 1.000000000000000000, 1.000000000000000000, 1.000000000000000000, 1.000000000000000000, 1.000000000000000000, 1.000000000000000000, 1.000000000000000000, 1.000000000000000000, 1.000000000000000000, 1.000000000000000000, 1.000000000000000000, 1.000000000000000000, 1.000000000000000000) ) ) 
 REPRESENTATION_ITEM ( '' )  SURFACE ( )  );
#23329 = CARTESIAN_POINT ( 'NONE',  ( 200.0000000000000000, -42.42640687119290988, 14.14213562373064903 ) ) ;
#23330 = CARTESIAN_POINT ( 'NONE',  ( -631.8022509310842452, 28.60468924217828857, -34.74645141880154142 ) ) ;
#23331 = CARTESIAN_POINT ( 'NONE',  ( -726.9846540392142060, 4.898587196589404348E-15, 39.99999999999991473 ) ) ;
#23332 = VERTEX_POINT ( 'NONE', #9321 ) ;
#23333 = CARTESIAN_POINT ( 'NONE',  ( -91.56559293963834989, -16.03295912088659492, -40.53558337403696044 ) ) ;
#23334 = CARTESIAN_POINT ( 'NONE',  ( 200.0000000000000000, -52.49999999999970868, 82.49999999999998579 ) ) ;
#23335 = DIRECTION ( 'NONE',  ( 0.000000000000000000, 0.000000000000000000, 1.000000000000000000 ) ) ;
#23336 = ORIENTED_EDGE ( 'NONE', *, *, #379, .F. ) ;
#23337 = CARTESIAN_POINT ( 'NONE',  ( 91.82158438592158234, 2.580785920671402147E-13, -22.79471317813470321 ) ) ;
#23338 = CARTESIAN_POINT ( 'NONE',  ( 199.0199226726568895, -18.44042569010415633, -7.747917312412542223 ) ) ;
#23339 = DIRECTION ( 'NONE',  ( -1.000000000000000000, 0.000000000000000000, 0.000000000000000000 ) ) ;
#23340 = ORIENTED_EDGE ( 'NONE', *, *, #22659, .F. ) ;
#23341 = ORIENTED_EDGE ( 'NONE', *, *, #10932, .T. ) ;
#23342 = CARTESIAN_POINT ( 'NONE',  ( 163.1118516004056573, 12.73709011382478273, 2.449293598294708485E-15 ) ) ;
#23343 = CARTESIAN_POINT ( 'NONE',  ( -100.0957100001013913, -20.56213589528242736, -8.517115559121256396 ) ) ;
#23344 = AXIS2_PLACEMENT_3D ( 'NONE', #20963, #10986, #2744 ) ;
#23345 = PRODUCT_DEFINITION_CONTEXT ( 'detailed design', #24315, 'design' ) ;
#23346 = AXIS2_PLACEMENT_3D ( 'NONE', #23570, #17321, #3100 ) ;
#23347 = CARTESIAN_POINT ( 'NONE',  ( -138.9613193425336988, -10.11110876495216537, 29.42718875726419014 ) ) ;
#23348 = CARTESIAN_POINT ( 'NONE',  ( -198.0356074513804572, -9.007331120208026888E-14, 15.37879056873070560 ) ) ;
#23349 = CARTESIAN_POINT ( 'NONE',  ( 199.9999999999998863, -17.04947422730185025, -8.406841951002201441 ) ) ;
#23350 = CARTESIAN_POINT ( 'NONE',  ( -77.78738561284504271, 9.951797149076110571, 19.58913667614457310 ) ) ;
#23351 = CARTESIAN_POINT ( 'NONE',  ( 57.59792236341147031, -1.722363176415055985, 1.722363176415024677 ) ) ;
#23352 = CARTESIAN_POINT ( 'NONE',  ( -213.1075012329537230, -9.698598906462304825, -66.26714140138675191 ) ) ;
#23353 = CARTESIAN_POINT ( 'NONE',  ( -114.7826396787322665, -15.64922767586157981, -15.64922767586183383 ) ) ;
#23354 = CARTESIAN_POINT ( 'NONE',  ( 146.6084372240433993, 8.568076647504290689E-14, -5.374981219216972583 ) ) ;
#23355 = DIRECTION ( 'NONE',  ( 1.000000000000000000, 1.836970198721030181E-16, 0.000000000000000000 ) ) ;
#23356 = CARTESIAN_POINT ( 'NONE',  ( 163.1118516004056573, 27.26290988616876021, -40.00000000000002132 ) ) ;
#23357 = CARTESIAN_POINT ( 'NONE',  ( 19.06497207195982924, -66.60410523465823474, 10.03556273973400081 ) ) ;
#23358 = CARTESIAN_POINT ( 'NONE',  ( 192.4448373802101173, 20.00000000003945644, -40.00000000000002132 ) ) ;
#23360 = CARTESIAN_POINT ( 'NONE',  ( -105.3755690713226585, 40.00000000000007816, -21.75974354311636461 ) ) ;
#23359 = CARTESIAN_POINT ( 'NONE',  ( -30.26275506840324070, -27.08623969584554558, -29.48230279907826912 ) ) ;
#23361 = CARTESIAN_POINT ( 'NONE',  ( 151.7948205124836534, -33.23291073765550863, -40.00000000000002132 ) ) ;
#23362 = CARTESIAN_POINT ( 'NONE',  ( 14.38125909742181285, -17.55144818341476309, 39.01709431150910490 ) ) ;
#23363 = CARTESIAN_POINT ( 'NONE',  ( 151.7948205124836250, 6.767089262349059275, 2.449293598294708485E-15 ) ) ;
#23364 = ORIENTED_EDGE ( 'NONE', *, *, #21498, .T. ) ;
#23365 = VECTOR ( 'NONE', #3036, 1000.000000000000000 ) ;
#23366 = CARTESIAN_POINT ( 'NONE',  ( -4.004886986944963922, -47.00296421444941330, 13.82996668233338156 ) ) ;
#23367 = CARTESIAN_POINT ( 'NONE',  ( -162.0762913951020892, 41.69427287692678163, -40.00000000000002132 ) ) ;
#23368 = CARTESIAN_POINT ( 'NONE',  ( -87.10563802237723507, -13.14174799571811825, 16.99650074895399854 ) ) ;
#23369 =( BOUNDED_SURFACE ( )  B_SPLINE_SURFACE ( 3, 3, ( 
 ( #3678, #3413, #22180, #13515, #19640, #9524, #1823, #5804, #22046, #18167, #7649, #5413, #15763, #26182, #8057, #5939, #5668, #13774, #11786, #1690, #16038, #18031, #23634, #19906, #25774, #9794, #7525, #15633, #23758, #5539 ),
 ( #13645, #17897, #26045, #7782, #20574, #2219, #12446, #24570, #14312, #8455, #2346, #18704, #10458, #22704, #8594, #351, #4480, #6075, #4088, #20310, #487, #12581, #24433, #212, #12188, #20442, #16704, #16574, #24836, #18571 ),
 ( #10328, #24705, #18437, #6459, #16173, #8321, #14177, #2087, #10589, #12315, #24308, #22312, #20711, #14575, #18297, #2477, #16309, #10194, #83, #8193, #6200, #22446, #4226, #16446, #6326, #14448, #22575, #4353, #19820, #21956 ),
 ( #4143, #133, #14098, #26095, #11695, #9709, #21819, #7969, #2134, #26235, #11970, #7831, #8237, #20094, #1873, #1606, #9844, #17814, #16355, #3730, #13960, #17948, #22366, #13696, #9976, #19951, #12235, #5717, #20359, #15949 ),
 ( #10242, #11833, #3868, #25960, #24080, #18353, #10110, #5590, #5989, #22227, #1943, #18084, #4003, #1735, #3590, #7703, #14227, #15814, #8105, #23940, #12102, #13822, #16088, #20226, #5854, #22094, #24218, #2004, #18211, #16226 ),
 ( #24355, #6119, #16620, #10643, #8372, #25017, #6373, #534, #22493, #8639, #8903, #23022, #19020, #6637, #18620, #4272, #2264, #14363, #16749, #21014, #18751, #4531, #403, #799, #12629, #20756, #12360, #2394, #10372, #24488 ),
 ( #20491, #8772, #10908, #18482, #263, #12899, #6250, #24881, #4660, #22624, #10506, #22752, #12493, #20888, #16494, #2796, #20618, #8506, #6771, #12763, #24619, #2526, #18885, #14491, #14751, #22882, #14883, #4399, #24753, #10772 ) ),
 .UNSPECIFIED., .T., .F., .F. ) 
 B_SPLINE_SURFACE_WITH_KNOTS ( ( 4, 3, 4 ),
 ( 4, 2, 2, 2, 2, 2, 2, 2, 2, 2, 2, 2, 2, 2, 4 ),
 ( 0.000000000000000000, 0.5000000000000000000, 1.000000000000000000 ),
 ( 0.000000000000000000, 0.1357259735107005372, 0.1651108541090157700, 0.1944957347073310028, 0.3598804999793158710, 0.3867117631979620773, 0.4135430264166082281, 0.5789277916885930964, 0.6062785021374117456, 0.6336292125862302838, 0.8508620842112317728, 0.8814014469398914198, 0.9119408096685510667, 0.9559704048342755334, 1.000000000000000000 ),
 .UNSPECIFIED. ) 
 GEOMETRIC_REPRESENTATION_ITEM ( )  RATIONAL_B_SPLINE_SURFACE ( (
 ( 1.000000000000000000, 1.000000000000000000, 1.000000000000000000, 1.000000000000000000, 1.000000000000000000, 1.000000000000000000, 1.000000000000000000, 1.000000000000000000, 1.000000000000000000, 1.000000000000000000, 1.000000000000000000, 1.000000000000000000, 1.000000000000000000, 1.000000000000000000, 1.000000000000000000, 1.000000000000000000, 1.000000000000000000, 1.000000000000000000, 1.000000000000000000, 1.000000000000000000, 1.000000000000000000, 1.000000000000000000, 1.000000000000000000, 1.000000000000000000, 1.000000000000000000, 1.000000000000000000, 1.000000000000000000, 1.000000000000000000, 1.000000000000000000, 1.000000000000000000),
 ( 0.3333333333333333703, 0.3333333333333333703, 0.3333333333333333703, 0.3333333333333333703, 0.3333333333333333703, 0.3333333333333333703, 0.3333333333333333703, 0.3333333333333333703, 0.3333333333333333703, 0.3333333333333333703, 0.3333333333333333703, 0.3333333333333333703, 0.3333333333333333703, 0.3333333333333333703, 0.3333333333333333703, 0.3333333333333333703, 0.3333333333333333703, 0.3333333333333333703, 0.3333333333333333703, 0.3333333333333333703, 0.3333333333333333703, 0.3333333333333333703, 0.3333333333333333703, 0.3333333333333333703, 0.3333333333333333703, 0.3333333333333333703, 0.3333333333333333703, 0.3333333333333333703, 0.3333333333333333703, 0.3333333333333333703),
 ( 0.3333333333333333703, 0.3333333333333333703, 0.3333333333333333703, 0.3333333333333333703, 0.3333333333333333703, 0.3333333333333333703, 0.3333333333333333703, 0.3333333333333333703, 0.3333333333333333703, 0.3333333333333333703, 0.3333333333333333703, 0.3333333333333333703, 0.3333333333333333703, 0.3333333333333333703, 0.3333333333333333703, 0.3333333333333333703, 0.3333333333333333703, 0.3333333333333333703, 0.3333333333333333703, 0.3333333333333333703, 0.3333333333333333703, 0.3333333333333333703, 0.3333333333333333703, 0.3333333333333333703, 0.3333333333333333703, 0.3333333333333333703, 0.3333333333333333703, 0.3333333333333333703, 0.3333333333333333703, 0.3333333333333333703),
 ( 1.000000000000000000, 1.000000000000000000, 1.000000000000000000, 1.000000000000000000, 1.000000000000000000, 1.000000000000000000, 1.000000000000000000, 1.000000000000000000, 1.000000000000000000, 1.000000000000000000, 1.000000000000000000, 1.000000000000000000, 1.000000000000000000, 1.000000000000000000, 1.000000000000000000, 1.000000000000000000, 1.000000000000000000, 1.000000000000000000, 1.000000000000000000, 1.000000000000000000, 1.000000000000000000, 1.000000000000000000, 1.000000000000000000, 1.000000000000000000, 1.000000000000000000, 1.000000000000000000, 1.000000000000000000, 1.000000000000000000, 1.000000000000000000, 1.000000000000000000),
 ( 0.3333333333333333703, 0.3333333333333333703, 0.3333333333333333703, 0.3333333333333333703, 0.3333333333333333703, 0.3333333333333333703, 0.3333333333333333703, 0.3333333333333333703, 0.3333333333333333703, 0.3333333333333333703, 0.3333333333333333703, 0.3333333333333333703, 0.3333333333333333703, 0.3333333333333333703, 0.3333333333333333703, 0.3333333333333333703, 0.3333333333333333703, 0.3333333333333333703, 0.3333333333333333703, 0.3333333333333333703, 0.3333333333333333703, 0.3333333333333333703, 0.3333333333333333703, 0.3333333333333333703, 0.3333333333333333703, 0.3333333333333333703, 0.3333333333333333703, 0.3333333333333333703, 0.3333333333333333703, 0.3333333333333333703),
 ( 0.3333333333333333703, 0.3333333333333333703, 0.3333333333333333703, 0.3333333333333333703, 0.3333333333333333703, 0.3333333333333333703, 0.3333333333333333703, 0.3333333333333333703, 0.3333333333333333703, 0.3333333333333333703, 0.3333333333333333703, 0.3333333333333333703, 0.3333333333333333703, 0.3333333333333333703, 0.3333333333333333703, 0.3333333333333333703, 0.3333333333333333703, 0.3333333333333333703, 0.3333333333333333703, 0.3333333333333333703, 0.3333333333333333703, 0.3333333333333333703, 0.3333333333333333703, 0.3333333333333333703, 0.3333333333333333703, 0.3333333333333333703, 0.3333333333333333703, 0.3333333333333333703, 0.3333333333333333703, 0.3333333333333333703),
 ( 1.000000000000000000, 1.000000000000000000, 1.000000000000000000, 1.000000000000000000, 1.000000000000000000, 1.000000000000000000, 1.000000000000000000, 1.000000000000000000, 1.000000000000000000, 1.000000000000000000, 1.000000000000000000, 1.000000000000000000, 1.000000000000000000, 1.000000000000000000, 1.000000000000000000, 1.000000000000000000, 1.000000000000000000, 1.000000000000000000, 1.000000000000000000, 1.000000000000000000, 1.000000000000000000, 1.000000000000000000, 1.000000000000000000, 1.000000000000000000, 1.000000000000000000, 1.000000000000000000, 1.000000000000000000, 1.000000000000000000, 1.000000000000000000, 1.000000000000000000) ) ) 
 REPRESENTATION_ITEM ( '' )  SURFACE ( )  );
#23370 = CARTESIAN_POINT ( 'NONE',  ( -100.7734535825088500, -16.03295912088716335, 40.53558337403673306 ) ) ;
#23371 = CARTESIAN_POINT ( 'NONE',  ( -100.7734535825088358, 6.065416334915073333E-14, -22.67402823373191723 ) ) ;
#23372 = DIRECTION ( 'NONE',  ( 1.000000000000000000, -0.000000000000000000, -0.000000000000000000 ) ) ;
#23373 = CARTESIAN_POINT ( 'NONE',  ( -8.255580677153719904, 13.52904896325820339, -45.52720393890008665 ) ) ;
#23374 = CARTESIAN_POINT ( 'NONE',  ( 199.9999999999999432, -7.567711247534615993, 17.44155761536767812 ) ) ;
#23375 = EDGE_CURVE ( 'NONE', #12261, #3577, #18149, .T. ) ;
#23376 = CARTESIAN_POINT ( 'NONE',  ( -649.6854717427950163, 34.86078069656281286, -19.61884895816823260 ) ) ;
#23377 = CARTESIAN_POINT ( 'NONE',  ( -77.58512834294195670, -2.776851935584524256, -21.97396063739902061 ) ) ;
#23378 = CARTESIAN_POINT ( 'NONE',  ( 0.2972598230769886718, 38.42060263243643448, 18.14793986248763957 ) ) ;
#23379 = CARTESIAN_POINT ( 'NONE',  ( -91.56559293963836410, 44.31723036834908669, -12.25131212657445801 ) ) ;
#23380 = COLOUR_RGB ( '',0.7921568627450980005, 0.8196078431372548767, 0.9333333333333333481 ) ;
#23381 = CARTESIAN_POINT ( 'NONE',  ( 91.82158438592159655, 12.16597498400028776, 44.40256751092339016 ) ) ;
#23382 = CARTESIAN_POINT ( 'NONE',  ( 151.7948205124836250, -23.49921654116371883, 23.49921654116317526 ) ) ;
#23383 = CARTESIAN_POINT ( 'NONE',  ( -208.1127848780264742, 17.67593391476678377, -38.89260858015718014 ) ) ;
#23385 = CARTESIAN_POINT ( 'NONE',  ( -91.56559293963834989, -44.31723036834885932, -12.25131212657538171 ) ) ;
#23384 = CARTESIAN_POINT ( 'NONE',  ( 136.1360204305621266, 53.05693388239320285, -3.511608612530223716 ) ) ;
#23386 = CARTESIAN_POINT ( 'NONE',  ( -259.2033419157646676, 21.55415060305860209, -21.55415060305812602 ) ) ;
#23387 = CARTESIAN_POINT ( 'NONE',  ( -105.3755690713226585, -21.75974354311652448, -40.00000000000002132 ) ) ;
#23388 = DIRECTION ( 'NONE',  ( 0.000000000000000000, 0.000000000000000000, 1.000000000000000000 ) ) ;
#23389 = CARTESIAN_POINT ( 'NONE',  ( -86.96347745069644475, 5.999880687339585546E-14, -21.75974354311649961 ) ) ;
#23390 = CARTESIAN_POINT ( 'NONE',  ( 170.2234770963711128, -39.20704971665404059, 17.36149277826957160 ) ) ;
#23391 = FACE_OUTER_BOUND ( 'NONE', #15807, .T. ) ;
#23392 = ORIENTED_EDGE ( 'NONE', *, *, #22256, .F. ) ;
#23393 = CARTESIAN_POINT ( 'NONE',  ( 14.38125909742181108, 39.01709431150907648, 39.01709431150921858 ) ) ;
#23394 = CARTESIAN_POINT ( 'NONE',  ( -196.0240759113457045, 24.63338926175158861, 44.60678620512894099 ) ) ;
#23395 = CARTESIAN_POINT ( 'NONE',  ( 9.006212071497531113, 24.85331907609986501, 44.90541342374595501 ) ) ;
#23396 = CARTESIAN_POINT ( 'NONE',  ( -16.87994666116949460, -39.19724034060761397, -20.93785811911747530 ) ) ;
#23397 = ORIENTED_EDGE ( 'NONE', *, *, #306, .T. ) ;
#23398 = CARTESIAN_POINT ( 'NONE',  ( -184.9729924864286659, -42.02333070177691354, 22.80024897330345368 ) ) ;
#23399 = CIRCLE ( 'NONE', #11910, 75.00000000000000000 ) ;
#23400 = CARTESIAN_POINT ( 'NONE',  ( 200.0000000000000284, -3.097043465352568248, -18.74877632928372151 ) ) ;
#23401 = CARTESIAN_POINT ( 'NONE',  ( 23.10188454848764650, -23.40120037233781147, 42.94013537404170222 ) ) ;
#23402 = EDGE_CURVE ( 'NONE', #555, #5488, #22930, .T. ) ;
#23403 = CARTESIAN_POINT ( 'NONE',  ( 73.43374752933530658, 26.88866000079776342, -12.96823637283455355 ) ) ;
#23404 = CARTESIAN_POINT ( 'NONE',  ( 199.0053210531128229, 14.60061869579413063, -13.67646033072836786 ) ) ;
#23405 = CARTESIAN_POINT ( 'NONE',  ( -86.94483050222758891, 20.27470715367157794, 6.877769850676278551 ) ) ;
#23406 = CARTESIAN_POINT ( 'NONE',  ( -30.26275506840324070, -1.147469862568086380E-14, 1.694272468446259783 ) ) ;
#23407 = CARTESIAN_POINT ( 'NONE',  ( -86.95456146551094889, -6.703401383518407641, 20.33691291319591699 ) ) ;
#23408 = CARTESIAN_POINT ( 'NONE',  ( -210.0000000000000284, 52.50000000000007816, -52.49999999999999289 ) ) ;
#23409 = CARTESIAN_POINT ( 'NONE',  ( 130.8568914410475088, -5.949712681206664300, -40.00000000000002132 ) ) ;
#23411 = CARTESIAN_POINT ( 'NONE',  ( -624.9082308837247410, 26.45751311064576683, -30.00000000000002842 ) ) ;
#23410 = CARTESIAN_POINT ( 'NONE',  ( 23.35901252181223597, -13.80180065670210432, -46.81387818480128260 ) ) ;
#23412 = CARTESIAN_POINT ( 'NONE',  ( 4.995406935893309530, -55.24977328856464709, 40.00000000000002132 ) ) ;
#23413 = CARTESIAN_POINT ( 'NONE',  ( -100.7734535825088500, 44.31723036834890905, 12.25131212657507795 ) ) ;
#23414 = CIRCLE ( 'NONE', #15744, 5.000000000000004441 ) ;
#23415 = CARTESIAN_POINT ( 'NONE',  ( 19.06497207195979726, 40.00000000000017053, -14.19242893257798599 ) ) ;
#23416 = CARTESIAN_POINT ( 'NONE',  ( -30.26275506840324070, -40.00000000000001421, -1.694272468446678559 ) ) ;
#23417 = CARTESIAN_POINT ( 'NONE',  ( -626.9846540392142060, 90.00000000000000000, -60.00000000000000000 ) ) ;
#23418 = CARTESIAN_POINT ( 'NONE',  ( -135.8532207217289738, 21.81201906317729566, 34.75652343174635917 ) ) ;
#23419 = ORIENTED_EDGE ( 'NONE', *, *, #3969, .T. ) ;
#23421 = CARTESIAN_POINT ( 'NONE',  ( -0.5869797817588224831, 43.96874597319774836, -18.21245090264383393 ) ) ;
#23420 = CARTESIAN_POINT ( 'NONE',  ( -77.56334768864770979, 1.373422545953698615, -22.09347816142257059 ) ) ;
#23422 = CARTESIAN_POINT ( 'NONE',  ( 200.0000000000000000, -19.99999999999989342, 40.00000000000002132 ) ) ;
#23423 = CARTESIAN_POINT ( 'NONE',  ( -189.1288337602927641, 43.24060467048765588, -23.62383291543576647 ) ) ;
#23424 = VERTEX_POINT ( 'NONE', #17309 ) ;
#23425 = ORIENTED_EDGE ( 'NONE', *, *, #15144, .T. ) ;
#23426 = CARTESIAN_POINT ( 'NONE',  ( 91.82158438592158234, 12.16597498397773869, -12.16597498397759303 ) ) ;
#23427 = CARTESIAN_POINT ( 'NONE',  ( 90.71511022959295190, -21.07400258556058503, -9.285713565094647848 ) ) ;
#23428 = EDGE_LOOP ( 'NONE', ( #7430, #9349 ) ) ;
#23429 = EDGE_LOOP ( 'NONE', ( #1466, #24608, #19083, #8972 ) ) ;
#23430 = CARTESIAN_POINT ( 'NONE',  ( 199.9999999999999716, 2.158921371974932057, 18.88613560767030464 ) ) ;
#23431 = CIRCLE ( 'NONE', #10695, 75.00000000000000000 ) ;
#23432 = LINE ( 'NONE', #7313, #6862 ) ;
#23433 = CARTESIAN_POINT ( 'NONE',  ( -86.96347745069644475, 41.18208027870598187, -15.38646221621779731 ) ) ;
#23434 = CARTESIAN_POINT ( 'NONE',  ( -114.4364955367326502, -20.04994829327650052, -8.644468109209421769 ) ) ;
#23435 = CARTESIAN_POINT ( 'NONE',  ( 23.37394308801977871, -46.80823611210205115, 13.80096434448272724 ) ) ;
#23436 = CARTESIAN_POINT ( 'NONE',  ( -188.7701102708081748, -23.55033952083662285, 43.14144101424771804 ) ) ;
#23437 = CARTESIAN_POINT ( 'NONE',  ( 180.0000000000000000, -35.78896085774750446, 82.49999999999998579 ) ) ;
#23438 = CARTESIAN_POINT ( 'NONE',  ( 136.1360204305621551, -39.99999999999994316, -4.966164525587488221 ) ) ;
#23439 = CARTESIAN_POINT ( 'NONE',  ( -135.8532207217289738, 3.005970985514575011E-13, -30.84685318188645553 ) ) ;
#23440 = CARTESIAN_POINT ( 'NONE',  ( -575.0231298121445889, 75.00000000000000000, 29.99999999999825206 ) ) ;
#23441 = CARTESIAN_POINT ( 'NONE',  ( -198.0356074513804572, -67.44298959250878056, 10.87444709758448447 ) ) ;
#23442 = CARTESIAN_POINT ( 'NONE',  ( 170.2234770963711128, 40.00000000000014211, -24.55285855007172913 ) ) ;
#23443 = FACE_OUTER_BOUND ( 'NONE', #4945, .T. ) ;
#23444 = CARTESIAN_POINT ( 'NONE',  ( -100.0753760173605258, 8.149786832858509911, 20.72827493166407464 ) ) ;
#23445 = ADVANCED_FACE ( 'NONE', ( #23806 ), #25475, .T. ) ;
#23446 = CARTESIAN_POINT ( 'NONE',  ( 180.0000000000000000, 4.582242954935206147E-14, 82.49999999999997158 ) ) ;
#23447 = CYLINDRICAL_SURFACE ( 'NONE', #23346, 5.000000000000004441 ) ;
#23448 = CARTESIAN_POINT ( 'NONE',  ( -77.56593252305926001, 22.07939426011869344, 1.556858787764804353 ) ) ;
#23449 = CARTESIAN_POINT ( 'NONE',  ( -56.48582580120559271, 21.81201906317768291, 21.81201906317777173 ) ) ;
#23450 = CIRCLE ( 'NONE', #6440, 21.53474504356810115 ) ;
#23451 = CARTESIAN_POINT ( 'NONE',  ( -30.26275506840324070, -29.48230279907817675, 27.08623969584564151 ) ) ;
#23452 = CARTESIAN_POINT ( 'NONE',  ( -187.7699188115162769, -13.79076593539094553, -46.80708926513509027 ) ) ;
#23453 = CARTESIAN_POINT ( 'NONE',  ( -105.2054292635175727, 15.19799821370213522, 15.19799821370241943 ) ) ;
#23454 = EDGE_LOOP ( 'NONE', ( #19202, #16151, #23206, #13342 ) ) ;
#23455 = CARTESIAN_POINT ( 'NONE',  ( 4.995406935893297984, 10.78321810390233892, -67.35176059882522281 ) ) ;
#23456 = ADVANCED_FACE ( 'NONE', ( #25858 ), #20014, .T. ) ;
#23457 = CYLINDRICAL_SURFACE ( 'NONE', #10309, 5.000000000000004441 ) ;
#23458 = DIRECTION ( 'NONE',  ( 0.000000000000000000, 0.000000000000000000, 1.000000000000000000 ) ) ;
#23459 = VERTEX_POINT ( 'NONE', #13207 ) ;
#23460 =( REPRESENTATION_RELATIONSHIP ('NONE','NONE', #23888, #15720 ) REPRESENTATION_RELATIONSHIP_WITH_TRANSFORMATION ( #18067 )SHAPE_REPRESENTATION_RELATIONSHIP( ) );
#23461 = CARTESIAN_POINT ( 'NONE',  ( 199.9999999999999432, -1.727494763561684666E-13, 20.00000000000010303 ) ) ;
#23462 = ADVANCED_FACE ( 'NONE', ( #3478 ), #7329, .T. ) ;
#23463 = CARTESIAN_POINT ( 'NONE',  ( 199.0199467956651063, -18.45968165710057107, -7.701887558844384252 ) ) ;
#23464 = CARTESIAN_POINT ( 'NONE',  ( 22.27781863250965344, -43.19367102557750115, 23.58928354728861976 ) ) ;
#23465 = ORIENTED_EDGE ( 'NONE', *, *, #6633, .T. ) ;
#23466 = ORIENTED_EDGE ( 'NONE', *, *, #1664, .F. ) ;
#23467 = CARTESIAN_POINT ( 'NONE',  ( -208.1127848780264742, -38.89260858015728672, -17.67593391476669851 ) ) ;
#23468 = CARTESIAN_POINT ( 'NONE',  ( -213.1075012329537230, 39.99999999999992895, 13.71589010951925935 ) ) ;
#23469 = CARTESIAN_POINT ( 'NONE',  ( 169.9999999999674571, -17.64300463372919836, -17.64300463252165585 ) ) ;
#23470 = AXIS2_PLACEMENT_3D ( 'NONE', #1298, #9408, #3684 ) ;
#23471 = DIRECTION ( 'NONE',  ( -1.836970198721030181E-16, 1.000000000000000000, 0.000000000000000000 ) ) ;
#23472 = CARTESIAN_POINT ( 'NONE',  ( -192.9588430854689989, -8.596193650988133061E-14, 14.46834944099969533 ) ) ;
#23473 = CARTESIAN_POINT ( 'NONE',  ( 200.0000000000000000, -18.09920287623689106, -5.808051173427421610 ) ) ;
#23474 = CARTESIAN_POINT ( 'NONE',  ( -82.23726319252905625, 13.38816311965448946, 15.17212531852062085 ) ) ;
#23475 = CARTESIAN_POINT ( 'NONE',  ( 199.9999999999999432, -14.14213562373115884, 14.14213562373085153 ) ) ;
#23476 = CARTESIAN_POINT ( 'NONE',  ( 91.82158438592156813, 40.45024623143973486, -16.11829626348390931 ) ) ;
#23477 = FACE_OUTER_BOUND ( 'NONE', #8356, .T. ) ;
#23478 = CARTESIAN_POINT ( 'NONE',  ( 199.9999999999999432, 2.486775779033024914E-13, -19.99999999999992539 ) ) ;
#23479 = CARTESIAN_POINT ( 'NONE',  ( 98.29820294273291381, -18.47759065023123526, -7.653668647304108674 ) ) ;
#23480 = CARTESIAN_POINT ( 'NONE',  ( 146.6084372240433709, 34.62501878078307982, 40.00000000000002132 ) ) ;
#23481 = CARTESIAN_POINT ( 'NONE',  ( 57.59792236341147031, 2.435789363418170872, -40.00000000000002132 ) ) ;
#23482 = CARTESIAN_POINT ( 'NONE',  ( -208.1127848780264742, 17.67593391476624021, 38.89260858015742883 ) ) ;
#23483 = CARTESIAN_POINT ( 'NONE',  ( -56.48582580120558561, -30.84685318188645553, -40.00000000000002132 ) ) ;
#23484 = CARTESIAN_POINT ( 'NONE',  ( -30.26275506840325136, 40.00000000000001421, 1.694272468446399227 ) ) ;
#23485 = CARTESIAN_POINT ( 'NONE',  ( 170.2234770963711128, -2.259079968736224833E-13, 24.55285855007187124 ) ) ;
#23486 = CARTESIAN_POINT ( 'NONE',  ( 4.995406935893287326, 67.35176059882533650, 10.78321810390163549 ) ) ;
#23487 = ADVANCED_FACE ( 'NONE', ( #11082, #19196 ), #6948, .T. ) ;
#23488 = CARTESIAN_POINT ( 'NONE',  ( -259.2033419157646676, 30.48217210827735713, -40.00000000000002132 ) ) ;
#23489 = VERTEX_POINT ( 'NONE', #15442 ) ;
#23490 = CARTESIAN_POINT ( 'NONE',  ( 22.17571259161115194, -43.20787961119348353, 23.59965736305207429 ) ) ;
#23491 = CARTESIAN_POINT ( 'NONE',  ( -87.13361725327075646, -15.19799821270861706, 15.19799821270823159 ) ) ;
#23492 = CARTESIAN_POINT ( 'NONE',  ( 184.8905102610680444, -14.79361573936389540, 41.77492675555996016 ) ) ;
#23493 = CARTESIAN_POINT ( 'NONE',  ( -626.9846540392142060, -82.50099999999990530, 0.000000000000000000 ) ) ;
#23494 = CARTESIAN_POINT ( 'NONE',  ( -82.25596499887640789, 19.79010929774564076, -3.998483074826426176 ) ) ;
#23495 = CARTESIAN_POINT ( 'NONE',  ( -24.53392603775155578, 12.34411287782940292, -39.81639166318235823 ) ) ;
#23496 = CARTESIAN_POINT ( 'NONE',  ( 199.9999999999998863, 8.252615397115851792, 17.12261885615216173 ) ) ;
#23497 = CARTESIAN_POINT ( 'NONE',  ( -656.1320007476808769, 39.36430177191026303, -7.173594678086772980 ) ) ;
#23498 = CARTESIAN_POINT ( 'NONE',  ( -215.0000000000000284, 57.47694228411666728, -64.52066607436458412 ) ) ;
#23499 = CARTESIAN_POINT ( 'NONE',  ( -259.2033419157646676, 21.55415060305790931, 35.01439189186571355 ) ) ;
#23500 = CARTESIAN_POINT ( 'NONE',  ( 19.06497207195981858, -10.03556273973377166, -66.60410523465827737 ) ) ;
#23501 = CARTESIAN_POINT ( 'NONE',  ( 57.59792236341147031, 30.00663442387683588, 26.56190807104703211 ) ) ;
#23502 = CARTESIAN_POINT ( 'NONE',  ( 57.59792236341147031, -1.722363176415055985, 1.722363176415024677 ) ) ;
#23503 = CARTESIAN_POINT ( 'NONE',  ( 57.59792236341147031, 30.00663442387720181, -26.56190807104661289 ) ) ;
#23505 = CARTESIAN_POINT ( 'NONE',  ( 91.82158438592158234, -12.16597498399995203, -44.40256751092347542 ) ) ;
#23504 = CARTESIAN_POINT ( 'NONE',  ( -208.1127848780264742, -38.89260858015704514, -38.89260858015768463 ) ) ;
#23506 = CARTESIAN_POINT ( 'NONE',  ( -192.9588430854690273, 10.23066800229588758, -66.79921049721882298 ) ) ;
#23507 = CARTESIAN_POINT ( 'NONE',  ( -114.7826396787323091, -1.398623183117054136, -22.13135001986807993 ) ) ;
#23508 = CARTESIAN_POINT ( 'NONE',  ( 180.0000000000000284, -135.7889608577475542, 2.284182285366599633E-14 ) ) ;
#23509 = CARTESIAN_POINT ( 'NONE',  ( -30.26275506840324070, -1.147469862568086380E-14, 1.694272468446259783 ) ) ;
#23510 = CARTESIAN_POINT ( 'NONE',  ( 163.1118516004056573, -9.006482792074626431, 47.56205970284951690 ) ) ;
#23511 = CARTESIAN_POINT ( 'NONE',  ( -208.1127848780264742, 55.00245453014418473, 40.00000000000002132 ) ) ;
#23512 = EDGE_LOOP ( 'NONE', ( #5484, #11052 ) ) ;
#23513 = CARTESIAN_POINT ( 'NONE',  ( -162.0762913951021176, 29.48230308784768638, -27.08623940707612121 ) ) ;
#23514 = B_SPLINE_CURVE_WITH_KNOTS ( 'NONE', 3,
 ( #13426, #4951, #954, #11422, #7177, #9061 ),
 .UNSPECIFIED., .F., .F.,
 ( 4, 2, 4 ),
 ( 0.000000000000000000, 0.004168007559015109859, 0.008336015118030219717 ),
 .UNSPECIFIED. ) ;
#23515 =( BOUNDED_CURVE ( )  B_SPLINE_CURVE ( 3, ( #23114, #4886, #21114, #3018 ),
 .UNSPECIFIED., .F., .F. ) 
 B_SPLINE_CURVE_WITH_KNOTS ( ( 4, 4 ),
 ( 0.01388163287021749320, 0.02359082919309987009 ),
 .UNSPECIFIED. ) 
 CURVE ( )  GEOMETRIC_REPRESENTATION_ITEM ( )  RATIONAL_B_SPLINE_CURVE ( ( 1.000000000000000000, 0.8672072324488975248, 0.7608653435686167921, 0.6809743333591576908 ) ) 
 REPRESENTATION_ITEM ( '' )  );
#23516 = CARTESIAN_POINT ( 'NONE',  ( -87.02159130206896975, -18.50869357302490315, -10.86091765595724468 ) ) ;
#23517 = CARTESIAN_POINT ( 'NONE',  ( 23.64688638900135587, 23.28414885118118249, 42.77321027809743725 ) ) ;
#23518 = CARTESIAN_POINT ( 'NONE',  ( -39.58644176650890500, -32.83087322311865819, -13.59899295362217764 ) ) ;
#23519 = ORIENTED_EDGE ( 'NONE', *, *, #7750, .T. ) ;
#23520 = CARTESIAN_POINT ( 'NONE',  ( -183.1090696430980529, -41.47043467734991395, 22.43564075026454319 ) ) ;
#23521 = CARTESIAN_POINT ( 'NONE',  ( 199.9999999999998295, -11.08011877867584261, -15.44095579151349185 ) ) ;
#23522 = CARTESIAN_POINT ( 'NONE',  ( 45.01779936585140263, -12.15764947731424250, 38.89115870265484176 ) ) ;
#23523 = DIRECTION ( 'NONE',  ( -0.000000000000000000, -0.000000000000000000, -1.000000000000000000 ) ) ;
#23524 = CARTESIAN_POINT ( 'NONE',  ( 199.0062091525825849, 18.60380424647159003, -7.335505861489442836 ) ) ;
#23525 = ADVANCED_FACE ( 'NONE', ( #23326 ), #13084, .T. ) ;
#23526 = CARTESIAN_POINT ( 'NONE',  ( -99.29480781227181296, -20.48155342677142698, -8.934325994365357460 ) ) ;
#23527 = CARTESIAN_POINT ( 'NONE',  ( -280.0000000000000568, 40.00000000000004263, -19.99999999999987210 ) ) ;
#23528 = DIRECTION ( 'NONE',  ( 0.9698969544100581874, -0.09318942523027390346, 0.2249791742614079271 ) ) ;
#23529 = CARTESIAN_POINT ( 'NONE',  ( -199.9999999999999716, -14.89048929005484467, -48.59548038928831915 ) ) ;
#23530 = CARTESIAN_POINT ( 'NONE',  ( -86.96347745069643054, -18.24025645688353947, 40.00000000000002132 ) ) ;
#23532 = CYLINDRICAL_SURFACE ( 'NONE', #11283, 20.53474504356812247 ) ;
#23531 = CARTESIAN_POINT ( 'NONE',  ( 83.01683444512164556, -9.947410331075138501, -24.01517293243385609 ) ) ;
#23533 = CARTESIAN_POINT ( 'NONE',  ( -135.8532207217289738, 9.153146818113548022, 40.00000000000002132 ) ) ;
#23534 = CARTESIAN_POINT ( 'NONE',  ( -238.4067589809705794, -0.6820004457913680929, 0.6820004457913170226 ) ) ;
#23535 = CARTESIAN_POINT ( 'NONE',  ( 192.4448373802100889, -1.741373372144848397E-13, 20.00000000003942091 ) ) ;
#23536 = CARTESIAN_POINT ( 'NONE',  ( 184.8905102610680444, -39.99999999999978684, -19.07866798485600768 ) ) ;
#23537 = DIRECTION ( 'NONE',  ( 0.000000000000000000, 1.000000000000000000, 0.000000000000000000 ) ) ;
#23538 = ADVANCED_FACE ( 'NONE', ( #9336 ), #23447, .F. ) ;
#23539 = EDGE_LOOP ( 'NONE', ( #22948, #14086, #15337, #13524, #16648, #13648, #19702, #8091 ) ) ;
#23541 = CARTESIAN_POINT ( 'NONE',  ( -3.494657986428189922, 43.29048295385600653, -17.93150516116771342 ) ) ;
#23540 = CARTESIAN_POINT ( 'NONE',  ( 98.29820294267349823, 10.02182676112789217, -17.32045324915450379 ) ) ;
#23542 = CARTESIAN_POINT ( 'NONE',  ( -86.96347745069645896, 21.75974354311648895, 40.00000000000002132 ) ) ;
#23543 = EDGE_CURVE ( 'NONE', #18515, #14022, #25455, .T. ) ;
#23544 = FILL_AREA_STYLE_COLOUR ( '', #884 ) ;
#23545 = CARTESIAN_POINT ( 'NONE',  ( -192.1963514251025913, 43.96876056338943783, -24.16258207727797824 ) ) ;
#23546 = CARTESIAN_POINT ( 'NONE',  ( 0.000000000000000000, 0.000000000000000000, 0.000000000000000000 ) ) ;
#23547 = ORIENTED_EDGE ( 'NONE', *, *, #8837, .T. ) ;
#23548 = ORIENTED_EDGE ( 'NONE', *, *, #21119, .F. ) ;
#23549 = CARTESIAN_POINT ( 'NONE',  ( 151.7948205124836250, 23.49921654116361225, -23.49921654116333514 ) ) ;
#23550 = CARTESIAN_POINT ( 'NONE',  ( 144.1620285550791891, 12.51613133675877876, -30.21661402164554744 ) ) ;
#23551 = CARTESIAN_POINT ( 'NONE',  ( -188.2995950289364089, 43.00522595870987885, -23.44932284465868477 ) ) ;
#23552 = VERTEX_POINT ( 'NONE', #17958 ) ;
#23553 = CARTESIAN_POINT ( 'NONE',  ( 199.9999999999999147, 2.470466796131644660, 18.84784629003980783 ) ) ;
#23554 = CARTESIAN_POINT ( 'NONE',  ( -192.1166648175283740, 14.00295691731063386, 48.16216898722862538 ) ) ;
#23555 = CARTESIAN_POINT ( 'NONE',  ( -198.0356074513804572, 39.15871834505901461, 39.15871834505919935 ) ) ;
#23556 = DIRECTION ( 'NONE',  ( -1.000000000000000000, -0.000000000000000000, -0.000000000000000000 ) ) ;
#23557 = CARTESIAN_POINT ( 'NONE',  ( -238.4067589809705794, -4.716212492215116094E-14, 0.9644942799825824142 ) ) ;
#23558 = DIRECTION ( 'NONE',  ( 0.000000000000000000, -1.000000000000000000, 0.000000000000000000 ) ) ;
#23559 = DIRECTION ( 'NONE',  ( -1.000000000000000000, -0.000000000000000000, -0.000000000000000000 ) ) ;
#23560 = DIRECTION ( 'NONE',  ( 0.000000000000000000, 0.000000000000000000, 1.000000000000000000 ) ) ;
#23561 = CARTESIAN_POINT ( 'NONE',  ( -238.4067589809705794, -40.00000000000005684, -0.9644942799830014124 ) ) ;
#23562 = CARTESIAN_POINT ( 'NONE',  ( 170.2234770963711128, 40.00000000000021316, -15.44714144992773797 ) ) ;
#23563 = CARTESIAN_POINT ( 'NONE',  ( -86.84055334702942730, 19.72499881414481493, 8.026593896031025466 ) ) ;
#23564 = CARTESIAN_POINT ( 'NONE',  ( 151.7948205124836250, 23.49921654116361225, -23.49921654116333514 ) ) ;
#23565 = CARTESIAN_POINT ( 'NONE',  ( -198.0356074513804572, -9.007331120208026888E-14, 15.37879056873070560 ) ) ;
#23566 = CARTESIAN_POINT ( 'NONE',  ( -259.2033419157646676, 6.730120644403521979, -6.730120644403498886 ) ) ;
#23567 = CARTESIAN_POINT ( 'NONE',  ( -109.1264249741457490, -13.72187187121248364, 33.12752917270315578 ) ) ;
#23568 = B_SPLINE_CURVE_WITH_KNOTS ( 'NONE', 3,
 ( #13133, #2769, #8876, #10878, #18993, #3026, #25509, #1030, #17753, #11503 ),
 .UNSPECIFIED., .F., .F.,
 ( 4, 2, 2, 2, 4 ),
 ( 0.7921542097164080420, 0.8508620842112317728, 0.8814014469398914198, 0.9119408096685510667, 0.9406682828395580565 ),
 .UNSPECIFIED. ) ;
#23569 = LINE ( 'NONE', #1099, #6844 ) ;
#23570 = CARTESIAN_POINT ( 'NONE',  ( 190.0000000000000000, 66.50000000000009948, -66.50000000000005684 ) ) ;
#23571 = CARTESIAN_POINT ( 'NONE',  ( -82.28266731793512179, -17.99064928892019211, 9.155589012557189932 ) ) ;
#23572 = CARTESIAN_POINT ( 'NONE',  ( 0.2972598230770011618, 10.13633138497462305, 66.70487387989858519 ) ) ;
#23573 = CARTESIAN_POINT ( 'NONE',  ( -100.7734535825088500, -12.25131212657524316, 44.31723036834888774 ) ) ;
#23574 = CARTESIAN_POINT ( 'NONE',  ( -644.6425580139975864, 33.33320607737224606, -30.23934288404415938 ) ) ;
#23575 = DIRECTION ( 'NONE',  ( 0.2259624730582988905, 0.9741360073261728925, 0.000000000000000000 ) ) ;
#23576 = ORIENTED_EDGE ( 'NONE', *, *, #3862, .T. ) ;
#23577 = CARTESIAN_POINT ( 'NONE',  ( 136.1360204305621266, 3.511608612530757068, -3.511608612530642937 ) ) ;
#23578 = FACE_OUTER_BOUND ( 'NONE', #956, .T. ) ;
#23579 = CARTESIAN_POINT ( 'NONE',  ( -620.9980249814747140, 28.88918448956861695, 34.50439121308308899 ) ) ;
#23580 = ORIENTED_EDGE ( 'NONE', *, *, #14999, .F. ) ;
#23581 = CARTESIAN_POINT ( 'NONE',  ( -86.96347745069643054, -40.00000000000026290, 21.75974354311608749 ) ) ;
#23582 = CARTESIAN_POINT ( 'NONE',  ( 199.0194986905590895, -18.08904332876870313, -8.539272476510683774 ) ) ;
#23583 = CARTESIAN_POINT ( 'NONE',  ( -70.35386311745469357, 10.19784241653377777, 22.51194464762888003 ) ) ;
#23584 = ORIENTED_EDGE ( 'NONE', *, *, #5398, .F. ) ;
#23585 = ORIENTED_EDGE ( 'NONE', *, *, #6860, .F. ) ;
#23586 = CARTESIAN_POINT ( 'NONE',  ( -192.9588430854689989, -10.23066800230756890, 10.23066800230742501 ) ) ;
#23587 = CARTESIAN_POINT ( 'NONE',  ( 192.4448373802100889, -3.692737725850373501E-14, 19.99999999996060751 ) ) ;
#23588 = CARTESIAN_POINT ( 'NONE',  ( -105.2054292635175869, 15.19799821370233062, -15.19799821370219206 ) ) ;
#23589 = EDGE_CURVE ( 'NONE', #9969, #9873, #5429, .T. ) ;
#23590 = CARTESIAN_POINT ( 'NONE',  ( 191.7822011676492195, 14.08373552998004463, -14.08373552997966449 ) ) ;
#23591 = CARTESIAN_POINT ( 'NONE',  ( 130.8568914410475088, -40.00000000000001421, 5.949712681206549725 ) ) ;
#23592 = CARTESIAN_POINT ( 'NONE',  ( 200.0000000000000853, -18.97025941512468705, -1.247367644282773691 ) ) ;
#23593 = MECHANICAL_DESIGN_GEOMETRIC_PRESENTATION_REPRESENTATION (  '', ( #8299 ), #12128 ) ;
#23594 = CARTESIAN_POINT ( 'NONE',  ( 19.06497207195981147, -4.605042221739098431E-14, 14.19242893257840521 ) ) ;
#23595 = PLANE ( 'NONE',  #16428 ) ;
#23596 = CARTESIAN_POINT ( 'NONE',  ( 19.06497207195980792, 10.03556273973447155, -10.03556273973422286 ) ) ;
#23597 = CARTESIAN_POINT ( 'NONE',  ( -162.0762913951021176, 27.08623940707639477, -29.48230308784743059 ) ) ;
#23598 = LINE ( 'NONE', #9889, #25879 ) ;
#23599 = CARTESIAN_POINT ( 'NONE',  ( 19.06497207195981858, 5.735870351258996432E-13, -54.19242893257843008 ) ) ;
#23600 = CARTESIAN_POINT ( 'NONE',  ( -626.9846540392142060, 90.00000000000000000, -54.99999999999995026 ) ) ;
#23601 = CARTESIAN_POINT ( 'NONE',  ( 146.6084372240433709, -5.374981219216948602, 40.00000000000002132 ) ) ;
#23602 = CARTESIAN_POINT ( 'NONE',  ( -259.2033419157646676, 9.517827891722582478, -40.00000000000002132 ) ) ;
#23603 = CARTESIAN_POINT ( 'NONE',  ( 4.995406935893287326, 17.50105314357170627, 39.06748935135200895 ) ) ;
#23604 = CARTESIAN_POINT ( 'NONE',  ( 184.8905102610680444, 20.92133201514447549, 0.000000000000000000 ) ) ;
#23606 = CARTESIAN_POINT ( 'NONE',  ( -716.9846540392142060, 66.50000000000009948, -66.50000000000005684 ) ) ;
#23605 = CARTESIAN_POINT ( 'NONE',  ( -105.3841681040955933, 6.699016078400306107, 20.33889746609499838 ) ) ;
#23607 = CARTESIAN_POINT ( 'NONE',  ( 130.8568914410475372, -3.326198072800416995E-13, 34.05028731879788495 ) ) ;
#23608 = CARTESIAN_POINT ( 'NONE',  ( 199.9999999999999432, 14.14213562373090838, 14.14213562373092437 ) ) ;
#23609 = CARTESIAN_POINT ( 'NONE',  ( -100.7734535825088500, 17.32597176626809699, -40.00000000000002132 ) ) ;
#23610 = EDGE_LOOP ( 'NONE', ( #7758, #12958 ) ) ;
#23611 = CARTESIAN_POINT ( 'NONE',  ( 25.62979979008006381, -45.99287499155195746, 13.63460241477595325 ) ) ;
#23612 = VECTOR ( 'NONE', #8645, 1000.000000000000000 ) ;
#23613 = ADVANCED_FACE ( 'NONE', ( #25839 ), #2157, .T. ) ;
#23614 = CARTESIAN_POINT ( 'NONE',  ( -213.1075012329537230, 9.698598906462684965, 66.26714140138669507 ) ) ;
#23615 = DIRECTION ( 'NONE',  ( -0.000000000000000000, 1.000000000000000000, -0.000000000000000000 ) ) ;
#23616 = CARTESIAN_POINT ( 'NONE',  ( -86.93367134006987840, 20.20393068805329762, 7.058177991699935205 ) ) ;
#23617 = EDGE_CURVE ( 'NONE', #11180, #4752, #23399, .T. ) ;
#23618 = CARTESIAN_POINT ( 'NONE',  ( 200.0000000000000284, 10.29196162618721644, 15.98165385515595815 ) ) ;
#23619 = EDGE_CURVE ( 'NONE', #25051, #13654, #10199, .T. ) ;
#23620 = CARTESIAN_POINT ( 'NONE',  ( -77.78739057084328579, -20.88856886083027575, -6.814681957699006531 ) ) ;
#23621 = ADVANCED_FACE ( 'NONE', ( #1451 ), #25801, .F. ) ;
#23622 = CARTESIAN_POINT ( 'NONE',  ( -87.05569247515344955, -4.389928423847803352, -20.98769100332471638 ) ) ;
#23623 = CARTESIAN_POINT ( 'NONE',  ( -162.0762913951020892, 1.198031840385732849, -1.198031840385733515 ) ) ;
#23624 = CARTESIAN_POINT ( 'NONE',  ( -162.0762913951020892, -1.198031840315659124, -57.76657433523998009 ) ) ;
#23625 = CARTESIAN_POINT ( 'NONE',  ( -114.7760651468638571, 22.09554796279716626, -1.204233200294609896 ) ) ;
#23626 = FACE_OUTER_BOUND ( 'NONE', #24648, .T. ) ;
#23627 = CARTESIAN_POINT ( 'NONE',  ( -162.0762913951020892, -1.198031840315659124, -57.76657433523998009 ) ) ;
#23629 = CARTESIAN_POINT ( 'NONE',  ( 91.82158438592158234, -40.45024623143936537, -16.11829626348475131 ) ) ;
#23628 = CARTESIAN_POINT ( 'NONE',  ( -192.9588430854690273, -10.23066800231931239, -66.79921049724377724 ) ) ;
#23630 = CARTESIAN_POINT ( 'NONE',  ( -56.48582580120559271, 21.81201906317798489, -21.81201906317746619 ) ) ;
#23631 = CARTESIAN_POINT ( 'NONE',  ( -208.1127848780265026, -10.60833733269551971, 10.60833733269537049 ) ) ;
#23632 = CARTESIAN_POINT ( 'NONE',  ( 136.1360204305621266, 35.03383547441298873, 0.000000000000000000 ) ) ;
#23633 = CARTESIAN_POINT ( 'NONE',  ( 136.1360204305621551, -39.99999999999987921, -35.03383547441310242 ) ) ;
#23634 = CARTESIAN_POINT ( 'NONE',  ( 136.1360204305621266, -24.77266263493151044, 24.77266263493093135 ) ) ;
#23635 = CARTESIAN_POINT ( 'NONE',  ( 146.6084372240433709, -34.62501878078303008, 40.00000000000002132 ) ) ;
#23636 = VERTEX_POINT ( 'NONE', #9686 ) ;
#23637 = AXIS2_PLACEMENT_3D ( 'NONE', #19920, #3694, #13407 ) ;
#23638 = CARTESIAN_POINT ( 'NONE',  ( 163.1118516004056573, 37.29075403953160617, -19.27778845539222985 ) ) ;
#23639 = AXIS2_PLACEMENT_3D ( 'NONE', #15876, #4070, #24005 ) ;
#23640 = CARTESIAN_POINT ( 'NONE',  ( 22.63898026999810043, 42.29338810984155828, 17.51849495380543331 ) ) ;
#23641 = CARTESIAN_POINT ( 'NONE',  ( 23.05038679986142469, 17.85133178553910582, 43.09692730307104824 ) ) ;
#23642 = CARTESIAN_POINT ( 'NONE',  ( -7.297127544327485893, -45.86058602274801643, -13.59739983758753645 ) ) ;
#23643 = VERTEX_POINT ( 'NONE', #7948 ) ;
#23644 = CARTESIAN_POINT ( 'NONE',  ( -114.4364955367328207, -20.29001642038830155, 8.064892380842811903 ) ) ;
#23645 = CARTESIAN_POINT ( 'NONE',  ( 200.0000000000000853, -8.685123034760072969, -16.90575535186691880 ) ) ;
#23646 = CARTESIAN_POINT ( 'NONE',  ( 44.65795722950328894, -15.21593185908468726, 36.73450905844209302 ) ) ;
#23647 = CARTESIAN_POINT ( 'NONE',  ( 90.71511022963046855, 9.285713564076607085, -21.07400258596608822 ) ) ;
#23648 = CARTESIAN_POINT ( 'NONE',  ( 199.0060120359516986, 18.22327268582330007, -8.235267977567980680 ) ) ;
#23649 = CARTESIAN_POINT ( 'NONE',  ( -103.9474983245028881, -19.92928099173742496, -8.577167319634591891 ) ) ;
#23650 = CARTESIAN_POINT ( 'NONE',  ( 146.6084372240433709, 40.00000000000003553, 5.374981219217116468 ) ) ;
#23652 = AXIS2_PLACEMENT_3D ( 'NONE', #11351, #21226, #19468 ) ;
#23651 = PLANE ( 'NONE',  #11292 ) ;
#23653 = DIRECTION ( 'NONE',  ( 0.000000000000000000, 1.000000000000000000, 0.000000000000000000 ) ) ;
#23654 = CARTESIAN_POINT ( 'NONE',  ( -86.96347745069645896, 21.75974354311648895, 40.00000000000002132 ) ) ;
#23656 = CARTESIAN_POINT ( 'NONE',  ( -597.7037569780933381, 39.46347844285461548, -6.549284831979162114 ) ) ;
#23655 = CARTESIAN_POINT ( 'NONE',  ( 90.68848816889322961, -9.291443202883320041, -21.08311784352002505 ) ) ;
#23657 = CARTESIAN_POINT ( 'NONE',  ( 192.4448373802101173, -19.99999999996057554, 40.00000000000002132 ) ) ;
#23658 = CARTESIAN_POINT ( 'NONE',  ( 57.59792236341147031, 2.435789363418170872, -40.00000000000002132 ) ) ;
#23659 = CARTESIAN_POINT ( 'NONE',  ( -91.56559293963834989, -22.67402823373193499, 0.000000000000000000 ) ) ;
#23660 = CARTESIAN_POINT ( 'NONE',  ( -280.0000000000000568, 39.99999999999976552, 20.00000000000043343 ) ) ;
#23661 = CARTESIAN_POINT ( 'NONE',  ( 199.9999999999999432, 2.486775779033024914E-13, -19.99999999999992539 ) ) ;
#23662 = DIRECTION ( 'NONE',  ( 0.000000000000000000, 1.000000000000000000, 0.000000000000000000 ) ) ;
#23663 = EDGE_LOOP ( 'NONE', ( #7810, #22259 ) ) ;
#23665 = CARTESIAN_POINT ( 'NONE',  ( 1.925538622547987355, 48.64880301058932588, -14.07631154916797733 ) ) ;
#23664 = DIRECTION ( 'NONE',  ( 0.000000000000000000, 0.000000000000000000, -1.000000000000000000 ) ) ;
#23666 = CARTESIAN_POINT ( 'NONE',  ( 14.38125909742182884, -55.17850393971007605, 40.00000000000002132 ) ) ;
#23667 = CARTESIAN_POINT ( 'NONE',  ( 0.2972598230769938343, 10.13633138497486286, -10.13633138497461594 ) ) ;
#23668 = CARTESIAN_POINT ( 'NONE',  ( -188.6889827002243578, 47.12918603174835397, -13.84869468768081369 ) ) ;
#23669 = DIRECTION ( 'NONE',  ( 0.000000000000000000, -0.9242245927363030855, -0.3818493186865927203 ) ) ;
#23670 = ORIENTED_EDGE ( 'NONE', *, *, #24595, .F. ) ;
#23671 = ORIENTED_EDGE ( 'NONE', *, *, #14107, .F. ) ;
#23672 = CARTESIAN_POINT ( 'NONE',  ( -89.92902785008668332, 8.734793929541243784, -20.17328762787294139 ) ) ;
#23673 = CARTESIAN_POINT ( 'NONE',  ( 135.5356265174576720, 12.51227922893905387, -30.20731421070341582 ) ) ;
#23674 = ORIENTED_EDGE ( 'NONE', *, *, #23848, .F. ) ;
#23675 = CARTESIAN_POINT ( 'NONE',  ( -99.29480781227204034, 8.165122821357641669, -20.80016781325159414 ) ) ;
#23676 = VERTEX_POINT ( 'NONE', #17660 ) ;
#23677 = CARTESIAN_POINT ( 'NONE',  ( 199.0263554293247523, -15.04073044714995611, 13.19117051905602089 ) ) ;
#23678 = DIRECTION ( 'NONE',  ( 0.000000000000000000, -1.000000000000000000, 0.000000000000000000 ) ) ;
#23679 = CARTESIAN_POINT ( 'NONE',  ( -208.1127848780264742, 67.17687982760683951, 10.60833733268317403 ) ) ;
#23680 = DIRECTION ( 'NONE',  ( 0.000000000000000000, -1.000000000000000000, 0.000000000000000000 ) ) ;
#23681 = CARTESIAN_POINT ( 'NONE',  ( 163.1118516004056573, 1.251511021549353291E-13, -27.26290988616872824 ) ) ;
#23682 = CARTESIAN_POINT ( 'NONE',  ( -199.9999999999999716, -45.81998439131056244, 19.51623549979313665 ) ) ;
#23683 = CARTESIAN_POINT ( 'NONE',  ( -626.9846540392097722, 90.00000000000000000, 59.99999999999999289 ) ) ;
#23684 = DIRECTION ( 'NONE',  ( 0.000000000000000000, -0.000000000000000000, -1.000000000000000000 ) ) ;
#23685 = CARTESIAN_POINT ( 'NONE',  ( 146.6084372240433993, -3.357462877844280890E-13, 34.62501878078305850 ) ) ;
#23686 = CARTESIAN_POINT ( 'NONE',  ( 146.6084372240433993, 8.568076647504290689E-14, -5.374981219216972583 ) ) ;
#23687 = ADVANCED_FACE ( 'NONE', ( #26342 ), #21668, .T. ) ;
#23688 = CARTESIAN_POINT ( 'NONE',  ( -110.0685463886661068, -10.00056106068391948, 17.53216629777173452 ) ) ;
#23689 = CARTESIAN_POINT ( 'NONE',  ( -30.26275506840324070, -1.198031551616032919, 1.198031551616014712 ) ) ;
#23690 = CARTESIAN_POINT ( 'NONE',  ( -199.9999999999999432, 14.17215463606722636, -49.28189405767596298 ) ) ;
#23691 = CARTESIAN_POINT ( 'NONE',  ( -197.4154352061136137, 14.14666496778293592, 49.11380478893853052 ) ) ;
#23692 = CARTESIAN_POINT ( 'NONE',  ( 110.0479209278586694, 22.74092928740047626, 9.419601331808811651 ) ) ;
#23693 = CARTESIAN_POINT ( 'NONE',  ( 210.0000000000000284, 66.50000000000009948, -66.50000000000005684 ) ) ;
#23694 = CARTESIAN_POINT ( 'NONE',  ( 192.4448373802100889, 14.14213562375893574, -14.14213562375874922 ) ) ;
#23695 = CARTESIAN_POINT ( 'NONE',  ( 130.8568914410475088, -39.99999999999988631, -34.05028731879802706 ) ) ;
#23696 = CARTESIAN_POINT ( 'NONE',  ( 14.38125909742181285, -17.55144818341476309, 39.01709431150910490 ) ) ;
#23697 = CARTESIAN_POINT ( 'NONE',  ( -105.3755690713226585, -41.18208027870611687, 15.38646221621750954 ) ) ;
#23698 = CARTESIAN_POINT ( 'NONE',  ( -656.4562131466713026, 40.84575396553432824, -18.91241459347874354 ) ) ;
#23699 = CARTESIAN_POINT ( 'NONE',  ( -77.70103689343427789, 11.20642775818909520, 18.98727594172718725 ) ) ;
#23700 = ORIENTED_EDGE ( 'NONE', *, *, #2591, .F. ) ;
#23701 = CARTESIAN_POINT ( 'NONE',  ( 192.4448373802101173, 42.42640687116487896, 14.14213562375934075 ) ) ;
#23702 = DIRECTION ( 'NONE',  ( 0.000000000000000000, 1.000000000000000000, 0.000000000000000000 ) ) ;
#23703 = B_SPLINE_CURVE_WITH_KNOTS ( 'NONE', 3,
 ( #5493, #9613, #26127, #19593, #17848, #25998 ),
 .UNSPECIFIED., .F., .F.,
 ( 4, 2, 4 ),
 ( -0.0001050551439130371028, 0.04006379722394161347, 0.08023264959179625400 ),
 .UNSPECIFIED. ) ;
#23704 = DIRECTION ( 'NONE',  ( 0.000000000000000000, 0.000000000000000000, -1.000000000000000000 ) ) ;
#23705 = ORIENTED_EDGE ( 'NONE', *, *, #10042, .T. ) ;
#23706 = CARTESIAN_POINT ( 'NONE',  ( -238.4067589809705794, -3.369206980223063916E-14, -0.9644942799825824142 ) ) ;
#23707 = CARTESIAN_POINT ( 'NONE',  ( 199.0159316777080676, -14.10546057009464072, -14.17879677899387758 ) ) ;
#23708 = CARTESIAN_POINT ( 'NONE',  ( 21.16156876808018694, -43.48822901267196528, 23.80729322913559187 ) ) ;
#23709 = ORIENTED_EDGE ( 'NONE', *, *, #19706, .T. ) ;
#23710 = ORIENTED_EDGE ( 'NONE', *, *, #9807, .F. ) ;
#23711 = CARTESIAN_POINT ( 'NONE',  ( -100.7734535825088500, 16.03295912088713848, -16.03295912088698927 ) ) ;
#23712 = CARTESIAN_POINT ( 'NONE',  ( 170.2234770963711128, -2.511315425431857630E-14, 15.44714144992816074 ) ) ;
#23713 = EDGE_CURVE ( 'NONE', #16552, #19937, #1982, .T. ) ;
#23714 = DIRECTION ( 'NONE',  ( 0.01051738792039888168, -0.3656191332797650295, -0.9307051272723736446 ) ) ;
#23715 = CARTESIAN_POINT ( 'NONE',  ( 200.0000000000000000, 69.29737539576909455, -75.30386416458597409 ) ) ;
#23716 = CARTESIAN_POINT ( 'NONE',  ( 4.995406935893305089, -40.00000000000021316, 55.24977328853194791 ) ) ;
#23717 = CARTESIAN_POINT ( 'NONE',  ( 200.0000000000000284, -15.36457271445731543, -11.18861246136148502 ) ) ;
#23718 = CARTESIAN_POINT ( 'NONE',  ( 151.7948205124836534, 40.00000000000017053, -33.23291073765538783 ) ) ;
#23719 = FACE_OUTER_BOUND ( 'NONE', #24338, .T. ) ;
#23720 = CARTESIAN_POINT ( 'NONE',  ( -86.96347745069644475, -15.38646221621807442, 15.38646221621768184 ) ) ;
#23721 = CARTESIAN_POINT ( 'NONE',  ( -91.56559293963834989, 16.03295912088740849, -40.53558337403661938 ) ) ;
#23722 = CARTESIAN_POINT ( 'NONE',  ( -87.04503123322947999, -18.12276621389172959, 11.46092073712200232 ) ) ;
#23723 = CARTESIAN_POINT ( 'NONE',  ( 163.1118516004056573, -2.556006622855449647E-13, 27.26290988616872824 ) ) ;
#23724 = FACE_BOUND ( 'NONE', #17041, .T. ) ;
#23725 = CARTESIAN_POINT ( 'NONE',  ( -105.3755690713226869, 21.75974354311648540, -0.000000000000000000 ) ) ;
#23726 = CARTESIAN_POINT ( 'NONE',  ( 200.0000000000000000, -19.99999999999988631, -40.00000000000002132 ) ) ;
#23727 = CARTESIAN_POINT ( 'NONE',  ( 4.995406935893293543, -10.78321810389005364, 10.78321810388994173 ) ) ;
#23728 = CARTESIAN_POINT ( 'NONE',  ( -56.48582580120559271, 9.153146818113576444, -0.000000000000000000 ) ) ;
#23729 = CARTESIAN_POINT ( 'NONE',  ( -105.4053751741942335, 19.27722189457469781, 9.295450928565532678 ) ) ;
#23730 = CARTESIAN_POINT ( 'NONE',  ( -259.2033419157646676, -1.473088368616265084E-13, 9.517827891722632216 ) ) ;
#23731 = CARTESIAN_POINT ( 'NONE',  ( -100.7734535825088500, 40.53558337403677569, -16.03295912088699993 ) ) ;
#23732 = CARTESIAN_POINT ( 'NONE',  ( 91.82158438592158234, 22.79471317813472453, -40.00000000000002132 ) ) ;
#23734 = VERTEX_POINT ( 'NONE', #16204 ) ;
#23733 = AXIS2_PLACEMENT_3D ( 'NONE', #22831, #25224, #609 ) ;
#23735 = CARTESIAN_POINT ( 'NONE',  ( 23.38399212876576527, -46.80460545930662875, 13.80022400692479501 ) ) ;
#23736 = CARTESIAN_POINT ( 'NONE',  ( 110.0479209278586836, 9.419601331808605593, 22.74092928740057218 ) ) ;
#23737 = CARTESIAN_POINT ( 'NONE',  ( -162.0762913951021176, 29.48230308784768638, -27.08623940707612121 ) ) ;
#23738 = CARTESIAN_POINT ( 'NONE',  ( -56.48582580120557850, -40.00000000000014211, 30.84685318188629921 ) ) ;
#23739 = CARTESIAN_POINT ( 'NONE',  ( 130.8568914410475088, 4.207082182989012153, 52.36146031193425188 ) ) ;
#23740 = CARTESIAN_POINT ( 'NONE',  ( -100.7734535825088500, -22.67402823373193499, -40.00000000000002132 ) ) ;
#23741 = DIRECTION ( 'NONE',  ( 0.000000000000000000, 0.000000000000000000, 1.000000000000000000 ) ) ;
#23742 = CARTESIAN_POINT ( 'NONE',  ( 199.9999999999999147, 2.470466796131644660, 18.84784629003980783 ) ) ;
#23743 = CARTESIAN_POINT ( 'NONE',  ( 169.9999999999999716, -19.80854622259151654, 15.47746304364889447 ) ) ;
#23744 = CARTESIAN_POINT ( 'NONE',  ( -30.26275506840325136, 29.48230279907760121, 27.08623969584625613 ) ) ;
#23745 = CARTESIAN_POINT ( 'NONE',  ( -91.56559293963834989, 16.03295912088740849, -40.53558337403661938 ) ) ;
#23746 = CARTESIAN_POINT ( 'NONE',  ( 170.2234770963711128, 17.36149277827004411, -17.36149277826983095 ) ) ;
#23747 = DIRECTION ( 'NONE',  ( -1.000000000000000000, -0.000000000000000000, -0.000000000000000000 ) ) ;
#23748 = CARTESIAN_POINT ( 'NONE',  ( 192.4448373802101173, 42.42640687122089815, -14.14213562370272470 ) ) ;
#23750 = CARTESIAN_POINT ( 'NONE',  ( -280.0000000000000568, -42.42640687119276066, -14.14213562373147148 ) ) ;
#23749 = CARTESIAN_POINT ( 'NONE',  ( 91.82158438592159655, 12.16597498400091304, -44.40256751092321963 ) ) ;
#23751 = CARTESIAN_POINT ( 'NONE',  ( 14.38125909742180752, 10.73282306404735387, -10.73282306404708919 ) ) ;
#23752 = AXIS2_PLACEMENT_3D ( 'NONE', #20868, #10757, #9274 ) ;
#23753 = CARTESIAN_POINT ( 'NONE',  ( -114.6379872168154890, -5.502324066487487286, -21.35005244387444989 ) ) ;
#23754 = DIRECTION ( 'NONE',  ( -1.836970198721030181E-16, 1.000000000000000000, 0.000000000000000000 ) ) ;
#23755 = ADVANCED_FACE ( 'NONE', ( #24336 ), #3443, .T. ) ;
#23756 = CARTESIAN_POINT ( 'NONE',  ( -208.1127848780264742, -40.00000000000025580, 55.00245453014408525 ) ) ;
#23757 = CARTESIAN_POINT ( 'NONE',  ( 4.995406935893301537, -10.78321810390187530, 67.35176059882529387 ) ) ;
#23758 = CARTESIAN_POINT ( 'NONE',  ( 192.4448373802100889, -14.14213562375896061, 14.14213562375865330 ) ) ;
#23759 = CARTESIAN_POINT ( 'NONE',  ( -198.0356074513804572, 55.37879056873070027, 2.449293598294708485E-15 ) ) ;
#23760 = VERTEX_POINT ( 'NONE', #2375 ) ;
#23761 = CARTESIAN_POINT ( 'NONE',  ( -238.4067589809705794, 0.6820004457912757223, 0.6820004457913219076 ) ) ;
#23762 = ADVANCED_FACE ( 'NONE', ( #24864 ), #16443, .T. ) ;
#23763 = CARTESIAN_POINT ( 'NONE',  ( -48.88328292457690338, 29.77915576935907183, 12.33493019568957649 ) ) ;
#23764 = CARTESIAN_POINT ( 'NONE',  ( -77.90255099906769942, -8.064892378657791738, -20.29001641120690635 ) ) ;
#23765 = CARTESIAN_POINT ( 'NONE',  ( 14.38125909742180752, 15.17850393972634038, 0.000000000000000000 ) ) ;
#23766 = EDGE_CURVE ( 'NONE', #23081, #17509, #18452, .T. ) ;
#23767 = EDGE_CURVE ( 'NONE', #25051, #10094, #19704, .T. ) ;
#23768 = ORIENTED_EDGE ( 'NONE', *, *, #7837, .T. ) ;
#23769 = CARTESIAN_POINT ( 'NONE',  ( -192.9370391625363936, -48.35015248261021270, 14.03127550871790419 ) ) ;
#23770 = CARTESIAN_POINT ( 'NONE',  ( 200.0000000000000568, -16.61842928396364272, -9.229186156037545885 ) ) ;
#23771 = CARTESIAN_POINT ( 'NONE',  ( 23.39921416754910055, -13.79910252519578862, 46.79910576274385647 ) ) ;
#23772 = CIRCLE ( 'NONE', #867, 39.99999999999991473 ) ;
#23773 = CARTESIAN_POINT ( 'NONE',  ( 11.59303701476897253, 18.58252782964011374, -44.86219070953460175 ) ) ;
#23774 = CARTESIAN_POINT ( 'NONE',  ( 199.0054597862206549, 11.64633275074771035, -16.26583636099561403 ) ) ;
#23775 = CARTESIAN_POINT ( 'NONE',  ( -94.58366989427298677, -20.58370269626831117, -9.000605044545542555 ) ) ;
#23776 = CARTESIAN_POINT ( 'NONE',  ( -192.9588430854689989, -8.596193650988133061E-14, 14.46834944099969533 ) ) ;
#23777 = CARTESIAN_POINT ( 'NONE',  ( 192.4448373802100889, 1.051811698935164031E-13, -20.00000000003942091 ) ) ;
#23778 = CARTESIAN_POINT ( 'NONE',  ( -575.0231298121466352, 75.00000000000000000, -35.00000000000203926 ) ) ;
#23779 = CARTESIAN_POINT ( 'NONE',  ( -162.0762913951021176, -1.694272876828353702, 40.00000000000002132 ) ) ;
#23780 = APPLICATION_CONTEXT ( 'automotive_design' ) ;
#23782 = CARTESIAN_POINT ( 'NONE',  ( 180.0000000000000000, -35.78896085774750446, -82.49999999999998579 ) ) ;
#23781 = CARTESIAN_POINT ( 'NONE',  ( -183.6285492668827999, 17.34367427885824142, -41.87133366543424273 ) ) ;
#23783 = CARTESIAN_POINT ( 'NONE',  ( -259.2033419157646676, -6.730120644403663199, 6.730120644403451813 ) ) ;
#23784 = CARTESIAN_POINT ( 'NONE',  ( -91.56559293963834989, -17.32597176626812185, -40.00000000000002132 ) ) ;
#23785 = CARTESIAN_POINT ( 'NONE',  ( 200.0000000000000000, -20.00000000000006750, 40.00000000000002132 ) ) ;
#23786 = CARTESIAN_POINT ( 'NONE',  ( 0.2972598230770103767, -39.99999999999945288, -54.33493731733979359 ) ) ;
#23787 = CARTESIAN_POINT ( 'NONE',  ( -192.9588430854689989, 1.161019517985663313E-13, -14.46834944099969533 ) ) ;
#23788 = LINE ( 'NONE', #1851, #16450 ) ;
#23789 = VERTEX_POINT ( 'NONE', #22473 ) ;
#23790 = DIRECTION ( 'NONE',  ( 0.000000000000000000, -0.3028247695821851271, 0.9530462522498561739 ) ) ;
#23791 = CARTESIAN_POINT ( 'NONE',  ( -208.1127848780265026, 10.60833733269537049, 10.60833733269544510 ) ) ;
#23792 = AXIS2_PLACEMENT_3D ( 'NONE', #14248, #16111, #7854 ) ;
#23793 = CARTESIAN_POINT ( 'NONE',  ( -89.91498783732308198, -8.733585467820335069, 20.17141720494836221 ) ) ;
#23794 = CARTESIAN_POINT ( 'NONE',  ( 0.000000000000000000, 0.000000000000000000, 0.000000000000000000 ) ) ;
#23795 = ORIENTED_EDGE ( 'NONE', *, *, #26073, .F. ) ;
#23796 = ORIENTED_EDGE ( 'NONE', *, *, #5649, .T. ) ;
#23797 = CARTESIAN_POINT ( 'NONE',  ( -238.4067589809705794, -0.6820004457913680929, 0.6820004457913170226 ) ) ;
#23798 = CARTESIAN_POINT ( 'NONE',  ( 147.2817042152898068, 12.35516179550147520, -29.82799917201316475 ) ) ;
#23799 = ORIENTED_EDGE ( 'NONE', *, *, #5333, .F. ) ;
#23800 = CARTESIAN_POINT ( 'NONE',  ( 200.0000000000000000, 19.99999999999996447, -40.00000000000002132 ) ) ;
#23801 = FACE_OUTER_BOUND ( 'NONE', #2167, .T. ) ;
#23802 = VERTEX_POINT ( 'NONE', #16871 ) ;
#23803 = CARTESIAN_POINT ( 'NONE',  ( 199.9999999999997442, -9.911795474730137556, 16.22255894585034852 ) ) ;
#23804 = DIRECTION ( 'NONE',  ( 1.000000000000000000, 1.303213150798907793E-16, 2.465190328815661892E-32 ) ) ;
#23805 = CARTESIAN_POINT ( 'NONE',  ( 19.06497207195980792, 66.60410523465817789, 10.03556273973446800 ) ) ;
#23806 = FACE_OUTER_BOUND ( 'NONE', #3229, .T. ) ;
#23807 = CARTESIAN_POINT ( 'NONE',  ( -213.1075012329537230, -8.703598725189323045E-14, 13.71589010951911902 ) ) ;
#23808 = CARTESIAN_POINT ( 'NONE',  ( 14.33519811653600939, -14.14278418308700758, 49.08818492847921533 ) ) ;
#23809 = DIRECTION ( 'NONE',  ( 0.000000000000000000, 1.000000000000000000, 0.000000000000000000 ) ) ;
#23810 = CYLINDRICAL_SURFACE ( 'NONE', #8436, 10.00000000000000888 ) ;
#23811 = CARTESIAN_POINT ( 'NONE',  ( -100.7734535825088358, -2.560096224687585342E-13, 22.67402823373191723 ) ) ;
#23812 = CARTESIAN_POINT ( 'NONE',  ( -213.1075012329537230, 1.045191102001431893E-13, -13.71589010951911902 ) ) ;
#23813 = CARTESIAN_POINT ( 'NONE',  ( -105.3239292022655320, -10.85048923515416952, 18.46172643730481511 ) ) ;
#23814 = CARTESIAN_POINT ( 'NONE',  ( -259.2033419157646676, -21.55415060305824326, -35.01439189186556433 ) ) ;
#23815 = CARTESIAN_POINT ( 'NONE',  ( 199.9999999999999432, 1.065690307512836407E-13, -20.00000000000010303 ) ) ;
#23816 = CARTESIAN_POINT ( 'NONE',  ( 130.8568914410475088, -32.49135343045460900, -24.07718906446924478 ) ) ;
#23817 = CARTESIAN_POINT ( 'NONE',  ( -93.02511667906883019, 8.169918093965335970, 20.82219708225692401 ) ) ;
#23818 = DIRECTION ( 'NONE',  ( -1.000000000000000000, -1.836970198721030427E-16, 0.000000000000000000 ) ) ;
#23819 = CARTESIAN_POINT ( 'NONE',  ( 57.59792236341146321, 40.00000000000000711, 2.435789363418579434 ) ) ;
#23820 = CARTESIAN_POINT ( 'NONE',  ( 151.7948205124836250, 1.439163438361279259E-13, -33.23291073765553705 ) ) ;
#23821 = CARTESIAN_POINT ( 'NONE',  ( 170.2234770963711128, -17.36149277826995885, 39.20704971665388427 ) ) ;
#23822 = CARTESIAN_POINT ( 'NONE',  ( 136.1360204305621266, -3.511608612531119000, 53.05693388239312469 ) ) ;
#23823 = CARTESIAN_POINT ( 'NONE',  ( -194.4222169614342590, -14.07715596671444658, -48.65437996132243370 ) ) ;
#23824 = CARTESIAN_POINT ( 'NONE',  ( -259.2033419157646676, 6.730120644403521979, -6.730120644403498886 ) ) ;
#23825 = ORIENTED_EDGE ( 'NONE', *, *, #18835, .F. ) ;
#23826 = CARTESIAN_POINT ( 'NONE',  ( -280.0000000000000568, -14.14213562373049449, -42.42640687119305198 ) ) ;
#23827 = DIRECTION ( 'NONE',  ( 0.000000000000000000, 1.000000000000000000, 0.000000000000000000 ) ) ;
#23828 = CARTESIAN_POINT ( 'NONE',  ( -65.65510974524495680, 9.107311025939294424, -24.89665924127712060 ) ) ;
#23829 = CARTESIAN_POINT ( 'NONE',  ( -213.1075012329537230, -18.58567234101102272, -37.98287015391260013 ) ) ;
#23830 = CARTESIAN_POINT ( 'NONE',  ( -82.24465949240999407, 2.525178489058720110, 20.03613703210050545 ) ) ;
#23831 = VERTEX_POINT ( 'NONE', #20599 ) ;
#23832 = VECTOR ( 'NONE', #20127, 1000.000000000000000 ) ;
#23833 = CARTESIAN_POINT ( 'NONE',  ( 199.9999999999999432, 15.97944553385140587, -10.28395956944812362 ) ) ;
#23834 = CARTESIAN_POINT ( 'NONE',  ( 199.0158433542230796, -13.98590299028042772, -14.29668655494494445 ) ) ;
#23835 = CARTESIAN_POINT ( 'NONE',  ( -210.0000000000000284, -66.50000000000001421, -66.50000000000005684 ) ) ;
#23836 = AXIS2_PLACEMENT_3D ( 'NONE', #24089, #6386, #5864 ) ;
#23837 = ORIENTED_EDGE ( 'NONE', *, *, #12728, .F. ) ;
#23838 = EDGE_LOOP ( 'NONE', ( #13428, #25343 ) ) ;
#23839 = CIRCLE ( 'NONE', #19590, 74.99999999999991473 ) ;
#23840 = CARTESIAN_POINT ( 'NONE',  ( -259.2033419157646676, -9.517827891722680178, -40.00000000000002132 ) ) ;
#23841 = CARTESIAN_POINT ( 'NONE',  ( -192.9370379452204816, -44.11033005023536191, -24.26711011077032154 ) ) ;
#23842 = CARTESIAN_POINT ( 'NONE',  ( -100.7734535825088500, 40.00000000000008527, -22.67402823373177512 ) ) ;
#23843 = CARTESIAN_POINT ( 'NONE',  ( -350.0000000000001137, -4.857225732735059864E-14, 0.000000000000000000 ) ) ;
#23844 = B_SPLINE_CURVE_WITH_KNOTS ( 'NONE', 3,
 ( #8703, #14950, #6434, #22946, #18951, #10972, #17079, #20551, #8567, #23085, #16681, #2319, #10706, #10427, #596, #14552, #10835, #19082, #24812, #327, #18816, #12961, #24678, #8429, #16548, #22682, #12551, #20819, #16814, #22815, #20683, #14813, #10563, #25213 ),
 .UNSPECIFIED., .F., .F.,
 ( 4, 2, 2, 2, 2, 2, 2, 2, 2, 2, 2, 2, 2, 2, 2, 2, 4 ),
 ( -5.298243351211008199E-05, 0.01887868273877531602, 0.02834451532491905068, 0.03071097347145496786, 0.03307743161799088505, 0.03544388976452680223, 0.03781034791106271942, 0.04254326420413454685, 0.04727618049720638121, 0.04964263864374229146, 0.05200909679027820171, 0.05674201308334994587, 0.05910847122988582142, 0.06029170030315371409, 0.06147492937642162064, 0.06620784566949321215, 0.07567367825563638128 ),
 .UNSPECIFIED. ) ;
#23845 = LINE ( 'NONE', #19990, #19955 ) ;
#23846 = CARTESIAN_POINT ( 'NONE',  ( -91.56559293963836410, 39.99999999999976552, 22.67402823373234000 ) ) ;
#23847 = DIRECTION ( 'NONE',  ( 0.000000000000000000, 1.000000000000000000, 0.000000000000000000 ) ) ;
#23848 = EDGE_CURVE ( 'NONE', #16014, #15457, #16974, .T. ) ;
#23849 = CARTESIAN_POINT ( 'NONE',  ( -190.0000000000000000, -66.50000000000001421, 66.50000000000005684 ) ) ;
#23850 = CARTESIAN_POINT ( 'NONE',  ( -4.439300432586500200, -23.37136716947730619, -42.88738538954447677 ) ) ;
#23851 = CARTESIAN_POINT ( 'NONE',  ( -30.26275506840325136, 27.08623969584614244, -29.48230279907770779 ) ) ;
#23852 = CARTESIAN_POINT ( 'NONE',  ( 200.0000000000000000, 7.347880794884121511E-14, 0.000000000000000000 ) ) ;
#23853 = CARTESIAN_POINT ( 'NONE',  ( -213.1075012329537230, 1.045191102001431893E-13, -13.71589010951911902 ) ) ;
#23854 = CARTESIAN_POINT ( 'NONE',  ( -105.4288953903223671, -20.05883966465301782, -7.317865678945969954 ) ) ;
#23855 = CARTESIAN_POINT ( 'NONE',  ( -30.26275506840324070, -1.694272468446265112, 0.000000000000000000 ) ) ;
#23856 = CARTESIAN_POINT ( 'NONE',  ( 4.995406935893307754, -55.24977328854835434, -2.449293598294708485E-15 ) ) ;
#23857 = EDGE_CURVE ( 'NONE', #862, #13433, #10173, .T. ) ;
#23858 = CARTESIAN_POINT ( 'NONE',  ( -208.1127848780265026, -10.60833733269551971, 10.60833733269537049 ) ) ;
#23859 = CARTESIAN_POINT ( 'NONE',  ( 146.6084372240433709, 34.62501878078307982, -40.00000000000002132 ) ) ;
#23860 = FACE_OUTER_BOUND ( 'NONE', #10227, .T. ) ;
#23861 = CARTESIAN_POINT ( 'NONE',  ( 151.7948205124836250, -3.202120068677277203E-13, 33.23291073765553705 ) ) ;
#23862 = CARTESIAN_POINT ( 'NONE',  ( 130.8568914410475372, 4.207082182992862407, 4.207082182992856190 ) ) ;
#23863 = EDGE_CURVE ( 'NONE', #6828, #287, #5495, .T. ) ;
#23864 = CARTESIAN_POINT ( 'NONE',  ( 184.8905102610680444, 19.07866798485562043, 2.449293598294708485E-15 ) ) ;
#23865 = ORIENTED_EDGE ( 'NONE', *, *, #18576, .T. ) ;
#23866 = EDGE_CURVE ( 'NONE', #2322, #24112, #7011, .T. ) ;
#23867 = CARTESIAN_POINT ( 'NONE',  ( 22.98934664983286780, -43.11412319250639058, 17.85845455616057720 ) ) ;
#23868 = CIRCLE ( 'NONE', #25606, 5.000000000000004441 ) ;
#23869 = DIRECTION ( 'NONE',  ( 0.000000000000000000, 1.000000000000000000, 0.000000000000000000 ) ) ;
#23870 = CARTESIAN_POINT ( 'NONE',  ( 91.82158438592158234, 16.11829626348434630, -40.45024623143955012 ) ) ;
#23871 = CARTESIAN_POINT ( 'NONE',  ( 146.6084372240433993, 5.715592784339989804E-15, 5.374981219216972583 ) ) ;
#23872 = CARTESIAN_POINT ( 'NONE',  ( 136.1360204305621551, 3.511608612530062512, 53.05693388239318864 ) ) ;
#23873 = CARTESIAN_POINT ( 'NONE',  ( 91.82158438592158234, -1.633484621919921769E-13, 17.20528682183300262 ) ) ;
#23874 = CARTESIAN_POINT ( 'NONE',  ( -162.0762913951020892, 1.694272876828294194, 0.000000000000000000 ) ) ;
#23875 = CARTESIAN_POINT ( 'NONE',  ( -114.4364955367323660, -8.064892380834915997, 20.29001642039123610 ) ) ;
#23876 = CARTESIAN_POINT ( 'NONE',  ( 200.0000000000001137, 4.308913765035643273, 18.51575813813059668 ) ) ;
#23877 = CARTESIAN_POINT ( 'NONE',  ( -77.78761611107495355, 6.817130479269885690, -20.88739660331173198 ) ) ;
#23878 = CARTESIAN_POINT ( 'NONE',  ( -238.4067589809705794, 0.6820004457912851592, -0.6820004457913123597 ) ) ;
#23879 = CARTESIAN_POINT ( 'NONE',  ( 170.2234770963711128, 17.36149277827028925, -39.20704971665377059 ) ) ;
#23880 = CARTESIAN_POINT ( 'NONE',  ( -110.0745364228914838, 19.60339732655324951, -4.981072281427304738 ) ) ;
#23881 = CARTESIAN_POINT ( 'NONE',  ( -77.70933353447252045, 18.93828009115779665, -11.19441472886040145 ) ) ;
#23882 = CARTESIAN_POINT ( 'NONE',  ( 170.2234770963711128, 45.64576402573196390, -10.92277846919159856 ) ) ;
#23884 = CARTESIAN_POINT ( 'NONE',  ( -238.4067589809705794, 0.6820004458491113475, -57.25054294077229144 ) ) ;
#23883 = CARTESIAN_POINT ( 'NONE',  ( 4.995406935893305977, -39.06748935135157552, -39.06748935135225764 ) ) ;
#23885 = CARTESIAN_POINT ( 'NONE',  ( 163.1118516004056573, -19.27778845539181063, -37.29075403953176959 ) ) ;
#23886 = CARTESIAN_POINT ( 'NONE',  ( -210.0000000000000284, 52.50000000000007816, 52.49999999999999289 ) ) ;
#23887 = CARTESIAN_POINT ( 'NONE',  ( 165.3321726438082351, 26.53500608755495094, 0.000000000000000000 ) ) ;
#23888 = SHAPE_REPRESENTATION ( 'MAS-348', ( #25746, #24447, #9156, #16793, #18044, #12984, #9988, #19755, #7023, #13805, #11256, #24013, #19338, #7845, #26153 ), #18956 ) ;
#23890 = CARTESIAN_POINT ( 'NONE',  ( 136.1360204305621551, -40.00000000000001421, 4.966164525586921563 ) ) ;
#23889 = CARTESIAN_POINT ( 'NONE',  ( -91.56559293963834989, 40.53558337403654832, 16.03295912088756481 ) ) ;
#23891 = CARTESIAN_POINT ( 'NONE',  ( 170.2234770963711128, 17.36149277826973503, 39.20704971665401217 ) ) ;
#23892 = CARTESIAN_POINT ( 'NONE',  ( -86.96347745069644475, 15.38646221621772092, 15.38646221621800336 ) ) ;
#23893 = CARTESIAN_POINT ( 'NONE',  ( -91.56559293963834989, -22.67402823373193499, 40.00000000000002132 ) ) ;
#23894 = ORIENTED_EDGE ( 'NONE', *, *, #26226, .F. ) ;
#23895 = CARTESIAN_POINT ( 'NONE',  ( -135.8532207217289738, 50.09629031063965243, -6.472252184284084109 ) ) ;
#23896 = DIRECTION ( 'NONE',  ( 0.000000000000000000, 0.000000000000000000, -1.000000000000000000 ) ) ;
#23897 = CARTESIAN_POINT ( 'NONE',  ( 22.89778847644965154, 17.86913359794376532, 43.13990468001245659 ) ) ;
#23898 = CARTESIAN_POINT ( 'NONE',  ( 98.29820294267359770, -19.33391160836604783, -5.160908283052728862 ) ) ;
#23899 = ORIENTED_EDGE ( 'NONE', *, *, #8523, .F. ) ;
#23900 = CARTESIAN_POINT ( 'NONE',  ( -626.9846540392142060, 90.00000000000000000, 46.18033988749894547 ) ) ;
#23901 = DIRECTION ( 'NONE',  ( 0.000000000000000000, 0.000000000000000000, 1.000000000000000000 ) ) ;
#23902 = CARTESIAN_POINT ( 'NONE',  ( -0.6848998193088060571, -24.09453515733104112, 43.87669161504448567 ) ) ;
#23903 = EDGE_CURVE ( 'NONE', #23932, #16552, #5283, .T. ) ;
#23904 = CARTESIAN_POINT ( 'NONE',  ( 23.41418334855269023, 13.79799959793996678, -46.79369727367426179 ) ) ;
#23905 = CARTESIAN_POINT ( 'NONE',  ( 199.0072281836893637, 3.578240568248503894, -19.67355276342582115 ) ) ;
#23906 = CARTESIAN_POINT ( 'NONE',  ( -77.70103891335998014, -5.501929570351923537, 21.35016180889197557 ) ) ;
#23907 = CARTESIAN_POINT ( 'NONE',  ( 180.0000000000000000, -61.50000000000001421, 66.50000000000005684 ) ) ;
#23908 = CARTESIAN_POINT ( 'NONE',  ( 190.0000000000000000, 52.50000000000007816, -52.49999999999999289 ) ) ;
#23909 = CARTESIAN_POINT ( 'NONE',  ( -56.48582580120559271, 21.81201906317798489, -21.81201906317746619 ) ) ;
#23910 = CARTESIAN_POINT ( 'NONE',  ( 192.4448373802100889, -19.99999999996057198, -2.449293598294708485E-15 ) ) ;
#23912 = PLANE ( 'NONE',  #11294 ) ;
#23911 = CARTESIAN_POINT ( 'NONE',  ( 44.82887508586490100, -12.17256213127418185, -38.96139886160057131 ) ) ;
#23913 = ADVANCED_FACE ( 'NONE', ( #2912 ), #2781, .F. ) ;
#23914 = CARTESIAN_POINT ( 'NONE',  ( -208.1127848780265026, 10.60833733269551615, -10.60833733269529766 ) ) ;
#23915 = CARTESIAN_POINT ( 'NONE',  ( -162.0762913951021176, -1.694272876828353702, -40.00000000000002132 ) ) ;
#23916 = CARTESIAN_POINT ( 'NONE',  ( -198.0356074513804572, 55.37879056871320671, 40.00000000000002132 ) ) ;
#23917 = CARTESIAN_POINT ( 'NONE',  ( 0.2972598230770030492, 5.716321584140269555E-13, -54.33493731733936016 ) ) ;
#23918 = CARTESIAN_POINT ( 'NONE',  ( -210.0000000000000284, 0.000000000000000000, 0.000000000000000000 ) ) ;
#23919 = EDGE_LOOP ( 'NONE', ( #243, #13188, #14347, #8064 ) ) ;
#23920 = CARTESIAN_POINT ( 'NONE',  ( -4.039451493210501454, 43.00522595894040734, -23.44932283416630270 ) ) ;
#23921 = CARTESIAN_POINT ( 'NONE',  ( -135.8532207217289738, -6.472252184284190690, -6.472252184284188914 ) ) ;
#23922 = CARTESIAN_POINT ( 'NONE',  ( 146.6084372240433993, -24.48358557860353457, 24.48358557860296258 ) ) ;
#23923 = CARTESIAN_POINT ( 'NONE',  ( -89.91646883264553480, -8.407637968170137199, 20.29783361038910883 ) ) ;
#23924 = SHAPE_DEFINITION_REPRESENTATION ( #8040, #21040 ) ;
#23925 = ORIENTED_EDGE ( 'NONE', *, *, #20550, .T. ) ;
#23926 = ORIENTED_EDGE ( 'NONE', *, *, #9954, .T. ) ;
#23927 = CARTESIAN_POINT ( 'NONE',  ( -198.0356074513804572, -67.44298959250878056, 10.87444709758448447 ) ) ;
#23928 = CARTESIAN_POINT ( 'NONE',  ( 23.48902902575167673, -46.76665409567426224, -13.79248457097946101 ) ) ;
#23929 = ORIENTED_EDGE ( 'NONE', *, *, #43, .T. ) ;
#23930 = CARTESIAN_POINT ( 'NONE',  ( 19.06497207195980792, 14.19242893257840699, -40.00000000000002132 ) ) ;
#23931 = CARTESIAN_POINT ( 'NONE',  ( -86.86578273022429642, -19.68494377654087657, 8.153770686795153821 ) ) ;
#23932 = VERTEX_POINT ( 'NONE', #1172 ) ;
#23933 = CARTESIAN_POINT ( 'NONE',  ( 199.9999999999998863, 9.495902909754645904, 16.46521490772419583 ) ) ;
#23934 = CARTESIAN_POINT ( 'NONE',  ( -105.2109914857827420, 21.45686921896511734, -1.364328617316883818 ) ) ;
#23935 = CARTESIAN_POINT ( 'NONE',  ( -213.1075012329537230, 37.98287015391228749, 37.98287015391245802 ) ) ;
#23936 = CARTESIAN_POINT ( 'NONE',  ( -105.2276019182101550, -2.726932708308365427, -21.34775691551994115 ) ) ;
#23937 = EDGE_CURVE ( 'NONE', #13337, #2595, #10893, .T. ) ;
#23938 = CARTESIAN_POINT ( 'NONE',  ( 199.9999999999999432, 1.065690307512836407E-13, -20.00000000000010303 ) ) ;
#23939 = CARTESIAN_POINT ( 'NONE',  ( 91.82158438592158234, -17.20528682183298486, 40.00000000000002132 ) ) ;
#23940 = CARTESIAN_POINT ( 'NONE',  ( 57.59792236341147031, -1.722363176414363206, -54.84617931850881689 ) ) ;
#23941 = SPHERICAL_SURFACE ( 'NONE', #8987, 15.00000000000000000 ) ;
#23942 =( REPRESENTATION_RELATIONSHIP ('NONE','NONE', #23888, #14572 ) REPRESENTATION_RELATIONSHIP_WITH_TRANSFORMATION ( #789 )SHAPE_REPRESENTATION_RELATIONSHIP( ) );
#23943 = CARTESIAN_POINT ( 'NONE',  ( -265.0000000000000000, -4.867971026610730343E-14, -6.532754371361504014E-30 ) ) ;
#23944 = CARTESIAN_POINT ( 'NONE',  ( 200.0000000000000000, -39.99999999999977973, -20.00000000000034817 ) ) ;
#23945 = CARTESIAN_POINT ( 'NONE',  ( -105.3901353553839044, -9.627478968556738792, 19.08722479150669571 ) ) ;
#23946 = CARTESIAN_POINT ( 'NONE',  ( -56.48582580120558561, -50.09629031063963112, -6.472252184284449150 ) ) ;
#23947 = EDGE_CURVE ( 'NONE', #13247, #7623, #7204, .T. ) ;
#23948 = CARTESIAN_POINT ( 'NONE',  ( -91.56559293963836410, 22.67402823373190301, -40.00000000000002132 ) ) ;
#23949 = EDGE_CURVE ( 'NONE', #17205, #23049, #8473, .T. ) ;
#23950 = CARTESIAN_POINT ( 'NONE',  ( 192.4448373802101173, -14.14213562370283128, -42.42640687122081999 ) ) ;
#23951 = FACE_OUTER_BOUND ( 'NONE', #13944, .T. ) ;
#23952 = VECTOR ( 'NONE', #15265, 1000.000000000000000 ) ;
#23953 = DIRECTION ( 'NONE',  ( -1.000000000000000000, -0.000000000000000000, -0.000000000000000000 ) ) ;
#23954 = CARTESIAN_POINT ( 'NONE',  ( 91.82158438592158234, -1.633484621919921769E-13, 17.20528682183300262 ) ) ;
#23955 = CARTESIAN_POINT ( 'NONE',  ( -198.0356074513804572, -40.00000000000011369, 15.37879056873056527 ) ) ;
#23956 = CARTESIAN_POINT ( 'NONE',  ( 151.7948205124836250, 4.785054706301690608, 4.785054706301682614 ) ) ;
#23957 = CARTESIAN_POINT ( 'NONE',  ( 91.82158438592156813, -16.11829626348459144, 40.45024623143943643 ) ) ;
#23958 = CARTESIAN_POINT ( 'NONE',  ( -188.8948648269078490, -17.93710299892572380, -43.30399732969062399 ) ) ;
#23959 = CARTESIAN_POINT ( 'NONE',  ( -238.4067589809705794, -28.96627169325313389, -27.60227080167074831 ) ) ;
#23960 = VERTEX_POINT ( 'NONE', #1292 ) ;
#23961 = CARTESIAN_POINT ( 'NONE',  ( 91.82158438592158234, -12.16597498397778843, 12.16597498397750954 ) ) ;
#23962 = CARTESIAN_POINT ( 'NONE',  ( -280.0000000000000000, 14.14213562373098299, -14.14213562373088706 ) ) ;
#23963 = CARTESIAN_POINT ( 'NONE',  ( -280.0000000000000568, 19.99999999999996092, -40.00000000000002132 ) ) ;
#23964 = DIRECTION ( 'NONE',  ( 0.000000000000000000, 0.000000000000000000, 1.000000000000000000 ) ) ;
#23965 = CARTESIAN_POINT ( 'NONE',  ( 136.1360204305621551, -53.05693388239309627, -3.511608612531332163 ) ) ;
#23966 = DIRECTION ( 'NONE',  ( 0.3301743741142292299, 0.000000000000000000, -0.9439199556521077339 ) ) ;
#23967 = EDGE_LOOP ( 'NONE', ( #18305, #22087, #6919, #3888, #6733 ) ) ;
#23968 = CARTESIAN_POINT ( 'NONE',  ( 199.9999999999999432, 18.99425342239354819, -0.6074896776222012962 ) ) ;
#23969 = CARTESIAN_POINT ( 'NONE',  ( 22.68416413276403176, -23.49220544186193038, 43.06288726621021823 ) ) ;
#23970 = CARTESIAN_POINT ( 'NONE',  ( -5.152948516938606005, 13.74948675458142766, 46.60473671797301165 ) ) ;
#23971 = ORIENTED_EDGE ( 'NONE', *, *, #19855, .T. ) ;
#23972 = ORIENTED_EDGE ( 'NONE', *, *, #5719, .T. ) ;
#23973 = PRODUCT_DEFINITION_SHAPE ( 'NONE', 'NONE',  #1112 ) ;
#23974 = CARTESIAN_POINT ( 'NONE',  ( -238.4067589809705794, 0.9644942799825385604, -40.00000000000002132 ) ) ;
#23975 = CARTESIAN_POINT ( 'NONE',  ( -213.1075012329537230, -9.698598906450557777, 9.698598906450415669 ) ) ;
#23976 = CARTESIAN_POINT ( 'NONE',  ( 4.995406935893283773, 39.99999999999997158, 15.24977328854846803 ) ) ;
#23977 = CARTESIAN_POINT ( 'NONE',  ( -93.01741312767285308, -20.82169463880986626, -8.169811846216443740 ) ) ;
#23978 = CARTESIAN_POINT ( 'NONE',  ( 146.6084372240433993, 3.800685668858732935, -3.800685668858610367 ) ) ;
#23979 = CARTESIAN_POINT ( 'NONE',  ( -100.7734535825088358, -2.560096224687585342E-13, 22.67402823373191723 ) ) ;
#23980 = CARTESIAN_POINT ( 'NONE',  ( 199.9999999999998579, -15.18157530797039101, 11.44282300742696457 ) ) ;
#23981 = CARTESIAN_POINT ( 'NONE',  ( 199.0181823811410311, 10.83083347386195427, 16.81793973133765618 ) ) ;
#23982 = CARTESIAN_POINT ( 'NONE',  ( -199.9999999999999432, 43.68705981750494516, 18.09577267661451927 ) ) ;
#23983 = CARTESIAN_POINT ( 'NONE',  ( 9.028290303189734800, -18.59346688788116353, -44.88859993223265832 ) ) ;
#23984 = CARTESIAN_POINT ( 'NONE',  ( 14.38125909742183062, -67.30136555895943218, -10.73282306403629605 ) ) ;
#23985 = CARTESIAN_POINT ( 'NONE',  ( -87.13361725327075646, 15.19799821270843765, 15.19799821270837015 ) ) ;
#23986 = CARTESIAN_POINT ( 'NONE',  ( 192.4448373802101173, -14.14213562370283128, -42.42640687122081999 ) ) ;
#23987 = CARTESIAN_POINT ( 'NONE',  ( -135.8532207217289738, -1.208299557080134822E-13, 9.153146818113572891 ) ) ;
#23988 = CARTESIAN_POINT ( 'NONE',  ( 200.0000000000000000, 7.347880794884121511E-14, 0.000000000000000000 ) ) ;
#23989 = FACE_BOUND ( 'NONE', #21552, .T. ) ;
#23990 = CARTESIAN_POINT ( 'NONE',  ( 4.995406935893309530, -55.24977328856464709, 40.00000000000002132 ) ) ;
#23991 = CARTESIAN_POINT ( 'NONE',  ( 200.0000000000000000, 14.14213562373083022, 42.42640687119289566 ) ) ;
#23992 = CARTESIAN_POINT ( 'NONE',  ( -280.0000000000000000, -20.00000000000006750, -2.449293598294708485E-15 ) ) ;
#23993 = CARTESIAN_POINT ( 'NONE',  ( 98.29820294273055481, 14.14213562373424971, 14.14213562373465294 ) ) ;
#23994 = CARTESIAN_POINT ( 'NONE',  ( -114.5544872014192208, 20.90328437005500817, -6.783945353999890848 ) ) ;
#23995 = CARTESIAN_POINT ( 'NONE',  ( 91.82158438592158234, 16.11829626348434630, -40.45024623143955012 ) ) ;
#23996 = CARTESIAN_POINT ( 'NONE',  ( -91.56559293963834989, -22.67402823373193499, 0.000000000000000000 ) ) ;
#23997 = ORIENTED_EDGE ( 'NONE', *, *, #19220, .F. ) ;
#23998 = CARTESIAN_POINT ( 'NONE',  ( 23.37583784646145091, -46.80752016581931940, 13.80085822091005099 ) ) ;
#23999 = CARTESIAN_POINT ( 'NONE',  ( -114.4364955367323091, -20.29001642039124675, -8.064892380834873364 ) ) ;
#24000 = CARTESIAN_POINT ( 'NONE',  ( 200.0000000000000000, 14.14213562373100608, -42.42640687119291698 ) ) ;
#24001 = CIRCLE ( 'NONE', #7858, 31.79780246617542616 ) ;
#24002 = CARTESIAN_POINT ( 'NONE',  ( 163.1118516004056573, -40.00000000000003553, 12.73709011382460687 ) ) ;
#24003 = AXIS2_PLACEMENT_3D ( 'NONE', #14543, #317, #4446 ) ;
#24004 = CARTESIAN_POINT ( 'NONE',  ( -238.4067589809705794, 0.6820004457912851592, -0.6820004457913123597 ) ) ;
#24005 = DIRECTION ( 'NONE',  ( 0.000000000000000000, 0.3656393565653410227, -0.9307566067079424688 ) ) ;
#24006 = CARTESIAN_POINT ( 'NONE',  ( 19.06497207195980792, 14.19242893257840876, 0.000000000000000000 ) ) ;
#24007 = CARTESIAN_POINT ( 'NONE',  ( -626.9846540392142060, 75.00000000000000000, -54.99999999999995026 ) ) ;
#24008 = CARTESIAN_POINT ( 'NONE',  ( 199.9999999999999716, 18.09021486607068496, 5.826594753398616433 ) ) ;
#24009 = CARTESIAN_POINT ( 'NONE',  ( 199.9999999999999432, -18.36475088389829935, -4.912290392632249869 ) ) ;
#24010 = CARTESIAN_POINT ( 'NONE',  ( 130.8568914410475088, 32.49135343045448820, 24.07718906446946860 ) ) ;
#24011 = CARTESIAN_POINT ( 'NONE',  ( 0.2972598230770153171, -66.70487387989849992, -10.13633138497533004 ) ) ;
#24012 = ADVANCED_FACE ( 'NONE', ( #14868 ), #6886, .T. ) ;
#24013 = AXIS2_PLACEMENT_3D ( 'NONE', #21423, #11060, #13304 ) ;
#24014 = DIRECTION ( 'NONE',  ( -1.000000000000000000, -1.836970198721024264E-16, 0.000000000000000000 ) ) ;
#24015 = CARTESIAN_POINT ( 'NONE',  ( -82.25988539629349816, 17.04081484591361217, -10.82485991171699879 ) ) ;
#24016 = CARTESIAN_POINT ( 'NONE',  ( -91.56559293963834989, 16.03295912088740849, -40.53558337403661938 ) ) ;
#24018 = LINE ( 'NONE', #1682, #13406 ) ;
#24017 = CARTESIAN_POINT ( 'NONE',  ( 184.8905102610680444, -13.49065550809791603, -13.49065550809818781 ) ) ;
#24019 = CARTESIAN_POINT ( 'NONE',  ( -208.1127848780265026, 10.60833733269551615, -10.60833733269529766 ) ) ;
#24020 = CARTESIAN_POINT ( 'NONE',  ( -135.8532207217289738, 6.472252184284186249, -6.472252184284142729 ) ) ;
#24021 = CARTESIAN_POINT ( 'NONE',  ( 199.0154006451087128, 14.87427763521356461, 13.37117338753515305 ) ) ;
#24023 = CARTESIAN_POINT ( 'NONE',  ( 14.38125909742181818, -40.00000000000007816, 15.17850393972619649 ) ) ;
#24022 = CARTESIAN_POINT ( 'NONE',  ( 151.7948205124836250, -23.49921654116371883, 23.49921654116317526 ) ) ;
#24024 = CARTESIAN_POINT ( 'NONE',  ( 199.9999999999999432, -14.14213562373093680, 14.14213562373082311 ) ) ;
#24025 = VECTOR ( 'NONE', #22517, 1000.000000000000000 ) ;
#24026 = CARTESIAN_POINT ( 'NONE',  ( -215.0000000000000284, 71.50000000000002842, -66.50000000000005684 ) ) ;
#24027 = AXIS2_PLACEMENT_3D ( 'NONE', #16756, #5060, #14759 ) ;
#24028 = CARTESIAN_POINT ( 'NONE',  ( 163.1118516004056573, 12.73709011382477918, 40.00000000000002132 ) ) ;
#24029 = VERTEX_POINT ( 'NONE', #20999 ) ;
#24030 = CARTESIAN_POINT ( 'NONE',  ( 14.32711916788068329, -24.71075626504557121, -44.71189734681527739 ) ) ;
#24031 = CARTESIAN_POINT ( 'NONE',  ( 24.02412737066820370, 41.95328616380271569, 17.37762011516664629 ) ) ;
#24032 = CARTESIAN_POINT ( 'NONE',  ( -351.0000000000000568, -4.605747634845933236E-14, -20.53474504356812247 ) ) ;
#24033 = CARTESIAN_POINT ( 'NONE',  ( -105.3755690713226727, -21.75974354311652093, 0.000000000000000000 ) ) ;
#24034 = AXIS2_PLACEMENT_3D ( 'NONE', #4208, #4466, #8440 ) ;
#24035 = ORIENTED_EDGE ( 'NONE', *, *, #11656, .F. ) ;
#24036 = AXIS2_PLACEMENT_3D ( 'NONE', #1684, #3813, #19505 ) ;
#24037 = DIRECTION ( 'NONE',  ( -1.000000000000000000, 1.836970198721030181E-16, 0.000000000000000000 ) ) ;
#24038 = ORIENTED_EDGE ( 'NONE', *, *, #11099, .T. ) ;
#24039 = CARTESIAN_POINT ( 'NONE',  ( 199.9999999999999147, -18.52330518485242195, -4.309840028370497400 ) ) ;
#24040 = AXIS2_PLACEMENT_3D ( 'NONE', #9115, #4880, #14974 ) ;
#24041 = CARTESIAN_POINT ( 'NONE',  ( 16.38602454705575795, -14.09104119325942328, 48.74566733940696395 ) ) ;
#24042 = CARTESIAN_POINT ( 'NONE',  ( 22.92196489051228880, 13.82589419143594611, -46.97629733300941268 ) ) ;
#24043 = CARTESIAN_POINT ( 'NONE',  ( 199.0089689370622352, -1.315408825438062257, -19.96384840600867960 ) ) ;
#24044 = CLOSED_SHELL ( 'NONE', ( #7117, #14681, #13218, #14522, #12243, #23621, #13220, #12560, #2598, #25407, #20880, #11346, #14761, #16623, #1764, #25604, #23687, #3149, #4604, #1819 ) ) ;
#24045 = CARTESIAN_POINT ( 'NONE',  ( -188.2995950289363805, 23.44932284466059969, -43.00522595870931752 ) ) ;
#24046 = CARTESIAN_POINT ( 'NONE',  ( -183.1091233173814317, -22.43565125815695538, 41.47045062403629601 ) ) ;
#24047 =( BOUNDED_SURFACE ( )  B_SPLINE_SURFACE ( 3, 2, ( 
 ( #10404, #6409, #26126 ),
 ( #14526, #15988, #24116 ),
 ( #10010, #26269, #8005 ),
 ( #16122, #4568, #6540 ),
 ( #12664, #436, #25054 ),
 ( #14788, #21051, #23058 ),
 ( #16785, #571, #12524 ),
 ( #24921, #15052, #20791 ),
 ( #9069, #22918, #10677 ),
 ( #8943, #2429, #19181 ),
 ( #17050, #8540, #4697 ),
 ( #12800, #16920, #10810 ),
 ( #8676, #17176, #2835 ),
 ( #20926, #13067, #4960 ),
 ( #2705, #16657, #25185 ),
 ( #6673, #6934, #18920 ) ),
 .UNSPECIFIED., .F., .F., .F. ) 
 B_SPLINE_SURFACE_WITH_KNOTS ( ( 4, 2, 2, 2, 2, 2, 2, 4 ),
 ( 3, 3 ),
 ( 0.04143342415521648198, 0.04844520227998382056, 0.05195109134236748638, 0.05545698040475115220, 0.06246875852951849079, 0.06422170306071033063, 0.06597464759190216355, 0.06948053665428582937 ),
 ( 0.000000000000000000, 1.000000000000000000 ),
 .UNSPECIFIED. ) 
 GEOMETRIC_REPRESENTATION_ITEM ( )  RATIONAL_B_SPLINE_SURFACE ( (
 ( 1.000000000000000000, 0.9541700777564650071, 1.000000000000000000),
 ( 1.000000000000000000, 0.9520170179154711088, 1.000000000000000000),
 ( 1.000000000000000000, 0.9503264940275176764, 1.000000000000000000),
 ( 1.000000000000000000, 0.9485966650353455654, 1.000000000000000000),
 ( 1.000000000000000000, 0.9481601953995637544, 1.000000000000000000),
 ( 1.000000000000000000, 0.9475786562863925955, 1.000000000000000000),
 ( 1.000000000000000000, 0.9474333041674911637, 1.000000000000000000),
 ( 1.000000000000000000, 0.9474385324093995697, 1.000000000000000000),
 ( 1.000000000000000000, 0.9480205960576686408, 1.000000000000000000),
 ( 1.000000000000000000, 0.9494433550397629595, 1.000000000000000000),
 ( 1.000000000000000000, 0.9497628485356935935, 1.000000000000000000),
 ( 1.000000000000000000, 0.9504717112739308194, 1.000000000000000000),
 ( 1.000000000000000000, 0.9508623530679600755, 1.000000000000000000),
 ( 1.000000000000000000, 0.9521262215768991899, 1.000000000000000000),
 ( 1.000000000000000000, 0.9530922057183041085, 1.000000000000000000),
 ( 1.000000000000000000, 0.9541700777564281477, 1.000000000000000000) ) ) 
 REPRESENTATION_ITEM ( '' )  SURFACE ( )  );
#24048 = CARTESIAN_POINT ( 'NONE',  ( 57.59792236341147031, 54.84617931850878136, 1.722363176415705910 ) ) ;
#24049 = CARTESIAN_POINT ( 'NONE',  ( 146.6084372240433709, 34.62501878078307982, 40.00000000000002132 ) ) ;
#24051 = CARTESIAN_POINT ( 'NONE',  ( 151.7948205124836534, 4.785054706297857230, 51.78348778862544322 ) ) ;
#24050 = CARTESIAN_POINT ( 'NONE',  ( -173.7925586254464747, 12.78856870749536512, -41.93433064659100751 ) ) ;
#24052 = DIRECTION ( 'NONE',  ( 4.657398277317546459E-32, -1.682156097916904081E-16, -1.000000000000000000 ) ) ;
#24054 = CARTESIAN_POINT ( 'NONE',  ( -56.48582580120558561, -30.84685318188645553, -40.00000000000002132 ) ) ;
#24053 = VECTOR ( 'NONE', #22996, 1000.000000000000000 ) ;
#24055 = CARTESIAN_POINT ( 'NONE',  ( -162.0762913951021176, 1.694272876828294194, 40.00000000000002132 ) ) ;
#24056 = CARTESIAN_POINT ( 'NONE',  ( -238.4067589809705794, 3.877349844572403567E-13, -40.96449427998260973 ) ) ;
#24057 = CARTESIAN_POINT ( 'NONE',  ( 98.29850319158911987, -8.262390927704235111, 18.22532005579163794 ) ) ;
#24058 = CARTESIAN_POINT ( 'NONE',  ( -280.0000000000000568, 42.42640687119294540, -14.14213562373059041 ) ) ;
#24059 = ORIENTED_EDGE ( 'NONE', *, *, #7756, .T. ) ;
#24060 = CARTESIAN_POINT ( 'NONE',  ( -77.90255099906772784, 20.04994828523968664, -8.644468104261312291 ) ) ;
#24061 = CARTESIAN_POINT ( 'NONE',  ( 0.2972598230769983307, -14.33493731733933352, 0.000000000000000000 ) ) ;
#24062 = CARTESIAN_POINT ( 'NONE',  ( -100.0968563617495590, -8.893120081474123140, 20.41799937592168490 ) ) ;
#24063 = APPLICATION_PROTOCOL_DEFINITION ( 'draft international standard', 'automotive_design', 1998, #22452 ) ;
#24064 = VERTEX_POINT ( 'NONE', #11145 ) ;
#24065 = ORIENTED_EDGE ( 'NONE', *, *, #7189, .F. ) ;
#24066 = CARTESIAN_POINT ( 'NONE',  ( 151.7948205124835681, -4.785054706298153882, -51.78348778862540058 ) ) ;
#24067 = CARTESIAN_POINT ( 'NONE',  ( 23.84827734669235966, -42.71123329578353633, -23.24317830786350214 ) ) ;
#24068 = ORIENTED_EDGE ( 'NONE', *, *, #11594, .T. ) ;
#24069 = CARTESIAN_POINT ( 'NONE',  ( 0.2972598230769930017, 14.33493731733933352, -40.00000000000002132 ) ) ;
#24070 = CARTESIAN_POINT ( 'NONE',  ( -89.91498783733561595, -20.17141720492066170, 8.733585467896798349 ) ) ;
#24071 = ORIENTED_EDGE ( 'NONE', *, *, #388, .T. ) ;
#24072 = CARTESIAN_POINT ( 'NONE',  ( 200.0000000000001421, 18.96284454896564142, 1.255519873078760229 ) ) ;
#24073 = CARTESIAN_POINT ( 'NONE',  ( -105.2501940903818252, 21.20184772653823657, -3.401136913335300438 ) ) ;
#24074 = CARTESIAN_POINT ( 'NONE',  ( 146.6084372240433709, 3.800685668858776900, -52.76785682606518435 ) ) ;
#24075 = CARTESIAN_POINT ( 'NONE',  ( -187.7699188115095694, -42.84915433765046089, -23.34606611631119222 ) ) ;
#24076 = AXIS2_PLACEMENT_3D ( 'NONE', #22002, #4047, #8016 ) ;
#24077 = CIRCLE ( 'NONE', #16853, 5.000000000000004441 ) ;
#24078 = CARTESIAN_POINT ( 'NONE',  ( -56.48582580120557850, -40.00000000000014211, 30.84685318188629921 ) ) ;
#24079 = CARTESIAN_POINT ( 'NONE',  ( 19.06497207195980792, 14.19242893257840699, 40.00000000000002132 ) ) ;
#24080 = CARTESIAN_POINT ( 'NONE',  ( -208.1127848780264742, 10.60833733268383483, -67.17687982760675425 ) ) ;
#24081 = CARTESIAN_POINT ( 'NONE',  ( -93.12335834970889437, -2.546043227727554326E-13, 22.67402823373191723 ) ) ;
#24082 = CARTESIAN_POINT ( 'NONE',  ( 4.995406935893297984, -40.00000000000007816, 15.24977328854818914 ) ) ;
#24083 = CARTESIAN_POINT ( 'NONE',  ( -135.8532207217289738, -40.00000000000014211, 9.153146818113153671 ) ) ;
#24084 = FACE_BOUND ( 'NONE', #7020, .T. ) ;
#24085 = CARTESIAN_POINT ( 'NONE',  ( 184.8905102610680444, -13.49065550809810965, 13.49065550809799596 ) ) ;
#24086 = CARTESIAN_POINT ( 'NONE',  ( 151.7948205124835681, 33.23291073765556547, -40.00000000000002132 ) ) ;
#24087 = CARTESIAN_POINT ( 'NONE',  ( 146.6084372240433709, -3.800685668858344801, -52.76785682606520567 ) ) ;
#24088 = FACE_OUTER_BOUND ( 'NONE', #6437, .T. ) ;
#24089 = CARTESIAN_POINT ( 'NONE',  ( 180.0000000000000000, -35.78896085774753288, -1.496915739050591872E-14 ) ) ;
#24090 = CARTESIAN_POINT ( 'NONE',  ( 160.7895100360998981, 20.14405787076340459, 20.14405787076372434 ) ) ;
#24091 = CARTESIAN_POINT ( 'NONE',  ( 192.4448373802101173, -39.99999999999991473, -20.00000000003956302 ) ) ;
#24092 = CARTESIAN_POINT ( 'NONE',  ( -162.0762913951020892, 57.76657433537918251, 1.198031840455469066 ) ) ;
#24093 = CARTESIAN_POINT ( 'NONE',  ( -114.7569578620488215, 13.65702197131982132, 17.44219256208173974 ) ) ;
#24094 = CARTESIAN_POINT ( 'NONE',  ( -188.6890294954785361, -23.53287096355055752, -43.11788624870519726 ) ) ;
#24095 = CARTESIAN_POINT ( 'NONE',  ( -91.56559293963836410, 16.03295912088714203, -16.03295912088699282 ) ) ;
#24096 = ORIENTED_EDGE ( 'NONE', *, *, #11906, .F. ) ;
#24097 = CARTESIAN_POINT ( 'NONE',  ( -238.4067589809705794, -27.60227080167029001, -28.96627169325357798 ) ) ;
#24098 = LINE ( 'NONE', #7989, #12312 ) ;
#24099 = CARTESIAN_POINT ( 'NONE',  ( 14.38125909742181285, -10.73282306404727393, 10.73282306404716380 ) ) ;
#24100 = DIRECTION ( 'NONE',  ( 0.000000000000000000, 0.000000000000000000, 1.000000000000000000 ) ) ;
#24101 = CIRCLE ( 'NONE', #18519, 15.00000000000000000 ) ;
#24102 = EDGE_CURVE ( 'NONE', #22942, #17673, #2126, .T. ) ;
#24103 = CARTESIAN_POINT ( 'NONE',  ( 170.0000000000000000, -30.00000000000001066, 3.673940397442064700E-15 ) ) ;
#24104 = CARTESIAN_POINT ( 'NONE',  ( 19.06497207195981858, 10.03556273973516078, -66.60410523465806421 ) ) ;
#24105 = CARTESIAN_POINT ( 'NONE',  ( -199.0730705748672449, -18.57195860672538501, -44.83667434817598973 ) ) ;
#24106 = CARTESIAN_POINT ( 'NONE',  ( 190.0000000000000000, 82.50000000000008527, 52.49999999999979394 ) ) ;
#24107 = ORIENTED_EDGE ( 'NONE', *, *, #6969, .T. ) ;
#24108 = CARTESIAN_POINT ( 'NONE',  ( 199.9999999999998863, 15.07162310294758711, 11.58087552627913119 ) ) ;
#24109 = DIRECTION ( 'NONE',  ( 0.000000000000000000, 0.6739498806388349861, 0.7387770694782697101 ) ) ;
#24110 = EDGE_CURVE ( 'NONE', #18109, #11822, #8929, .T. ) ;
#24111 = CARTESIAN_POINT ( 'NONE',  ( -3.993758944537615818, 13.83056263162083610, 47.00698038896962316 ) ) ;
#24112 = VERTEX_POINT ( 'NONE', #4906 ) ;
#24113 = ORIENTED_EDGE ( 'NONE', *, *, #18653, .T. ) ;
#24114 = CARTESIAN_POINT ( 'NONE',  ( -210.0000000000000284, -71.50000000000002842, 66.50000000000005684 ) ) ;
#24115 = CARTESIAN_POINT ( 'NONE',  ( 199.0077026597514021, 2.114100997916472657, -19.88449140175694296 ) ) ;
#24116 = CARTESIAN_POINT ( 'NONE',  ( -114.5514240062852878, 6.817200167027167801, 20.88736325032624919 ) ) ;
#24117 = EDGE_CURVE ( 'NONE', #24643, #17972, #25496, .T. ) ;
#24118 = EDGE_CURVE ( 'NONE', #3746, #3578, #23772, .T. ) ;
#24119 = CARTESIAN_POINT ( 'NONE',  ( 200.0000000000000000, 52.50000000000007816, -52.49999999999999289 ) ) ;
#24120 = CARTESIAN_POINT ( 'NONE',  ( 21.16156876808017273, 43.48822901267212160, -23.80729322913541424 ) ) ;
#24121 = DIRECTION ( 'NONE',  ( 0.9352143323240664774, -0.3271292298997905967, 0.1355013636862025250 ) ) ;
#24122 = CARTESIAN_POINT ( 'NONE',  ( -109.1264249741456211, -33.12752917268984731, 13.72187187124577434 ) ) ;
#24123 = CARTESIAN_POINT ( 'NONE',  ( -635.0400797919774050, 27.64234391852529171, -28.91503648664665960 ) ) ;
#24124 = CARTESIAN_POINT ( 'NONE',  ( -28.75704569508430808, -18.59466133783069708, 35.61514925947740551 ) ) ;
#24125 = CARTESIAN_POINT ( 'NONE',  ( 199.0222638060928375, 2.763249014911820733, 19.81200274180636711 ) ) ;
#24126 = DIRECTION ( 'NONE',  ( -1.000000000000000000, 1.836970198721030181E-16, 0.000000000000000000 ) ) ;
#24127 = CARTESIAN_POINT ( 'NONE',  ( 1.925538622545307943, -14.07631154917879890, -48.64880301057759482 ) ) ;
#24128 = CARTESIAN_POINT ( 'NONE',  ( -238.4067589809705794, -28.96627169325303797, -28.96627169325349627 ) ) ;
#24129 = CARTESIAN_POINT ( 'NONE',  ( -200.0000000000000568, 14.52307781036561352, 48.92947633520088857 ) ) ;
#24130 = CARTESIAN_POINT ( 'NONE',  ( 200.0000000000000000, -14.14213562373062949, -42.42640687119301646 ) ) ;
#24131 = CARTESIAN_POINT ( 'NONE',  ( 184.8905102610680444, -1.851754852062639767E-13, 20.92133201514444352 ) ) ;
#24132 = CARTESIAN_POINT ( 'NONE',  ( 160.9163046357249129, -205.7889608577475542, -55.61140153332243585 ) ) ;
#24133 = CARTESIAN_POINT ( 'NONE',  ( 91.82158438592159655, -22.79471317813468545, -2.449293598294708485E-15 ) ) ;
#24134 = PLANE ( 'NONE',  #4516 ) ;
#24135 = CARTESIAN_POINT ( 'NONE',  ( 19.06497207195982924, -54.19242893257843008, -40.00000000000002132 ) ) ;
#24136 = CARTESIAN_POINT ( 'NONE',  ( -110.0473846051921214, 8.595625304770370789, 18.26116446882227251 ) ) ;
#24137 = CARTESIAN_POINT ( 'NONE',  ( 91.82158438592156813, 39.99999999999986500, 17.20528682183341473 ) ) ;
#24138 = CARTESIAN_POINT ( 'NONE',  ( -86.96347745069644475, -15.38646221621786125, -15.38646221621789856 ) ) ;
#24139 = CARTESIAN_POINT ( 'NONE',  ( 136.1360204305621551, -35.03383547441293899, -40.00000000000002132 ) ) ;
#24140 = ORIENTED_EDGE ( 'NONE', *, *, #7750, .F. ) ;
#24141 = CARTESIAN_POINT ( 'NONE',  ( 23.49666234703823520, -46.76389514419459204, 13.79192166426267363 ) ) ;
#24142 = DIRECTION ( 'NONE',  ( 1.000000000000000000, 1.836970198721030181E-16, 0.000000000000000000 ) ) ;
#24143 = CARTESIAN_POINT ( 'NONE',  ( 146.6084372240433709, 3.800685668858776900, -52.76785682606518435 ) ) ;
#24144 = CARTESIAN_POINT ( 'NONE',  ( 170.2234770963711128, -40.00000000000004263, 15.44714144992801685 ) ) ;
#24145 = CARTESIAN_POINT ( 'NONE',  ( 91.82158438592158234, 16.11829626348378142, 40.45024623143977749 ) ) ;
#24146 = CARTESIAN_POINT ( 'NONE',  ( -198.0356074513804572, 15.37879056873067007, 0.000000000000000000 ) ) ;
#24147 = CARTESIAN_POINT ( 'NONE',  ( 184.8905102610680444, -20.92133201514440799, -40.00000000000002132 ) ) ;
#24148 = CARTESIAN_POINT ( 'NONE',  ( -126.6834156230571011, -24.04426801068274244, -11.16464796290152428 ) ) ;
#24149 = CARTESIAN_POINT ( 'NONE',  ( 199.9999999999998579, 17.67836847945686429, -6.970492097432807732 ) ) ;
#24150 = CARTESIAN_POINT ( 'NONE',  ( 199.9999999999999432, -17.67796534906667816, -6.985163107940991267 ) ) ;
#24151 = CARTESIAN_POINT ( 'NONE',  ( -56.48582580120559271, 21.81201906317798489, -21.81201906317746619 ) ) ;
#24152 = CARTESIAN_POINT ( 'NONE',  ( 14.38125909742183062, -67.30136555895943218, -10.73282306403629605 ) ) ;
#24153 = DIRECTION ( 'NONE',  ( 0.000000000000000000, 0.000000000000000000, -1.000000000000000000 ) ) ;
#24154 = CARTESIAN_POINT ( 'NONE',  ( -77.90255099906775627, 20.04994828523981099, -8.644468104260917940 ) ) ;
#24155 = CARTESIAN_POINT ( 'NONE',  ( 184.8905102610680444, -13.49065550809791603, -13.49065550809818781 ) ) ;
#24156 = DIRECTION ( 'NONE',  ( 0.000000000000000000, 0.000000000000000000, 1.000000000000000000 ) ) ;
#24157 = CARTESIAN_POINT ( 'NONE',  ( -280.0000000000000568, -42.42640687119276066, -14.14213562373147148 ) ) ;
#24158 = CARTESIAN_POINT ( 'NONE',  ( 4.995406935893293543, -10.78321810389005364, 10.78321810388994173 ) ) ;
#24159 = CARTESIAN_POINT ( 'NONE',  ( 199.0158545704749713, 14.28178091326991783, 14.00113215330521221 ) ) ;
#24160 = AXIS2_PLACEMENT_3D ( 'NONE', #22301, #22437, #203 ) ;
#24162 = CARTESIAN_POINT ( 'NONE',  ( 57.59792236341147031, 1.908507979671054758E-14, -2.435789363418160658 ) ) ;
#24161 = CARTESIAN_POINT ( 'NONE',  ( 0.2972598230770011618, 10.13633138497555919, -66.70487387989845729 ) ) ;
#24163 =( BOUNDED_SURFACE ( )  B_SPLINE_SURFACE ( 3, 3, ( 
 ( #26131, #26274, #16400, #12811, #12404, #14403, #8685, #22665, #20933, #6547, #14795, #21059, #4707, #4574, #2572, #712, #10817, #24660, #2712, #16532, #14657, #23065, #6285, #24529, #20529, #444, #22533, #4837, #8816, #4314 ),
 ( #8547, #578, #2300, #16794, #12531, #10409, #16927, #18930, #6417, #18526, #24930, #25061, #6813, #16663, #6680, #14929, #308, #20664, #10686, #22797, #12943, #2845, #10953, #14534, #24795, #8410, #4437, #19059, #8275, #2434 ),
 ( #10546, #18657, #12671, #20800, #18797, #22926, #17183, #17314, #13199, #25446, #973, #17438, #15562, #19436, #9077, #21566, #13446, #21192, #9202, #25193, #3339, #2964, #7198, #13319, #11196, #11440, #23562, #6941, #21321, #21439 ),
 ( #25697, #7321, #15191, #1223, #4968, #15313, #5094, #13077, #23439, #3094, #19189, #21694, #15059, #19310, #841, #11320, #25319, #7077, #5215, #1093, #3214, #23319, #25575, #23686, #9327, #15435, #19562, #1354, #11075, #5337 ),
 ( #11569, #23189, #9453, #17559, #7448, #5465, #13568, #3470, #8951, #17060, #3594, #1476, #24222, #26098, #9582, #2010, #13963, #1, #13700, #8113, #15817, #24723, #3872, #17818, #5594, #9979, #17687, #19956, #22721, #23944 ),
 ( #1739, #9848, #17951, #7706, #7834, #19688, #15957, #19824, #24083, #11836, #5857, #22098, #6479, #11973, #18215, #25966, #25830, #26239, #20098, #14592, #11703, #4007, #10115, #1876, #16229, #5722, #4498, #7574, #12106, #18088 ),
 ( #1610, #7974, #15687, #23812, #21825, #9714, #16092, #13826, #21959, #20231, #3733, #5996, #14102, #22231, #4897, #20731, #13006, #16861, #6606, #21254, #7001, #20857, #16722, #21127, #3027, #23253, #12872, #11011, #15122, #1031 ) ),
 .UNSPECIFIED., .T., .F., .F. ) 
 B_SPLINE_SURFACE_WITH_KNOTS ( ( 4, 3, 4 ),
 ( 4, 2, 2, 2, 2, 2, 2, 2, 2, 2, 2, 2, 2, 2, 4 ),
 ( 0.000000000000000000, 0.5000000000000000000, 1.000000000000000000 ),
 ( 0.000000000000000000, 0.1357259735107005372, 0.1651108541090157700, 0.1944957347073310028, 0.3598804999793158710, 0.3867117631979620773, 0.4135430264166082281, 0.5789277916885930964, 0.6062785021374117456, 0.6336292125862302838, 0.8508620842112317728, 0.8814014469398914198, 0.9119408096685510667, 0.9559704048342755334, 1.000000000000000000 ),
 .UNSPECIFIED. ) 
 GEOMETRIC_REPRESENTATION_ITEM ( )  RATIONAL_B_SPLINE_SURFACE ( (
 ( 1.000000000000000000, 1.000000000000000000, 1.000000000000000000, 1.000000000000000000, 1.000000000000000000, 1.000000000000000000, 1.000000000000000000, 1.000000000000000000, 1.000000000000000000, 1.000000000000000000, 1.000000000000000000, 1.000000000000000000, 1.000000000000000000, 1.000000000000000000, 1.000000000000000000, 1.000000000000000000, 1.000000000000000000, 1.000000000000000000, 1.000000000000000000, 1.000000000000000000, 1.000000000000000000, 1.000000000000000000, 1.000000000000000000, 1.000000000000000000, 1.000000000000000000, 1.000000000000000000, 1.000000000000000000, 1.000000000000000000, 1.000000000000000000, 1.000000000000000000),
 ( 0.3333333333333333703, 0.3333333333333333703, 0.3333333333333333703, 0.3333333333333333703, 0.3333333333333333703, 0.3333333333333333703, 0.3333333333333333703, 0.3333333333333333703, 0.3333333333333333703, 0.3333333333333333703, 0.3333333333333333703, 0.3333333333333333703, 0.3333333333333333703, 0.3333333333333333703, 0.3333333333333333703, 0.3333333333333333703, 0.3333333333333333703, 0.3333333333333333703, 0.3333333333333333703, 0.3333333333333333703, 0.3333333333333333703, 0.3333333333333333703, 0.3333333333333333703, 0.3333333333333333703, 0.3333333333333333703, 0.3333333333333333703, 0.3333333333333333703, 0.3333333333333333703, 0.3333333333333333703, 0.3333333333333333703),
 ( 0.3333333333333333703, 0.3333333333333333703, 0.3333333333333333703, 0.3333333333333333703, 0.3333333333333333703, 0.3333333333333333703, 0.3333333333333333703, 0.3333333333333333703, 0.3333333333333333703, 0.3333333333333333703, 0.3333333333333333703, 0.3333333333333333703, 0.3333333333333333703, 0.3333333333333333703, 0.3333333333333333703, 0.3333333333333333703, 0.3333333333333333703, 0.3333333333333333703, 0.3333333333333333703, 0.3333333333333333703, 0.3333333333333333703, 0.3333333333333333703, 0.3333333333333333703, 0.3333333333333333703, 0.3333333333333333703, 0.3333333333333333703, 0.3333333333333333703, 0.3333333333333333703, 0.3333333333333333703, 0.3333333333333333703),
 ( 1.000000000000000000, 1.000000000000000000, 1.000000000000000000, 1.000000000000000000, 1.000000000000000000, 1.000000000000000000, 1.000000000000000000, 1.000000000000000000, 1.000000000000000000, 1.000000000000000000, 1.000000000000000000, 1.000000000000000000, 1.000000000000000000, 1.000000000000000000, 1.000000000000000000, 1.000000000000000000, 1.000000000000000000, 1.000000000000000000, 1.000000000000000000, 1.000000000000000000, 1.000000000000000000, 1.000000000000000000, 1.000000000000000000, 1.000000000000000000, 1.000000000000000000, 1.000000000000000000, 1.000000000000000000, 1.000000000000000000, 1.000000000000000000, 1.000000000000000000),
 ( 0.3333333333333333703, 0.3333333333333333703, 0.3333333333333333703, 0.3333333333333333703, 0.3333333333333333703, 0.3333333333333333703, 0.3333333333333333703, 0.3333333333333333703, 0.3333333333333333703, 0.3333333333333333703, 0.3333333333333333703, 0.3333333333333333703, 0.3333333333333333703, 0.3333333333333333703, 0.3333333333333333703, 0.3333333333333333703, 0.3333333333333333703, 0.3333333333333333703, 0.3333333333333333703, 0.3333333333333333703, 0.3333333333333333703, 0.3333333333333333703, 0.3333333333333333703, 0.3333333333333333703, 0.3333333333333333703, 0.3333333333333333703, 0.3333333333333333703, 0.3333333333333333703, 0.3333333333333333703, 0.3333333333333333703),
 ( 0.3333333333333333703, 0.3333333333333333703, 0.3333333333333333703, 0.3333333333333333703, 0.3333333333333333703, 0.3333333333333333703, 0.3333333333333333703, 0.3333333333333333703, 0.3333333333333333703, 0.3333333333333333703, 0.3333333333333333703, 0.3333333333333333703, 0.3333333333333333703, 0.3333333333333333703, 0.3333333333333333703, 0.3333333333333333703, 0.3333333333333333703, 0.3333333333333333703, 0.3333333333333333703, 0.3333333333333333703, 0.3333333333333333703, 0.3333333333333333703, 0.3333333333333333703, 0.3333333333333333703, 0.3333333333333333703, 0.3333333333333333703, 0.3333333333333333703, 0.3333333333333333703, 0.3333333333333333703, 0.3333333333333333703),
 ( 1.000000000000000000, 1.000000000000000000, 1.000000000000000000, 1.000000000000000000, 1.000000000000000000, 1.000000000000000000, 1.000000000000000000, 1.000000000000000000, 1.000000000000000000, 1.000000000000000000, 1.000000000000000000, 1.000000000000000000, 1.000000000000000000, 1.000000000000000000, 1.000000000000000000, 1.000000000000000000, 1.000000000000000000, 1.000000000000000000, 1.000000000000000000, 1.000000000000000000, 1.000000000000000000, 1.000000000000000000, 1.000000000000000000, 1.000000000000000000, 1.000000000000000000, 1.000000000000000000, 1.000000000000000000, 1.000000000000000000, 1.000000000000000000, 1.000000000000000000) ) ) 
 REPRESENTATION_ITEM ( '' )  SURFACE ( )  );
#24164 = CARTESIAN_POINT ( 'NONE',  ( -192.9588430854689989, -10.23066800230742501, -10.23066800230756712 ) ) ;
#24165 = CARTESIAN_POINT ( 'NONE',  ( -4.082462733455239245, 42.99255347688239937, -23.44093842354132917 ) ) ;
#24166 = CARTESIAN_POINT ( 'NONE',  ( -91.56559293963834989, 17.32597176626809343, 2.449293598294708485E-15 ) ) ;
#24167 = ORIENTED_EDGE ( 'NONE', *, *, #15616, .F. ) ;
#24168 = CARTESIAN_POINT ( 'NONE',  ( -86.96347745069644475, -15.38646221621786125, -15.38646221621789856 ) ) ;
#24169 = CARTESIAN_POINT ( 'NONE',  ( 6.875206813650288851, 43.66894609317728992, 18.08826972633240970 ) ) ;
#24170 = CARTESIAN_POINT ( 'NONE',  ( -86.86493150571111244, 7.943527260496201947, -19.77569912839169319 ) ) ;
#24171 = FACE_OUTER_BOUND ( 'NONE', #5107, .T. ) ;
#24172 = EDGE_LOOP ( 'NONE', ( #25470, #21845 ) ) ;
#24173 = CARTESIAN_POINT ( 'NONE',  ( -193.3669111531511646, -44.23532963564880305, 18.32287347113157949 ) ) ;
#24174 = CARTESIAN_POINT ( 'NONE',  ( 199.9999999999999716, -14.18957598410689869, 12.65210747703644500 ) ) ;
#24175 = ADVANCED_FACE ( 'NONE', ( #17129 ), #16591, .T. ) ;
#24176 = CARTESIAN_POINT ( 'NONE',  ( 20.38198589868259347, -18.12553405622861646, 43.75891014376981047 ) ) ;
#24177 = B_SPLINE_CURVE_WITH_KNOTS ( 'NONE', 3,
 ( #19118, #10607, #367, #6477, #8470, #18719 ),
 .UNSPECIFIED., .F., .F.,
 ( 4, 2, 4 ),
 ( 3.460613336329060854E-15, 0.03937794852164089310, 0.07875589704327831675 ),
 .UNSPECIFIED. ) ;
#24178 = CARTESIAN_POINT ( 'NONE',  ( 23.30336656375570215, 13.80490921643141355, -46.83484695576438384 ) ) ;
#24179 = CARTESIAN_POINT ( 'NONE',  ( 199.0193324171001450, -17.94164708558885124, -8.847044913458905313 ) ) ;
#24180 = AXIS2_PLACEMENT_3D ( 'NONE', #23493, #23615, #3020 ) ;
#24181 = FACE_OUTER_BOUND ( 'NONE', #16947, .T. ) ;
#24182 = CARTESIAN_POINT ( 'NONE',  ( -144.1957134278176227, -12.48102206790046864, 30.13185274883752740 ) ) ;
#24183 = CARTESIAN_POINT ( 'NONE',  ( -135.8532207217289738, 21.81201906317798134, -21.81201906317747685 ) ) ;
#24184 = CARTESIAN_POINT ( 'NONE',  ( -192.9588430854689989, -14.46834944099973086, 0.000000000000000000 ) ) ;
#24186 = FACE_OUTER_BOUND ( 'NONE', #16653, .T. ) ;
#24185 = CARTESIAN_POINT ( 'NONE',  ( -188.8753834511962566, 17.93496043754537439, -43.29882472894595935 ) ) ;
#24187 = CARTESIAN_POINT ( 'NONE',  ( -91.56559293963836410, 22.67402823373189946, -0.000000000000000000 ) ) ;
#24188 = CARTESIAN_POINT ( 'NONE',  ( 199.9999999999999432, 20.00000000000013856, 0.000000000000000000 ) ) ;
#24189 = CARTESIAN_POINT ( 'NONE',  ( 14.38125909742180752, 15.17850393972634038, 0.000000000000000000 ) ) ;
#24190 = B_SPLINE_CURVE_WITH_KNOTS ( 'NONE', 3,
 ( #18882, #661, #18749, #16884, #21011, #10641, #25148, #4395, #16746, #797, #24879, #21149, #17011, #397 ),
 .UNSPECIFIED., .F., .F.,
 ( 4, 2, 2, 2, 2, 2, 4 ),
 ( 0.0003132551814622137128, 0.004485169056170316450, 0.006571125993524368387, 0.008657082930878422927, 0.01282899680558652854, 0.01491495374294058394, 0.01700091068029464109 ),
 .UNSPECIFIED. ) ;
#24191 = CARTESIAN_POINT ( 'NONE',  ( -213.1075012329537230, -39.99999999999948841, -53.71589010950208376 ) ) ;
#24192 = CARTESIAN_POINT ( 'NONE',  ( -213.1075012329537230, 66.26714140136188291, 9.698598906438215650 ) ) ;
#24193 = CARTESIAN_POINT ( 'NONE',  ( 180.0000000000000284, -125.7889608577475400, 2.115966675574909200E-14 ) ) ;
#24194 = PRODUCT_DEFINITION_SHAPE ( 'NONE', 'NONE',  #26360 ) ;
#24195 = CARTESIAN_POINT ( 'NONE',  ( 57.59792236341147031, 1.722363176415040886, 1.722363176415060426 ) ) ;
#24196 = B_SPLINE_CURVE_WITH_KNOTS ( 'NONE', 3,
 ( #6528, #16909, #20642, #2284, #2549, #22907, #4685, #8797 ),
 .UNSPECIFIED., .F., .F.,
 ( 4, 2, 2, 4 ),
 ( 0.0002291277468225442668, 0.002289782534629433795, 0.004350437322436322835, 0.008471746898050105251 ),
 .UNSPECIFIED. ) ;
#24197 = EDGE_CURVE ( 'NONE', #25714, #2784, #9963, .T. ) ;
#24198 = ORIENTED_EDGE ( 'NONE', *, *, #18927, .T. ) ;
#24199 = CARTESIAN_POINT ( 'NONE',  ( 146.6084372240433993, -24.48358557860319706, -24.48358557860330720 ) ) ;
#24200 = CARTESIAN_POINT ( 'NONE',  ( -100.0968563617643099, -8.149320301498496733, 20.72609133247458146 ) ) ;
#24201 = ORIENTED_EDGE ( 'NONE', *, *, #26318, .F. ) ;
#24202 = ORIENTED_EDGE ( 'NONE', *, *, #5343, .F. ) ;
#24203 = CARTESIAN_POINT ( 'NONE',  ( -100.7734535825088500, -40.53558337403669753, -16.03295912088728770 ) ) ;
#24204 = CARTESIAN_POINT ( 'NONE',  ( 22.92196489051404029, -42.99364193793746836, -23.44087486047875402 ) ) ;
#24205 = ORIENTED_EDGE ( 'NONE', *, *, #17515, .T. ) ;
#24206 = CARTESIAN_POINT ( 'NONE',  ( -280.0000000000000000, -20.00000000000006750, 0.000000000000000000 ) ) ;
#24207 = CARTESIAN_POINT ( 'NONE',  ( -86.86493150571010347, -19.77569912839160082, 7.943527260495840459 ) ) ;
#24208 = VECTOR ( 'NONE', #1266, 1000.000000000000000 ) ;
#24210 = VERTEX_POINT ( 'NONE', #19479 ) ;
#24209 = ADVANCED_FACE ( 'NONE', ( #5873 ), #8257, .F. ) ;
#24211 = CARTESIAN_POINT ( 'NONE',  ( 199.9999999999998010, 4.909892096549036467, 18.36538930945351566 ) ) ;
#24212 = CYLINDRICAL_SURFACE ( 'NONE', #2643, 5.000000000000004441 ) ;
#24213 = CARTESIAN_POINT ( 'NONE',  ( 163.1118516004056573, -19.27778845538761132, -19.27778845538770724 ) ) ;
#24214 = CARTESIAN_POINT ( 'NONE',  ( -166.3490736459090442, -39.29841219601716062, -12.23457872942467972 ) ) ;
#24215 =( BOUNDED_SURFACE ( )  B_SPLINE_SURFACE ( 3, 2, ( 
 ( #24915, #16778, #8669 ),
 ( #565, #10532, #6800 ),
 ( #17044, #4690, #8802 ),
 ( #8397, #6666, #12930 ),
 ( #2423, #25179, #20648 ),
 ( #18645, #430, #290 ),
 ( #8534, #12518, #16519 ),
 ( #24646, #12793, #16651 ),
 ( #4956, #20919, #24781 ),
 ( #16914, #6403, #6533 ),
 ( #21046, #14644, #22650 ),
 ( #22783, #2829, #10938 ) ),
 .UNSPECIFIED., .F., .F., .F. ) 
 B_SPLINE_SURFACE_WITH_KNOTS ( ( 4, 2, 2, 2, 2, 4 ),
 ( 3, 3 ),
 ( 0.006022589392326821271, 0.01254516766564470545, 0.01580645680230364711, 0.01906774593896258876, 0.02559032421228047555, 0.03211290248559835886 ),
 ( 0.000000000000000000, 1.000000000000000000 ),
 .UNSPECIFIED. ) 
 GEOMETRIC_REPRESENTATION_ITEM ( )  RATIONAL_B_SPLINE_SURFACE ( (
 ( 1.000000000000000000, 0.9998834880171258988, 1.000000000000000000),
 ( 1.000000000000000000, 0.9998139205011338237, 1.000000000000000000),
 ( 1.000000000000000000, 0.9997315632445886724, 1.000000000000000000),
 ( 1.000000000000000000, 0.9996405464946352959, 1.000000000000000000),
 ( 1.000000000000000000, 0.9996155081776924023, 1.000000000000000000),
 ( 1.000000000000000000, 0.9995814087511104562, 1.000000000000000000),
 ( 1.000000000000000000, 0.9995724100939918921, 1.000000000000000000),
 ( 1.000000000000000000, 0.9995726760936894939, 1.000000000000000000),
 ( 1.000000000000000000, 0.9996103361816741639, 1.000000000000000000),
 ( 1.000000000000000000, 0.9997312749796802844, 1.000000000000000000),
 ( 1.000000000000000000, 0.9998135910914284219, 1.000000000000000000),
 ( 1.000000000000000000, 0.9998834880173383954, 1.000000000000000000) ) ) 
 REPRESENTATION_ITEM ( '' )  SURFACE ( )  );
#24216 = CARTESIAN_POINT ( 'NONE',  ( -135.8532207217289738, -40.00000000000001421, -9.153146818113709671 ) ) ;
#24217 = CARTESIAN_POINT ( 'NONE',  ( -105.3755690713226585, -21.75974354311652448, 40.00000000000002132 ) ) ;
#24218 = CARTESIAN_POINT ( 'NONE',  ( 170.2234770963711128, -17.36149277826940462, -39.20704971665412586 ) ) ;
#24219 = CARTESIAN_POINT ( 'NONE',  ( 199.0225339954500328, 2.108197227390415929, 19.89250884296043864 ) ) ;
#24220 = CARTESIAN_POINT ( 'NONE',  ( -198.0356074513804572, -40.00000000000011369, 15.37879056873056527 ) ) ;
#24221 = CARTESIAN_POINT ( 'NONE',  ( -86.96347745069643054, -40.00000000000009948, 18.24025645688337960 ) ) ;
#24222 = CARTESIAN_POINT ( 'NONE',  ( -86.96347745069643054, -39.99999999999985079, -18.24025645688394448 ) ) ;
#24223 = CARTESIAN_POINT ( 'NONE',  ( 136.1360204305621551, 40.00000000000017053, -35.03383547441281820 ) ) ;
#24224 = DIRECTION ( 'NONE',  ( -1.000000000000000000, -0.000000000000000000, -0.000000000000000000 ) ) ;
#24225 = CARTESIAN_POINT ( 'NONE',  ( -56.48582580120558561, -21.81201906317785699, 21.81201906317761896 ) ) ;
#24226 = CARTESIAN_POINT ( 'NONE',  ( 14.38125909742181285, -15.17850393972633505, 0.000000000000000000 ) ) ;
#24227 = CARTESIAN_POINT ( 'NONE',  ( 4.995406935893310418, -67.35176059880237176, 10.78321810387813429 ) ) ;
#24228 = CARTESIAN_POINT ( 'NONE',  ( -100.0753760173604121, -8.894334231739641439, 20.41987330121789768 ) ) ;
#24229 = CIRCLE ( 'NONE', #1282, 5.000000000000011546 ) ;
#24230 = CARTESIAN_POINT ( 'NONE',  ( -716.9846540392142060, -66.50000000000001421, -66.50000000000005684 ) ) ;
#24231 = CARTESIAN_POINT ( 'NONE',  ( -105.3755690713226585, 39.99999999999977263, 21.75974354311691883 ) ) ;
#24232 = CARTESIAN_POINT ( 'NONE',  ( -135.8532207217289738, -40.00000000000001421, -9.153146818113709671 ) ) ;
#24233 = CARTESIAN_POINT ( 'NONE',  ( 192.4448373802100889, 14.14213562370310662, 14.14213562370312438 ) ) ;
#24234 = CARTESIAN_POINT ( 'NONE',  ( 184.8905102610680444, -13.49065550809840630, 43.07788698682565354 ) ) ;
#24235 = CARTESIAN_POINT ( 'NONE',  ( -188.8842637254080046, -17.93596642850386758, -43.30125340596359251 ) ) ;
#24236 = CARTESIAN_POINT ( 'NONE',  ( -100.7734535825088500, 16.03295912088713848, -16.03295912088698927 ) ) ;
#24237 = EDGE_LOOP ( 'NONE', ( #10927, #2518, #21176, #5357 ) ) ;
#24238 = CARTESIAN_POINT ( 'NONE',  ( 19.06497207195980792, -18.24870850772710540, -38.31983398719647482 ) ) ;
#24239 = DIRECTION ( 'NONE',  ( 1.000000000000000000, -0.000000000000000000, -0.000000000000000000 ) ) ;
#24240 = CARTESIAN_POINT ( 'NONE',  ( -280.0000000000000000, 19.99999999999996092, -0.000000000000000000 ) ) ;
#24241 = CARTESIAN_POINT ( 'NONE',  ( -87.01524264494790373, 18.58252313551766832, 10.72938103944079380 ) ) ;
#24242 = CARTESIAN_POINT ( 'NONE',  ( -238.4067589809705794, -27.60227080167029001, -28.96627169325357798 ) ) ;
#24243 = DIRECTION ( 'NONE',  ( 0.7071067811865479058, -0.7071067811865472397, 8.659560562354931626E-17 ) ) ;
#24244 = ORIENTED_EDGE ( 'NONE', *, *, #970, .T. ) ;
#24245 = CARTESIAN_POINT ( 'NONE',  ( 199.9999999999999716, 18.74571404017359555, 3.115601181343412573 ) ) ;
#24246 = CARTESIAN_POINT ( 'NONE',  ( -210.0000000000000284, 66.50000000000009948, -66.50000000000005684 ) ) ;
#24247 = CARTESIAN_POINT ( 'NONE',  ( -4.558244102845256940, 23.34817229226072754, 42.85231560262773343 ) ) ;
#24248 = ORIENTED_EDGE ( 'NONE', *, *, #4789, .T. ) ;
#24249 = EDGE_LOOP ( 'NONE', ( #118, #14050, #14381, #2421 ) ) ;
#24250 = CARTESIAN_POINT ( 'NONE',  ( 199.9999999999999432, -20.00000000000006750, 0.000000000000000000 ) ) ;
#24251 = CARTESIAN_POINT ( 'NONE',  ( 199.0112868605082497, -6.441215115722609852, -18.93473387006624620 ) ) ;
#24252 = CARTESIAN_POINT ( 'NONE',  ( -105.2054292637484849, -1.359563962808593374, -21.49321519467867247 ) ) ;
#24253 =( NAMED_UNIT ( * ) SI_UNIT ( $, .STERADIAN. ) SOLID_ANGLE_UNIT ( ) );
#24254 = EDGE_CURVE ( 'NONE', #5362, #2425, #14246, .T. ) ;
#24255 = CARTESIAN_POINT ( 'NONE',  ( -89.91646883263047130, -8.407637968043596643, -20.29783361037425493 ) ) ;
#24256 = CARTESIAN_POINT ( 'NONE',  ( -192.9588430854690273, 40.00000000000014211, -14.46834944099927966 ) ) ;
#24257 = CARTESIAN_POINT ( 'NONE',  ( 98.29850319134099834, 7.044854746987213368, -18.72964005463162351 ) ) ;
#24258 = CARTESIAN_POINT ( 'NONE',  ( 190.0000000000000000, 61.50000000000009948, -66.50000000000005684 ) ) ;
#24259 = CARTESIAN_POINT ( 'NONE',  ( -65.65555754753385997, -11.16466304451101621, 24.04429191298356017 ) ) ;
#24260 = CARTESIAN_POINT ( 'NONE',  ( 199.0220573263155188, 3.250837537642027542, 19.73775173755759127 ) ) ;
#24261 = DIRECTION ( 'NONE',  ( 0.000000000000000000, 0.000000000000000000, 1.000000000000000000 ) ) ;
#24262 = CARTESIAN_POINT ( 'NONE',  ( -2.004660104927048714, -18.09067139730387197, -43.67474423982621801 ) ) ;
#24263 = ADVANCED_FACE ( 'NONE', ( #2154 ), #15605, .F. ) ;
#24264 = CARTESIAN_POINT ( 'NONE',  ( 91.82158438592159655, -44.40256751092341858, 12.16597498400012434 ) ) ;
#24265 = CARTESIAN_POINT ( 'NONE',  ( -114.7826396787321812, -14.66025428929974517, -16.63820106242354058 ) ) ;
#24266 = CARTESIAN_POINT ( 'NONE',  ( -238.4067589809705794, -57.25054294065807881, 0.6820004457338858517 ) ) ;
#24267 = CARTESIAN_POINT ( 'NONE',  ( 192.4448373802100889, -1.741373372144848397E-13, 20.00000000003942091 ) ) ;
#24268 = AXIS2_PLACEMENT_3D ( 'NONE', #3328, #11427, #5204 ) ;
#24269 = CARTESIAN_POINT ( 'NONE',  ( -238.4067589809705794, 27.60227080167080160, -28.96627169325299533 ) ) ;
#24270 = CARTESIAN_POINT ( 'NONE',  ( 146.6084372240433993, -5.374981219216945938, -2.449293598294708485E-15 ) ) ;
#24271 = EDGE_CURVE ( 'NONE', #7299, #12394, #22036, .T. ) ;
#24272 = CARTESIAN_POINT ( 'NONE',  ( -213.1075012329537230, 9.698598906450543566, -9.698598906450348167 ) ) ;
#24273 = AXIS2_PLACEMENT_3D ( 'NONE', #9377, #19488, #11244 ) ;
#24274 = CIRCLE ( 'NONE', #8542, 5.000000000000004441 ) ;
#24275 = CARTESIAN_POINT ( 'NONE',  ( 91.82158438592159655, -22.79471317813468545, -40.00000000000002132 ) ) ;
#24276 = AXIS2_PLACEMENT_3D ( 'NONE', #2249, #14211, #24739 ) ;
#24277 = CARTESIAN_POINT ( 'NONE',  ( -110.0853217340286250, 16.68198050937877497, 11.37485173728495269 ) ) ;
#24278 = CARTESIAN_POINT ( 'NONE',  ( 19.06497207195979726, 40.00000000000017053, -14.19242893257798599 ) ) ;
#24279 = CARTESIAN_POINT ( 'NONE',  ( -198.0356074513804572, 39.15871834505912119, -17.40982414986464377 ) ) ;
#24280 = CARTESIAN_POINT ( 'NONE',  ( -280.0000000000000000, -20.00000000000006750, 0.000000000000000000 ) ) ;
#24281 = EDGE_LOOP ( 'NONE', ( #3615, #5670 ) ) ;
#24282 = ORIENTED_EDGE ( 'NONE', *, *, #13068, .T. ) ;
#24283 = CARTESIAN_POINT ( 'NONE',  ( 170.2234770963711128, -24.55285855007183926, 0.000000000000000000 ) ) ;
#24284 = CARTESIAN_POINT ( 'NONE',  ( 155.1206158682454941, 11.51471166709214877, 27.79897307351034996 ) ) ;
#24285 = CARTESIAN_POINT ( 'NONE',  ( -86.96347745069644475, -8.210974027862429531E-14, 18.24025645688352881 ) ) ;
#24286 = AXIS2_PLACEMENT_3D ( 'NONE', #13397, #15009, #19514 ) ;
#24287 = CARTESIAN_POINT ( 'NONE',  ( 91.82158438592158234, -12.16597498397778843, 12.16597498397750954 ) ) ;
#24288 = CARTESIAN_POINT ( 'NONE',  ( 190.0000000000000000, 66.50000000000009948, 66.50000000000005684 ) ) ;
#24289 = AXIS2_PLACEMENT_3D ( 'NONE', #2436, #14659, #22799 ) ;
#24290 = CARTESIAN_POINT ( 'NONE',  ( 136.1360204305621266, -35.03383547441293899, 0.000000000000000000 ) ) ;
#24291 = EDGE_CURVE ( 'NONE', #2553, #5353, #24098, .T. ) ;
#24292 = DIRECTION ( 'NONE',  ( 0.000000000000000000, -0.3656393565208022056, -0.9307566067254390285 ) ) ;
#24293 = CARTESIAN_POINT ( 'NONE',  ( 199.9999999999999147, 16.22794370004292830, -9.883520089760141403 ) ) ;
#24294 = UNCERTAINTY_MEASURE_WITH_UNIT (LENGTH_MEASURE( 1.000000000000000082E-05 ), #22264, 'distance_accuracy_value', 'NONE');
#24295 = CARTESIAN_POINT ( 'NONE',  ( 199.9999999999999432, -18.14801006015633789, 5.661042778411160548 ) ) ;
#24296 = CARTESIAN_POINT ( 'NONE',  ( 151.7948205124836250, 4.785054706301759886, -4.785054706301612448 ) ) ;
#24297 = CARTESIAN_POINT ( 'NONE',  ( 163.1118516004056573, -9.006482792069506971, -9.006482792069697041 ) ) ;
#24298 = DIRECTION ( 'NONE',  ( 1.000000000000000000, -0.000000000000000000, -0.000000000000000000 ) ) ;
#24299 = CARTESIAN_POINT ( 'NONE',  ( -100.7734535825088358, -2.560096224687585342E-13, 22.67402823373191723 ) ) ;
#24300 = CARTESIAN_POINT ( 'NONE',  ( 4.995406935893312195, -67.35176059882525124, -10.78321810390210445 ) ) ;
#24301 = CARTESIAN_POINT ( 'NONE',  ( -192.9588430854689989, 10.23066800230756712, -10.23066800230735396 ) ) ;
#24302 = CARTESIAN_POINT ( 'NONE',  ( 130.8568914410475088, -24.07718906446864793, -32.49135343045505664 ) ) ;
#24303 = EDGE_CURVE ( 'NONE', #9693, #1564, #18, .T. ) ;
#24304 = CARTESIAN_POINT ( 'NONE',  ( -259.2033419157646676, -49.83842185052031937, -6.730120644403796426 ) ) ;
#24305 = CARTESIAN_POINT ( 'NONE',  ( 199.0233413878889621, 0.01881827774306017026, 20.00361705477971341 ) ) ;
#24307 = CARTESIAN_POINT ( 'NONE',  ( 170.2234770963711128, 40.00000000000000000, 15.44714144992830462 ) ) ;
#24306 = CARTESIAN_POINT ( 'NONE',  ( 170.2234770963711128, 39.20704971665372796, 17.36149277827039583 ) ) ;
#24308 = CARTESIAN_POINT ( 'NONE',  ( -100.7734535825088500, 40.53558337403654832, 16.03295912088756481 ) ) ;
#24309 = AXIS2_PLACEMENT_3D ( 'NONE', #20353, #2129, #10237 ) ;
#24310 = CARTESIAN_POINT ( 'NONE',  ( 21.80824205440350383, 47.36272483143649481, -13.88338701302033051 ) ) ;
#24311 = CARTESIAN_POINT ( 'NONE',  ( -198.0356074513804572, 55.37879056874818673, -40.00000000000002132 ) ) ;
#24312 = ORIENTED_EDGE ( 'NONE', *, *, #19871, .T. ) ;
#24313 = CARTESIAN_POINT ( 'NONE',  ( -208.1127848780265026, 15.00245453012665564, 0.000000000000000000 ) ) ;
#24314 = CARTESIAN_POINT ( 'NONE',  ( -5.304449574935675038, -42.80137191221822235, 17.72890873421427571 ) ) ;
#24315 = APPLICATION_CONTEXT ( 'automotive_design' ) ;
#24316 = CARTESIAN_POINT ( 'NONE',  ( 130.8568914410475372, -34.05028731879786363, 0.000000000000000000 ) ) ;
#24317 = ORIENTED_EDGE ( 'NONE', *, *, #17520, .F. ) ;
#24318 = CARTESIAN_POINT ( 'NONE',  ( -190.5535326093807953, -43.70552662394274535, 18.10342187830013927 ) ) ;
#24319 = CARTESIAN_POINT ( 'NONE',  ( 200.0000000000000853, -18.00470042792477798, 6.107801588486966082 ) ) ;
#24320 = CARTESIAN_POINT ( 'NONE',  ( 17.91733029160310409, -24.32486282486970097, 44.18858371746046743 ) ) ;
#24321 = CARTESIAN_POINT ( 'NONE',  ( 20.91285618074528330, 13.92631245145418895, -47.65039156502910345 ) ) ;
#24322 = CARTESIAN_POINT ( 'NONE',  ( 199.0104473268430922, -4.709499629590884417, -19.43548647772360383 ) ) ;
#24323 = AXIS2_PLACEMENT_3D ( 'NONE', #3191, #25426, #11300 ) ;
#24324 = CARTESIAN_POINT ( 'NONE',  ( -362.0709805440841365, -4.857225732735059864E-14, 0.000000000000000000 ) ) ;
#24325 = FACE_OUTER_BOUND ( 'NONE', #5747, .T. ) ;
#24326 = CARTESIAN_POINT ( 'NONE',  ( 91.82158438592158234, 7.693928927950222250E-14, -17.20528682183300262 ) ) ;
#24327 = CARTESIAN_POINT ( 'NONE',  ( -259.2033419157646676, 21.55415060305860209, -21.55415060305812602 ) ) ;
#24328 = CARTESIAN_POINT ( 'NONE',  ( 146.6084372240433993, 34.62501878078308692, 0.000000000000000000 ) ) ;
#24330 = CARTESIAN_POINT ( 'NONE',  ( -105.3755690713226727, -15.38646221621807619, 15.38646221621768362 ) ) ;
#24329 = CARTESIAN_POINT ( 'NONE',  ( -189.2667921706156449, 17.97629039507469173, -43.39860407294614220 ) ) ;
#24331 = CARTESIAN_POINT ( 'NONE',  ( -280.0000000000000000, -14.14213562373118549, 14.14213562373078936 ) ) ;
#24332 = CARTESIAN_POINT ( 'NONE',  ( 136.1360204305621266, -4.966164525587039691, -2.449293598294708485E-15 ) ) ;
#24333 = CARTESIAN_POINT ( 'NONE',  ( -192.9588430854689989, 54.46834944099968823, 2.449293598294708485E-15 ) ) ;
#24334 = CARTESIAN_POINT ( 'NONE',  ( -280.0000000000000000, 1.605030083646939673E-13, -20.00000000000001421 ) ) ;
#24335 = CARTESIAN_POINT ( 'NONE',  ( 0.2972598230769959993, 38.42060263243659080, 38.42060263243672580 ) ) ;
#24336 = FACE_OUTER_BOUND ( 'NONE', #12690, .T. ) ;
#24337 = CARTESIAN_POINT ( 'NONE',  ( 184.8905102610680444, 14.79361573936375507, 14.79361573936398067 ) ) ;
#24338 = EDGE_LOOP ( 'NONE', ( #5884, #1725, #281, #563 ) ) ;
#24339 = CARTESIAN_POINT ( 'NONE',  ( -105.3755690713226727, -15.38646221621786481, -15.38646221621789856 ) ) ;
#24340 = CARTESIAN_POINT ( 'NONE',  ( -99.31267923333066960, 8.544756979486514581, 20.62886818712721393 ) ) ;
#24341 = ORIENTED_EDGE ( 'NONE', *, *, #22658, .F. ) ;
#24342 = ORIENTED_EDGE ( 'NONE', *, *, #21349, .F. ) ;
#24343 = CARTESIAN_POINT ( 'NONE',  ( -208.1127848780264742, -67.17687982763172272, 10.60833733270744617 ) ) ;
#24344 = CARTESIAN_POINT ( 'NONE',  ( 67.78092418438932043, -29.26022923833890133, -12.11998378862976011 ) ) ;
#24345 = VERTEX_POINT ( 'NONE', #25621 ) ;
#24346 = CARTESIAN_POINT ( 'NONE',  ( -198.0356074513804572, 15.37879056873067007, 0.000000000000000000 ) ) ;
#24347 = FACE_OUTER_BOUND ( 'NONE', #20420, .T. ) ;
#24348 = ORIENTED_EDGE ( 'NONE', *, *, #12164, .T. ) ;
#24349 = CARTESIAN_POINT ( 'NONE',  ( 199.9999999999998863, 14.88114354045644561, 11.82478185164094775 ) ) ;
#24350 = DIRECTION ( 'NONE',  ( -1.000000000000000000, 1.836970198721030181E-16, 0.000000000000000000 ) ) ;
#24351 = CARTESIAN_POINT ( 'NONE',  ( -192.9588430854689989, 10.23066800230742679, 10.23066800230749607 ) ) ;
#24352 = CARTESIAN_POINT ( 'NONE',  ( -188.3120606736146669, -46.99497558484360127, -13.82878088495401236 ) ) ;
#24353 = CARTESIAN_POINT ( 'NONE',  ( -238.4067589809705794, -40.00000000000021316, 40.96449427990166470 ) ) ;
#24354 = CARTESIAN_POINT ( 'NONE',  ( -100.7734535825088358, -22.67402823373193499, 0.000000000000000000 ) ) ;
#24355 = CARTESIAN_POINT ( 'NONE',  ( -280.0000000000000568, -42.42640687119276066, -14.14213562373147148 ) ) ;
#24356 = CARTESIAN_POINT ( 'NONE',  ( 199.0212010157159455, 5.167062836304152640, 19.32642926518865423 ) ) ;
#24357 = CARTESIAN_POINT ( 'NONE',  ( -105.3755690713226585, -39.99999999999996447, -21.75974354311664527 ) ) ;
#24358 = CARTESIAN_POINT ( 'NONE',  ( 170.2234770963711128, -40.00000000000004263, 15.44714144992801685 ) ) ;
#24359 = CARTESIAN_POINT ( 'NONE',  ( -259.2033419157646676, 40.00000000000000711, -9.517827891722491884 ) ) ;
#24360 = CARTESIAN_POINT ( 'NONE',  ( -213.1075012329537230, -13.71589010951915810, -40.00000000000002132 ) ) ;
#24361 = CARTESIAN_POINT ( 'NONE',  ( -105.3755690713226585, -41.18208027870589660, -15.38646221621809040 ) ) ;
#24362 = CARTESIAN_POINT ( 'NONE',  ( -198.0356074513804572, -15.37879056873074290, 0.000000000000000000 ) ) ;
#24363 = CARTESIAN_POINT ( 'NONE',  ( -192.9588430854690273, -38.51493924976932703, -18.05360324515463688 ) ) ;
#24364 = FACE_BOUND ( 'NONE', #13059, .T. ) ;
#24365 = EDGE_CURVE ( 'NONE', #4560, #22478, #14444, .T. ) ;
#24366 = FACE_OUTER_BOUND ( 'NONE', #21271, .T. ) ;
#24367 = CARTESIAN_POINT ( 'NONE',  ( 19.06497207195981147, 1.521599808664285085E-13, -14.19242893257840521 ) ) ;
#24368 = CARTESIAN_POINT ( 'NONE',  ( -105.3755690713226585, -40.00000000000010658, 18.24025645688337249 ) ) ;
#24369 = CARTESIAN_POINT ( 'NONE',  ( 4.995406935893287326, 67.35176059882533650, 10.78321810390163549 ) ) ;
#24370 = CARTESIAN_POINT ( 'NONE',  ( 151.7948205124835681, -4.785054706298876859, 51.78348778862533663 ) ) ;
#24371 = CARTESIAN_POINT ( 'NONE',  ( -188.2507053403081727, -23.43979243030855741, -42.99082124349035183 ) ) ;
#24372 = CARTESIAN_POINT ( 'NONE',  ( 151.7948205124836250, -3.202120068677277203E-13, 33.23291073765553705 ) ) ;
#24373 = EDGE_LOOP ( 'NONE', ( #9636, #9829, #19799, #2198 ) ) ;
#24374 = CARTESIAN_POINT ( 'NONE',  ( -162.0762913951020892, 1.198031840385732849, -1.198031840385733515 ) ) ;
#24375 = CARTESIAN_POINT ( 'NONE',  ( -296.0000000000000000, -4.605747634845933236E-14, -20.53474504356812247 ) ) ;
#24376 = CARTESIAN_POINT ( 'NONE',  ( 163.1118516004056573, 27.26290988616875310, 0.000000000000000000 ) ) ;
#24377 = CARTESIAN_POINT ( 'NONE',  ( 57.59792236341147031, -1.722363176414363206, -54.84617931850881689 ) ) ;
#24378 = LINE ( 'NONE', #17971, #4102 ) ;
#24379 = ORIENTED_EDGE ( 'NONE', *, *, #3532, .T. ) ;
#24380 = CARTESIAN_POINT ( 'NONE',  ( 199.9999999999999716, 16.61865903285387347, -9.211533038762446779 ) ) ;
#24381 = CARTESIAN_POINT ( 'NONE',  ( -105.3841681040951102, -19.11869201644174154, 9.644852623833179095 ) ) ;
#24382 = CARTESIAN_POINT ( 'NONE',  ( -5.787027468459356783, 17.67457596681839860, 42.67020100828666074 ) ) ;
#24383 = ORIENTED_EDGE ( 'NONE', *, *, #6633, .F. ) ;
#24384 = ORIENTED_EDGE ( 'NONE', *, *, #21822, .F. ) ;
#24385 = CARTESIAN_POINT ( 'NONE',  ( 91.82158438592158234, -17.20528682183298486, 0.000000000000000000 ) ) ;
#24386 = CARTESIAN_POINT ( 'NONE',  ( 199.0066734863077897, 5.484006884120094405, -19.23138624862535195 ) ) ;
#24387 = CARTESIAN_POINT ( 'NONE',  ( -114.5516833806003660, -6.814384331921130133, -20.88871136328873845 ) ) ;
#24388 = SURFACE_SIDE_STYLE ('',( #1907 ) ) ;
#24389 = CARTESIAN_POINT ( 'NONE',  ( -102.4309680866877699, -8.087567261546894315, -20.43798635343767245 ) ) ;
#24390 = CARTESIAN_POINT ( 'NONE',  ( -86.96347745069645896, 39.99999999999977973, 21.75974354311691883 ) ) ;
#24391 = AXIS2_PLACEMENT_3D ( 'NONE', #2786, #17263, #11272 ) ;
#24392 = DIRECTION ( 'NONE',  ( -4.625929269271485322E-15, -0.9166903767141219017, 0.3995982397855640800 ) ) ;
#24393 = CARTESIAN_POINT ( 'NONE',  ( -649.4031135302850544, 34.67746518522525179, 19.94086391362369781 ) ) ;
#24394 = DIRECTION ( 'NONE',  ( 0.000000000000000000, 1.000000000000000000, 0.000000000000000000 ) ) ;
#24395 = CARTESIAN_POINT ( 'NONE',  ( 199.0158819412750688, 14.24569456864689343, 14.03872682698725249 ) ) ;
#24396 = DIRECTION ( 'NONE',  ( 0.000000000000000000, 1.000000000000000000, 0.000000000000000000 ) ) ;
#24397 = CARTESIAN_POINT ( 'NONE',  ( 15.76057515058496605, -18.44716516376509929, -44.53539632572822171 ) ) ;
#24398 = CARTESIAN_POINT ( 'NONE',  ( -213.1075012329537230, -66.26714140136188291, -9.698598906438677503 ) ) ;
#24399 = CARTESIAN_POINT ( 'NONE',  ( -93.02511667906868809, 20.50052124204824011, -8.946512270084841845 ) ) ;
#24400 = CARTESIAN_POINT ( 'NONE',  ( 57.59792236341147031, -26.56190807104670171, -30.00663442387710234 ) ) ;
#24401 = DIRECTION ( 'NONE',  ( 0.01051738792036172217, 0.9307051272717591361, -0.3656191332813304995 ) ) ;
#24402 = CARTESIAN_POINT ( 'NONE',  ( 19.06497207195981147, -10.03556273973425483, -10.03556273973443247 ) ) ;
#24403 = CARTESIAN_POINT ( 'NONE',  ( -135.8532207217289454, -30.84685318188649106, 40.00000000000002132 ) ) ;
#24404 = DIRECTION ( 'NONE',  ( -1.836970198721030181E-16, 1.000000000000000000, 0.000000000000000000 ) ) ;
#24405 = CARTESIAN_POINT ( 'NONE',  ( -238.4067589809705794, -40.96449428006345528, 40.00000000000002132 ) ) ;
#24406 = CARTESIAN_POINT ( 'NONE',  ( -105.3881900741214395, 9.658524497639083606, 19.07360370665400495 ) ) ;
#24407 = CARTESIAN_POINT ( 'NONE',  ( -192.9588430854689989, 5.375290060580374156E-13, -54.46834944099972375 ) ) ;
#24408 = CARTESIAN_POINT ( 'NONE',  ( 170.2234770963711128, -17.36149277826985937, -17.36149277826995174 ) ) ;
#24409 = CARTESIAN_POINT ( 'NONE',  ( 200.0000000000000000, 19.99999999999996447, -40.00000000000002132 ) ) ;
#24410 = EDGE_LOOP ( 'NONE', ( #25210, #18379, #24507, #6236, #3686, #8659 ) ) ;
#24411 = EDGE_LOOP ( 'NONE', ( #8705, #14315 ) ) ;
#24412 = ORIENTED_EDGE ( 'NONE', *, *, #8335, .F. ) ;
#24413 = CARTESIAN_POINT ( 'NONE',  ( -86.96347745069644475, -21.75974354311652093, 40.00000000000002132 ) ) ;
#24414 = CARTESIAN_POINT ( 'NONE',  ( -105.4741150117379789, -19.60045294982730724, -8.366608964594114184 ) ) ;
#24415 = CARTESIAN_POINT ( 'NONE',  ( 199.9999999999999432, -3.553951640073651008E-14, 19.99999999999992539 ) ) ;
#24416 = CARTESIAN_POINT ( 'NONE',  ( -198.0356074513804572, 39.15871834505956173, -39.15871834505865223 ) ) ;
#24417 = DIRECTION ( 'NONE',  ( -1.000000000000000000, -1.836970198721030181E-16, 0.000000000000000000 ) ) ;
#24418 = CARTESIAN_POINT ( 'NONE',  ( -716.9846540392142060, -52.49999999999991473, 52.49999999999999289 ) ) ;
#24419 = CARTESIAN_POINT ( 'NONE',  ( -87.12803293485021072, 1.366105440193874143, -21.45672515674945657 ) ) ;
#24420 = CARTESIAN_POINT ( 'NONE',  ( 199.9999999999999432, 17.03543292729471403, 8.423468753378063667 ) ) ;
#24421 = CARTESIAN_POINT ( 'NONE',  ( 199.9999999999999147, -10.82661748099422638, -15.62198329103428840 ) ) ;
#24422 = CARTESIAN_POINT ( 'NONE',  ( 200.0000000000000000, 42.42640687119267540, 14.14213562373153543 ) ) ;
#24423 = CARTESIAN_POINT ( 'NONE',  ( 136.1360204305621266, -3.511608612530630058, -3.511608612530719764 ) ) ;
#24424 = CARTESIAN_POINT ( 'NONE',  ( -280.0000000000000000, -5.143516556418885689E-14, 0.000000000000000000 ) ) ;
#24425 = CARTESIAN_POINT ( 'NONE',  ( -198.0356074513804572, 40.00000000000014921, -15.37879056873028816 ) ) ;
#24426 = CARTESIAN_POINT ( 'NONE',  ( 19.06497207195982924, -66.60410523465809263, -10.03556273973493163 ) ) ;
#24427 = CARTESIAN_POINT ( 'NONE',  ( -210.0000000000000000, -82.49999999999991473, -52.49999999999977973 ) ) ;
#24428 = CARTESIAN_POINT ( 'NONE',  ( -162.0762913951021176, -27.08623940707624911, 29.48230308784761888 ) ) ;
#24429 = CARTESIAN_POINT ( 'NONE',  ( -162.0762913951020892, -57.76657433524000851, 1.198031840315820329 ) ) ;
#24430 = CARTESIAN_POINT ( 'NONE',  ( 199.0233313290092383, 0.04621523056493160447, 20.00358013886366138 ) ) ;
#24432 = CARTESIAN_POINT ( 'NONE',  ( -162.0762913951020892, 39.99999999999985079, 41.69427287692695216 ) ) ;
#24431 = CARTESIAN_POINT ( 'NONE',  ( 57.59792236341147031, 54.84617931850878136, 1.722363176415705910 ) ) ;
#24433 = CARTESIAN_POINT ( 'NONE',  ( 136.1360204305621551, 3.511608612530062512, 53.05693388239318864 ) ) ;
#24434 = CARTESIAN_POINT ( 'NONE',  ( 22.90311673803743986, 46.98314248934284620, -13.82691048574049475 ) ) ;
#24435 = CARTESIAN_POINT ( 'NONE',  ( 151.7948205124836534, 6.767089262349062828, -40.00000000000002132 ) ) ;
#24436 = ORIENTED_EDGE ( 'NONE', *, *, #25095, .T. ) ;
#24437 = CARTESIAN_POINT ( 'NONE',  ( -91.56559293963834989, -22.67402823373193499, 0.000000000000000000 ) ) ;
#24438 = EDGE_CURVE ( 'NONE', #6965, #19453, #10130, .T. ) ;
#24439 = CARTESIAN_POINT ( 'NONE',  ( -4.915070467874388171, -46.68718905935042329, 13.76630780994306846 ) ) ;
#24440 = CARTESIAN_POINT ( 'NONE',  ( -259.2033419157646676, 30.48217210827734647, 40.00000000000002132 ) ) ;
#24441 = VERTEX_POINT ( 'NONE', #20113 ) ;
#24442 = CARTESIAN_POINT ( 'NONE',  ( -109.1264249741463459, 33.12752917270373132, -13.72187187121062557 ) ) ;
#24443 = CARTESIAN_POINT ( 'NONE',  ( 200.0000000000000284, -19.00889450552964988, -0.1561390237190347086 ) ) ;
#24444 = CARTESIAN_POINT ( 'NONE',  ( -3.786831587087837736, -13.84155926340451970, 47.08106124085753663 ) ) ;
#24445 = ADVANCED_FACE ( 'NONE', ( #9370 ), #22113, .T. ) ;
#24446 = EDGE_CURVE ( 'NONE', #6051, #61, #20824, .T. ) ;
#24447 = AXIS2_PLACEMENT_3D ( 'NONE', #955, #17299, #25557 ) ;
#24448 = CARTESIAN_POINT ( 'NONE',  ( -0.1993645192496782403, 18.24262160100998997, -44.04158448241128099 ) ) ;
#24449 = CARTESIAN_POINT ( 'NONE',  ( 199.0139917666041924, -11.25641580849352685, -16.53121693397544689 ) ) ;
#24451 = B_SPLINE_CURVE_WITH_KNOTS ( 'NONE', 3,
 ( #25736, #13355, #9243, #13606, #17597, #17350 ),
 .UNSPECIFIED., .F., .F.,
 ( 4, 2, 4 ),
 ( -6.000000000996541667E-08, 0.04016968416332604430, 0.08033942832665208478 ),
 .UNSPECIFIED. ) ;
#24450 = CARTESIAN_POINT ( 'NONE',  ( -314.0000000000000568, -4.857225732735059864E-14, 0.000000000000000000 ) ) ;
#24452 = LINE ( 'NONE', #22461, #13853 ) ;
#24453 = CARTESIAN_POINT ( 'NONE',  ( -86.86493150571111244, 8.366608963953098055, -19.60045294882791467 ) ) ;
#24454 = CARTESIAN_POINT ( 'NONE',  ( -238.4067589809705794, 0.6820004458491113475, -57.25054294077229144 ) ) ;
#24455 = CARTESIAN_POINT ( 'NONE',  ( 192.4448373802100889, 20.00000000003945644, 0.000000000000000000 ) ) ;
#24456=STYLED_ITEM('',(#26409),#8871);
#24458 = CARTESIAN_POINT ( 'NONE',  ( 151.7948205124836250, -23.49921654116371883, 23.49921654116317526 ) ) ;
#24457 = CARTESIAN_POINT ( 'NONE',  ( -188.3611024622299510, 13.83140737835798895, -47.01268868735313333 ) ) ;
#24459 = CARTESIAN_POINT ( 'NONE',  ( -105.3755690713226585, 41.18208027870575449, 15.38646221621837107 ) ) ;
#24460 = CARTESIAN_POINT ( 'NONE',  ( -135.8532207217289454, -30.84685318188649106, 40.00000000000002132 ) ) ;
#24461 = CARTESIAN_POINT ( 'NONE',  ( -135.8532207217289738, 30.84685318188643777, -40.00000000000002132 ) ) ;
#24462 = CARTESIAN_POINT ( 'NONE',  ( -238.4067589809705794, -40.00000000000005684, -0.9644942799830014124 ) ) ;
#24463 = CARTESIAN_POINT ( 'NONE',  ( 170.2234770963711128, -17.36149277826995885, 39.20704971665388427 ) ) ;
#24464 = CARTESIAN_POINT ( 'NONE',  ( 98.29820294267328507, -5.160908283042997091, 19.33391160836888290 ) ) ;
#24465 = CARTESIAN_POINT ( 'NONE',  ( -280.0000000000000568, 14.14213562373127431, -42.42640687119274645 ) ) ;
#24466 = EDGE_LOOP ( 'NONE', ( #3985, #17418, #18413, #1930 ) ) ;
#24467 = CARTESIAN_POINT ( 'NONE',  ( 170.2234770963711128, -17.36149277826985937, -17.36149277826995174 ) ) ;
#24468 = AXIS2_PLACEMENT_3D ( 'NONE', #420, #24771, #24903 ) ;
#24469 = VECTOR ( 'NONE', #7738, 1000.000000000000000 ) ;
#24470 = B_SPLINE_CURVE_WITH_KNOTS ( 'NONE', 3,
 ( #3847, #7811, #1325, #15927, #1454, #25552, #9555, #17663 ),
 .UNSPECIFIED., .F., .F.,
 ( 4, 2, 2, 4 ),
 ( 0.0002291277466117084692, 0.002289782534329003541, 0.004350437322046298017, 0.008471746897480886968 ),
 .UNSPECIFIED. ) ;
#24471 = CARTESIAN_POINT ( 'NONE',  ( -94.58360650945733994, 8.190527749687760206, 20.91945674502158070 ) ) ;
#24472 = APPLICATION_PROTOCOL_DEFINITION ( 'draft international standard', 'automotive_design', 1998, #10201 ) ;
#24473 = ORIENTED_EDGE ( 'NONE', *, *, #13064, .T. ) ;
#24474 = VERTEX_POINT ( 'NONE', #25745 ) ;
#24475 = CARTESIAN_POINT ( 'NONE',  ( -192.9588430854690273, -38.51493924976932703, -18.05360324515463688 ) ) ;
#24476 = CARTESIAN_POINT ( 'NONE',  ( 16.38602454699764976, -44.43226271089463353, -24.50452114743870169 ) ) ;
#24477 = ORIENTED_EDGE ( 'NONE', *, *, #15793, .F. ) ;
#24478 = CARTESIAN_POINT ( 'NONE',  ( -89.92902785008656963, -20.44110050034138126, 8.088236460649854465 ) ) ;
#24479 = DIRECTION ( 'NONE',  ( 0.000000000000000000, -0.3995982397418283427, -0.9166903767331869846 ) ) ;
#24480 = EDGE_LOOP ( 'NONE', ( #8891, #3318, #23086, #6565 ) ) ;
#24481 = CARTESIAN_POINT ( 'NONE',  ( 199.9999999999998579, 17.78360892267977178, 6.705045715290576247 ) ) ;
#24482 = AXIS2_PLACEMENT_3D ( 'NONE', #15448, #3228, #11452 ) ;
#24483 = CARTESIAN_POINT ( 'NONE',  ( -397.9898987322331436, -3.637015436189069562E-14, 0.000000000000000000 ) ) ;
#24484 = CARTESIAN_POINT ( 'NONE',  ( 4.995406935893289102, 10.78321810388998081, 10.78321810389001811 ) ) ;
#24485 = CARTESIAN_POINT ( 'NONE',  ( -151.7004448984925773, -32.50164219295758983, -13.46262099560747139 ) ) ;
#24486 = CARTESIAN_POINT ( 'NONE',  ( 136.1360204305621551, -40.00000000000001421, 4.966164525586921563 ) ) ;
#24487 = CARTESIAN_POINT ( 'NONE',  ( 199.9999999999999432, -20.00000000000006750, 0.000000000000000000 ) ) ;
#24488 = CARTESIAN_POINT ( 'NONE',  ( 200.0000000000000000, -42.42640687119272513, -14.14213562373140753 ) ) ;
#24489 = CARTESIAN_POINT ( 'NONE',  ( 199.0216355752872914, 4.216131936211398035, 19.55614661669859444 ) ) ;
#24490 = CIRCLE ( 'NONE', #25758, 29.99999999999999645 ) ;
#24491 = CARTESIAN_POINT ( 'NONE',  ( -208.1127848780264742, -40.00000000000025580, 55.00245453014408525 ) ) ;
#24492 = CARTESIAN_POINT ( 'NONE',  ( -198.0356074513804572, -40.00000000000025580, 55.37879056871310013 ) ) ;
#24493 = CARTESIAN_POINT ( 'NONE',  ( 170.2234770963711128, 40.00000000000000000, 15.44714144992830462 ) ) ;
#24494 = CARTESIAN_POINT ( 'NONE',  ( 0.2972598230769983307, -14.33493731733933352, -40.00000000000002132 ) ) ;
#24495 = CARTESIAN_POINT ( 'NONE',  ( 14.38125909742183062, -67.30136555898262429, 10.73282306405838682 ) ) ;
#24496 = CARTESIAN_POINT ( 'NONE',  ( -86.96347745069645896, 21.75974354311648895, -40.00000000000002132 ) ) ;
#24497 = CARTESIAN_POINT ( 'NONE',  ( 184.8905102610680444, 14.79361573936366092, 41.77492675556006674 ) ) ;
#24498 = CARTESIAN_POINT ( 'NONE',  ( -238.4067589809705794, -3.369206980223063916E-14, -0.9644942799825824142 ) ) ;
#24499 = FACE_BOUND ( 'NONE', #16244, .T. ) ;
#24500 = CARTESIAN_POINT ( 'NONE',  ( 4.995406935893298872, 5.820775922023080204E-13, -55.24977328854835434 ) ) ;
#24501 = CARTESIAN_POINT ( 'NONE',  ( 91.82158438592159655, -40.00000000000008527, 22.79471317813456110 ) ) ;
#24502 = CARTESIAN_POINT ( 'NONE',  ( -162.0762913951021176, 29.48230308784768638, -27.08623940707612121 ) ) ;
#24503 = AXIS2_PLACEMENT_3D ( 'NONE', #659, #10363, #16612 ) ;
#24504 = CARTESIAN_POINT ( 'NONE',  ( 180.0000000000000000, 6.980486755139914804E-14, 0.000000000000000000 ) ) ;
#24505 = DIRECTION ( 'NONE',  ( 0.000000000000000000, 1.000000000000000000, 0.000000000000000000 ) ) ;
#24506 = CARTESIAN_POINT ( 'NONE',  ( 146.6084372240433709, -3.800685668858344801, -52.76785682606520567 ) ) ;
#24507 = ORIENTED_EDGE ( 'NONE', *, *, #49, .T. ) ;
#24508 = CARTESIAN_POINT ( 'NONE',  ( -280.0000000000000568, -42.42640687119276066, -14.14213562373147148 ) ) ;
#24509 = DIRECTION ( 'NONE',  ( -0.000000000000000000, -1.000000000000000000, -0.000000000000000000 ) ) ;
#24510 = CARTESIAN_POINT ( 'NONE',  ( 19.06497207195982924, -54.19242893257843008, -2.449293598294708485E-15 ) ) ;
#24511 = CARTESIAN_POINT ( 'NONE',  ( 23.37394308801977871, 23.33966569535068203, 42.85717664514594816 ) ) ;
#24512 = CARTESIAN_POINT ( 'NONE',  ( -91.56559293963834989, -16.03295912088728414, 16.03295912088688269 ) ) ;
#24513 =( NAMED_UNIT ( * ) PLANE_ANGLE_UNIT ( ) SI_UNIT ( $, .RADIAN. ) );
#24514 = EDGE_LOOP ( 'NONE', ( #14130, #14356, #5083, #22210, #652, #2426, #25718, #18075, #23825, #13618, #23302, #19173, #19328, #15047, #13848 ) ) ;
#24515 = ORIENTED_EDGE ( 'NONE', *, *, #10595, .F. ) ;
#24516 = CARTESIAN_POINT ( 'NONE',  ( 199.9999999999999147, 7.543773257828894074, 17.44673522875667615 ) ) ;
#24517 = CARTESIAN_POINT ( 'NONE',  ( -53.37769371738607305, -13.65853730965327806, -27.95780717557944328 ) ) ;
#24518 = CARTESIAN_POINT ( 'NONE',  ( 22.82148508083373883, 17.87803012130506275, 43.16138278737005862 ) ) ;
#24519 = ORIENTED_EDGE ( 'NONE', *, *, #3774, .T. ) ;
#24520 = AXIS2_PLACEMENT_3D ( 'NONE', #13831, #5599, #14109 ) ;
#24521 = ORIENTED_EDGE ( 'NONE', *, *, #24699, .F. ) ;
#24522 = CARTESIAN_POINT ( 'NONE',  ( -135.8532207217289738, -9.153146818113595984, 0.000000000000000000 ) ) ;
#24523 = CARTESIAN_POINT ( 'NONE',  ( 199.0122387307937686, -8.258478517853962586, -18.21619819090958714 ) ) ;
#24524 = CARTESIAN_POINT ( 'NONE',  ( -190.1760717700867360, -43.55712811731331158, 23.85870456434319209 ) ) ;
#24525 = CARTESIAN_POINT ( 'NONE',  ( 169.9999999999999716, -125.7889608577475116, 82.50000000000001421 ) ) ;
#24526 = EDGE_CURVE ( 'NONE', #17301, #13098, #3890, .T. ) ;
#24527 = CARTESIAN_POINT ( 'NONE',  ( 5.009866156928143077, 44.71726210619370079, -24.71463403307565088 ) ) ;
#24528 = CARTESIAN_POINT ( 'NONE',  ( 163.1118516004056573, 39.99999999999976552, 27.26290988616914746 ) ) ;
#24529 = CARTESIAN_POINT ( 'NONE',  ( 146.6084372240433993, -3.357462877844280890E-13, 34.62501878078305850 ) ) ;
#24530 = CARTESIAN_POINT ( 'NONE',  ( -656.7096227442339114, 39.79407741042334834, -4.181560688537802051 ) ) ;
#24531 = FACE_OUTER_BOUND ( 'NONE', #831, .T. ) ;
#24532 = CARTESIAN_POINT ( 'NONE',  ( 199.0244464070843833, -3.263486543644114946, 19.73887645897787735 ) ) ;
#24533 = CARTESIAN_POINT ( 'NONE',  ( -188.9524464570897635, 13.86227157644379915, 47.22058047019342553 ) ) ;
#24534 = CARTESIAN_POINT ( 'NONE',  ( 23.38399212876534250, -13.80022400692441842, -46.80460545930682059 ) ) ;
#24535 = CARTESIAN_POINT ( 'NONE',  ( 130.8568914410475372, -4.207082182992785135, -4.207082182992884611 ) ) ;
#24536 = AXIS2_PLACEMENT_3D ( 'NONE', #24132, #12021, #18134 ) ;
#24537 = CARTESIAN_POINT ( 'NONE',  ( -30.26275506840324070, -29.48230279907780016, -27.08623969584605362 ) ) ;
#24538 = CARTESIAN_POINT ( 'NONE',  ( -210.0000000000000284, 66.50000000000009948, -66.50000000000005684 ) ) ;
#24539 = CARTESIAN_POINT ( 'NONE',  ( 146.6084372240433993, 24.48358557860307272, 24.48358557860347418 ) ) ;
#24540 = CARTESIAN_POINT ( 'NONE',  ( 91.82158438592156813, 17.20528682183302038, 40.00000000000002132 ) ) ;
#24541 = CARTESIAN_POINT ( 'NONE',  ( 192.4448373802100889, 14.14213562375893574, -14.14213562375874922 ) ) ;
#24542 = AXIS2_PLACEMENT_3D ( 'NONE', #8897, #15142, #15013 ) ;
#24543 = CARTESIAN_POINT ( 'NONE',  ( -86.96347745069643054, -18.24025645688353947, 40.00000000000002132 ) ) ;
#24544 = CARTESIAN_POINT ( 'NONE',  ( -110.1022965999516003, 13.49625447730847938, 15.07957642757643413 ) ) ;
#24545 = CARTESIAN_POINT ( 'NONE',  ( -30.26275506840324425, 40.00000000000044764, -41.69427246844585255 ) ) ;
#24546 = CARTESIAN_POINT ( 'NONE',  ( 192.4448373802100889, -14.14213562375876698, -14.14213562375885047 ) ) ;
#24547 = EDGE_CURVE ( 'NONE', #19647, #22653, #13031, .T. ) ;
#24548 = CARTESIAN_POINT ( 'NONE',  ( -192.9588430854690273, 14.46834944099966336, -40.00000000000002132 ) ) ;
#24549 = ORIENTED_EDGE ( 'NONE', *, *, #16629, .T. ) ;
#24550 = ORIENTED_EDGE ( 'NONE', *, *, #16145, .T. ) ;
#24551 = CARTESIAN_POINT ( 'NONE',  ( -77.90255099906767100, -8.064892378658175431, 20.29001641120675004 ) ) ;
#24552 = CARTESIAN_POINT ( 'NONE',  ( -105.4741150117390021, -7.943527260764932763, -19.77569912954469800 ) ) ;
#24553 = CARTESIAN_POINT ( 'NONE',  ( 151.7948205124836534, 33.06932595376333239, 23.49921654116065284 ) ) ;
#24554 = CARTESIAN_POINT ( 'NONE',  ( -114.5444905533601343, -20.85462941671032766, -6.798574478272650268 ) ) ;
#24555 = DIRECTION ( 'NONE',  ( 1.000000000000000000, 1.836970198721030181E-16, 0.000000000000000000 ) ) ;
#24556 = DIRECTION ( 'NONE',  ( 1.000000000000000000, 1.836970198721030427E-16, -0.000000000000000000 ) ) ;
#24557 = CARTESIAN_POINT ( 'NONE',  ( 199.9999999999998863, 15.61930985130600291, 10.83040361559445230 ) ) ;
#24558 = CARTESIAN_POINT ( 'NONE',  ( 200.0000000000000000, -10.30695654162946795, -15.96943722719255199 ) ) ;
#24559 = CARTESIAN_POINT ( 'NONE',  ( -105.3755690713226585, 41.18208027870575449, 15.38646221621837107 ) ) ;
#24560 = CARTESIAN_POINT ( 'NONE',  ( -100.7734535825088500, -12.25131212657524316, 44.31723036834888774 ) ) ;
#24561 = PLANE ( 'NONE',  #12695 ) ;
#24562 = CARTESIAN_POINT ( 'NONE',  ( 163.1118516004056573, 39.99999999999976552, 27.26290988616914746 ) ) ;
#24563 = CARTESIAN_POINT ( 'NONE',  ( -56.48582580120559982, -21.81201906317804173, 34.75652343174591152 ) ) ;
#24564 = CARTESIAN_POINT ( 'NONE',  ( -265.0000000000000000, -4.857225732735059864E-14, 0.000000000000000000 ) ) ;
#24565 = CARTESIAN_POINT ( 'NONE',  ( -105.3755690713226727, -15.38646221621786481, -15.38646221621789856 ) ) ;
#24566 = CARTESIAN_POINT ( 'NONE',  ( 184.8905102610680444, 14.79361573936396113, -14.79361573936377461 ) ) ;
#24567 = CARTESIAN_POINT ( 'NONE',  ( 199.0233077721956647, 0.1102320784427082423, 20.00336233838309496 ) ) ;
#24569 = CARTESIAN_POINT ( 'NONE',  ( 136.1360204305621266, 5.219216885335291329E-15, 4.966164525587064560 ) ) ;
#24568 = CARTESIAN_POINT ( 'NONE',  ( 192.4448373802101173, 42.42640687116487896, 14.14213562375934075 ) ) ;
#24570 = CARTESIAN_POINT ( 'NONE',  ( -162.0762913951021176, 29.48230308784730980, 27.08623940707652622 ) ) ;
#24571 = CARTESIAN_POINT ( 'NONE',  ( 23.42154907652877327, 46.79103593565408659, -13.79745687233748441 ) ) ;
#24572 = CARTESIAN_POINT ( 'NONE',  ( 170.2234770963711128, 15.44714144992819094, 2.449293598294708485E-15 ) ) ;
#24573 = FACE_OUTER_BOUND ( 'NONE', #20580, .T. ) ;
#24574 = CARTESIAN_POINT ( 'NONE',  ( 0.2972598230769938343, 10.13633138497472252, 10.13633138497475628 ) ) ;
#24575 = CARTESIAN_POINT ( 'NONE',  ( -3.439026802539349781, -43.30533194338908487, 17.93765581402033149 ) ) ;
#24576 = CARTESIAN_POINT ( 'NONE',  ( 4.995406935893288214, 55.24977328854835434, 2.449293598294708485E-15 ) ) ;
#24577 = EDGE_LOOP ( 'NONE', ( #22525, #15044, #11556, #6832 ) ) ;
#24578 = DIRECTION ( 'NONE',  ( 1.000000000000000000, 0.000000000000000000, 0.000000000000000000 ) ) ;
#24579 = CARTESIAN_POINT ( 'NONE',  ( -192.9588430854689989, 10.23066800230742679, 10.23066800230749607 ) ) ;
#24580 = FACE_BOUND ( 'NONE', #21642, .T. ) ;
#24581 = CARTESIAN_POINT ( 'NONE',  ( -3.336279363872681536, 17.94861674415367148, -43.33179396957144291 ) ) ;
#24582 = CARTESIAN_POINT ( 'NONE',  ( 199.0100048860339541, -3.743224330709818748, -19.64425440907078269 ) ) ;
#24583 = CARTESIAN_POINT ( 'NONE',  ( -4.039451493210481026, -46.99046209229796034, -13.82811171175467102 ) ) ;
#24584 = CARTESIAN_POINT ( 'NONE',  ( 144.9504669809063557, -30.13886470195709322, 12.48392651407819187 ) ) ;
#24586 = AXIS2_PLACEMENT_3D ( 'NONE', #3092, #17685, #23684 ) ;
#24585 = CARTESIAN_POINT ( 'NONE',  ( -190.0144721488334767, -13.91469502169458394, 47.57279682960911771 ) ) ;
#24587 = EDGE_CURVE ( 'NONE', #20259, #2697, #18104, .T. ) ;
#24588 = CARTESIAN_POINT ( 'NONE',  ( 4.995406935893294431, -17.50105314357144337, -39.06748935135212264 ) ) ;
#24589 = CARTESIAN_POINT ( 'NONE',  ( 184.8905102610680444, 20.92133201514447549, 0.000000000000000000 ) ) ;
#24591 = CARTESIAN_POINT ( 'NONE',  ( -198.0356074513804572, 39.15871834505887250, 17.40982414986519089 ) ) ;
#24590 = CARTESIAN_POINT ( 'NONE',  ( -188.8948648269078774, 17.93710299892656934, -43.30399732969019055 ) ) ;
#24592 = CARTESIAN_POINT ( 'NONE',  ( 146.6084372240433993, -24.48358557860353457, 24.48358557860296258 ) ) ;
#24593 = CARTESIAN_POINT ( 'NONE',  ( 0.2972598230770129857, -54.33493731733938148, 40.00000000000002132 ) ) ;
#24594 = CARTESIAN_POINT ( 'NONE',  ( -162.0762913951021176, 41.69427287672986182, 40.00000000000002132 ) ) ;
#24595 = EDGE_CURVE ( 'NONE', #3578, #21399, #22248, .T. ) ;
#24596 = CARTESIAN_POINT ( 'NONE',  ( 200.0000000000000000, -40.00000000000019185, 19.99999999999968381 ) ) ;
#24597 = CARTESIAN_POINT ( 'NONE',  ( -100.7734535825088358, 12.25131212657480440, 12.25131212657487012 ) ) ;
#24598 = CARTESIAN_POINT ( 'NONE',  ( -93.01741312764252712, 20.50009083229532436, -8.946232117619326019 ) ) ;
#24599 = CARTESIAN_POINT ( 'NONE',  ( -280.0000000000000000, -14.14213562373088706, -14.14213562373108424 ) ) ;
#24600 = EDGE_CURVE ( 'NONE', #26151, #5117, #9334, .T. ) ;
#24601 = CARTESIAN_POINT ( 'NONE',  ( -114.4364955367323660, -8.064892380834915997, 20.29001642039123610 ) ) ;
#24602 = EDGE_CURVE ( 'NONE', #9554, #15971, #5515, .T. ) ;
#24603 = ORIENTED_EDGE ( 'NONE', *, *, #9770, .F. ) ;
#24604 = CARTESIAN_POINT ( 'NONE',  ( 146.6084372240433709, -52.76785682606516303, 3.800685668858563737 ) ) ;
#24605 = CARTESIAN_POINT ( 'NONE',  ( -100.0968563617859530, 8.149320301543554024, 20.72609133245155988 ) ) ;
#24606 = CARTESIAN_POINT ( 'NONE',  ( -56.48582580120558561, -21.81201906317785699, 21.81201906317761896 ) ) ;
#24607 = CARTESIAN_POINT ( 'NONE',  ( 17.91733029160166168, -44.18858371746068769, -24.32486282486966545 ) ) ;
#24608 = ORIENTED_EDGE ( 'NONE', *, *, #20698, .T. ) ;
#24609 = CARTESIAN_POINT ( 'NONE',  ( -188.2995950289365226, 23.44932284465886241, 43.00522595870971543 ) ) ;
#24610 = CARTESIAN_POINT ( 'NONE',  ( -77.70093066171460805, -11.20685550411562303, -18.98763857597440818 ) ) ;
#24611 = AXIS2_PLACEMENT_3D ( 'NONE', #21475, #3376, #15469 ) ;
#24612 = ORIENTED_EDGE ( 'NONE', *, *, #9011, .F. ) ;
#24613 = CARTESIAN_POINT ( 'NONE',  ( 200.0000000000001705, 5.211075256460824257, -18.27473396828003871 ) ) ;
#24614 = CARTESIAN_POINT ( 'NONE',  ( -296.0000000000000000, -4.857225732735059864E-14, 0.000000000000000000 ) ) ;
#24615 = CARTESIAN_POINT ( 'NONE',  ( -86.96347745069644475, -15.38646221621786125, -15.38646221621789856 ) ) ;
#24616 = CARTESIAN_POINT ( 'NONE',  ( -189.2667921706087952, -43.39860407294495559, -17.97629039507308590 ) ) ;
#24617 = CARTESIAN_POINT ( 'NONE',  ( 130.8568914410475088, -39.99999999999988631, -34.05028731879802706 ) ) ;
#24618 = CARTESIAN_POINT ( 'NONE',  ( 136.1360204305621266, 4.966164525587089429, 2.449293598294708485E-15 ) ) ;
#24619 = CARTESIAN_POINT ( 'NONE',  ( 91.82158438592158234, -12.16597498397778843, 12.16597498397750954 ) ) ;
#24620 = CARTESIAN_POINT ( 'NONE',  ( 199.0248683625651154, -4.715036670046848677, 19.44145415004932076 ) ) ;
#24621 = CARTESIAN_POINT ( 'NONE',  ( -192.9588430854690273, -40.00000000000011369, 14.46834944099955855 ) ) ;
#24622 = CARTESIAN_POINT ( 'NONE',  ( -30.26275506840325136, 40.00000000000001421, 1.694272468446399227 ) ) ;
#24623 = CARTESIAN_POINT ( 'NONE',  ( -351.0000000000000568, -4.857225732735059864E-14, -20.53474504356812247 ) ) ;
#24624 = CARTESIAN_POINT ( 'NONE',  ( 151.7948205124836250, 33.23291073765556547, 0.000000000000000000 ) ) ;
#24625 = CARTESIAN_POINT ( 'NONE',  ( 170.2234770963711128, -15.44714144992812699, -40.00000000000002132 ) ) ;
#24626 = CARTESIAN_POINT ( 'NONE',  ( 91.82158438592159655, -16.11829626346147393, 16.11829626346132116 ) ) ;
#24627 = CARTESIAN_POINT ( 'NONE',  ( -192.9588430854689989, 1.161019517985663313E-13, -14.46834944099969533 ) ) ;
#24628 = CARTESIAN_POINT ( 'NONE',  ( -190.0000000000000000, -52.49999999999991473, 52.49999999999999289 ) ) ;
#24629 = CARTESIAN_POINT ( 'NONE',  ( -213.1075012329537230, 5.259461644596141978E-13, -53.71589010951915100 ) ) ;
#24630 = CARTESIAN_POINT ( 'NONE',  ( 19.06497207195982924, -40.00000000000021316, 54.19242893257830218 ) ) ;
#24631 = CARTESIAN_POINT ( 'NONE',  ( 184.8905102610680444, -14.79361573936379415, -14.79361573936387941 ) ) ;
#24632 = LINE ( 'NONE', #6390, #9639 ) ;
#24633 = CARTESIAN_POINT ( 'NONE',  ( -114.7823189589623780, -14.64951506473200737, 16.64646944814565543 ) ) ;
#24634 = CARTESIAN_POINT ( 'NONE',  ( 163.1118516004056573, -9.006482792073960297, -47.56205970284963769 ) ) ;
#24635 = ADVANCED_FACE ( 'NONE', ( #685 ), #25039, .F. ) ;
#24636 = ORIENTED_EDGE ( 'NONE', *, *, #25270, .T. ) ;
#24637 = CARTESIAN_POINT ( 'NONE',  ( -4.580761711668102087, 42.99740816077407857, -17.81010960708308843 ) ) ;
#24638 = DIRECTION ( 'NONE',  ( -1.000000000000000000, 0.000000000000000000, 0.000000000000000000 ) ) ;
#24639 = CARTESIAN_POINT ( 'NONE',  ( 57.59792236341148453, -37.56421063658185489, -2.449293598294708485E-15 ) ) ;
#24640 = CIRCLE ( 'NONE', #25087, 10.00000000000004796 ) ;
#24641 = CARTESIAN_POINT ( 'NONE',  ( -86.94949953272045207, -6.679047987426590893, -20.30809431151271127 ) ) ;
#24642 = CARTESIAN_POINT ( 'NONE',  ( -238.4067589809705794, 0.9644942799825386714, 0.000000000000000000 ) ) ;
#24643 = VERTEX_POINT ( 'NONE', #283 ) ;
#24644 = ORIENTED_EDGE ( 'NONE', *, *, #7803, .T. ) ;
#24645 = CARTESIAN_POINT ( 'NONE',  ( -97.72675010090222258, 8.987772175319644674, -20.56394680065910308 ) ) ;
#24646 = CARTESIAN_POINT ( 'NONE',  ( -94.58360650936646152, 8.190527749686246750, -20.91945674502226282 ) ) ;
#24647 = CARTESIAN_POINT ( 'NONE',  ( 21.80824205439611774, 23.67346680102962608, 43.30754100652750083 ) ) ;
#24648 = EDGE_LOOP ( 'NONE', ( #2732, #4552, #16149, #729, #24644 ) ) ;
#24649 = ORIENTED_EDGE ( 'NONE', *, *, #23617, .T. ) ;
#24650 = PRODUCT_DEFINITION_SHAPE ( 'NONE', 'NONE',  #26364 ) ;
#24651 = CARTESIAN_POINT ( 'NONE',  ( -213.1075012329537230, 13.71589010951907994, 0.000000000000000000 ) ) ;
#24652 = CARTESIAN_POINT ( 'NONE',  ( 199.0103724725597658, -4.548822225537863417, -19.47368150598642345 ) ) ;
#24653 = CARTESIAN_POINT ( 'NONE',  ( -105.2272259197136322, -2.713789710689835655, -21.35019349091949792 ) ) ;
#24654 = DIRECTION ( 'NONE',  ( -5.494191223143503443E-14, 0.7071067811865585639, -0.7071067811865364705 ) ) ;
#24655 = CARTESIAN_POINT ( 'NONE',  ( -192.9588430854690273, 38.51493924976939098, -18.05360324515436687 ) ) ;
#24656 = CARTESIAN_POINT ( 'NONE',  ( -199.9999999999999147, -22.35311919176581696, 45.06067021511796611 ) ) ;
#24657 = CARTESIAN_POINT ( 'NONE',  ( 14.32711916788066553, 44.71189734681538397, -24.71075626504571687 ) ) ;
#24658 = VECTOR ( 'NONE', #18235, 1000.000000000000000 ) ;
#24659 = CARTESIAN_POINT ( 'NONE',  ( -105.3755690713226727, 1.741486606973311632E-13, -18.24025645688352881 ) ) ;
#24660 = CARTESIAN_POINT ( 'NONE',  ( 14.38125909742181108, 1.616281842095393922E-13, -15.17850393972633682 ) ) ;
#24661 = CARTESIAN_POINT ( 'NONE',  ( -629.5670837480076898, 26.57842901870468211, 29.89303253829147167 ) ) ;
#24662 = FACE_OUTER_BOUND ( 'NONE', #24577, .T. ) ;
#24663 = CARTESIAN_POINT ( 'NONE',  ( 199.0106735244355320, 19.32142130491951804, 5.196343561012195522 ) ) ;
#24664 = CARTESIAN_POINT ( 'NONE',  ( -188.2870673237720496, 23.44688076656433751, 43.00153493964062790 ) ) ;
#24665 = CARTESIAN_POINT ( 'NONE',  ( 184.8905102610680444, -13.49065550809840630, 43.07788698682565354 ) ) ;
#24666 = B_SPLINE_CURVE_WITH_KNOTS ( 'NONE', 3,
 ( #16558, #335, #10045, #20558, #18150, #8303 ),
 .UNSPECIFIED., .F., .F.,
 ( 4, 2, 4 ),
 ( -6.000000014155440701E-08, 0.03937727993095193474, 0.07875461986190401831 ),
 .UNSPECIFIED. ) ;
#24667 = CARTESIAN_POINT ( 'NONE',  ( -200.0000000000000000, -69.99999999999998579, 8.572527594031471415E-15 ) ) ;
#24668 = CARTESIAN_POINT ( 'NONE',  ( 91.82158438592156813, 40.45024623143950038, 16.11829626348447420 ) ) ;
#24669 = DIRECTION ( 'NONE',  ( 0.000000000000000000, 1.000000000000000000, 0.000000000000000000 ) ) ;
#24670 = CARTESIAN_POINT ( 'NONE',  ( 4.995406935893300648, -10.78321810387790514, -67.35176059880241439 ) ) ;
#24671 = CARTESIAN_POINT ( 'NONE',  ( -644.6571494263627073, 33.34084698429052196, 30.23100662976579045 ) ) ;
#24672 = CARTESIAN_POINT ( 'NONE',  ( -192.9588430854689989, -14.46834944099973086, 0.000000000000000000 ) ) ;
#24673 = CARTESIAN_POINT ( 'NONE',  ( 165.3321726438350368, 18.76308274332837911, -18.76308274332814818 ) ) ;
#24674 = CARTESIAN_POINT ( 'NONE',  ( -162.0762913951020892, -1.694272876828353702, 0.000000000000000000 ) ) ;
#24675 = CARTESIAN_POINT ( 'NONE',  ( -618.7358282227124846, 29.45763196998035127, -34.01907996191106065 ) ) ;
#24676 = CARTESIAN_POINT ( 'NONE',  ( 4.995406935893291767, 40.00000000000059686, -55.24977328853165659 ) ) ;
#24677 = CARTESIAN_POINT ( 'NONE',  ( 199.0129030236711003, -9.437255757388491872, -17.63982070750089548 ) ) ;
#24678 = CARTESIAN_POINT ( 'NONE',  ( 151.0853911467766011, -12.04115959308015960, 29.06993079631205390 ) ) ;
#24679 = VERTEX_POINT ( 'NONE', #25171 ) ;
#24680 = ORIENTED_EDGE ( 'NONE', *, *, #4973, .F. ) ;
#24681 = CARTESIAN_POINT ( 'NONE',  ( -100.7734535825088358, -22.67402823373193499, 0.000000000000000000 ) ) ;
#24682 = CARTESIAN_POINT ( 'NONE',  ( 159.7744820660628591, 10.75261058663732960, 25.95909830917690186 ) ) ;
#24683 = CARTESIAN_POINT ( 'NONE',  ( 14.38125909742180397, 67.30136555898270956, -10.73282306405792319 ) ) ;
#24684 = CARTESIAN_POINT ( 'NONE',  ( 98.29820294267337033, 18.47759065023124236, -7.653668647303903505 ) ) ;
#24685 = EDGE_CURVE ( 'NONE', #20012, #22608, #24640, .T. ) ;
#24686 = CARTESIAN_POINT ( 'NONE',  ( -199.9999999999999716, -49.28189405767602693, 14.17215463606940595 ) ) ;
#24687 = CARTESIAN_POINT ( 'NONE',  ( 200.0000000000000000, -59.99999999999992184, 0.000000000000000000 ) ) ;
#24688 = CARTESIAN_POINT ( 'NONE',  ( 200.0000000000002558, -1.250172057809772586, -18.97074946354465652 ) ) ;
#24689 = EDGE_CURVE ( 'NONE', #25953, #4298, #12737, .T. ) ;
#24690 = CARTESIAN_POINT ( 'NONE',  ( 199.9999999999999147, 10.29454322937508159, -15.97255386245730691 ) ) ;
#24691 = VECTOR ( 'NONE', #12502, 1000.000000000000000 ) ;
#24692 = CARTESIAN_POINT ( 'NONE',  ( -259.2033419157646676, -35.01439189186523748, -21.55415060305881170 ) ) ;
#24693 = CARTESIAN_POINT ( 'NONE',  ( 184.8905102610680444, -13.49065550809840630, 43.07788698682565354 ) ) ;
#24694 = CARTESIAN_POINT ( 'NONE',  ( -114.4627503397241384, 20.42543059692667029, 7.807380225631771253 ) ) ;
#24695 = CARTESIAN_POINT ( 'NONE',  ( -105.3755690713226585, 39.99999999999977263, 21.75974354311691883 ) ) ;
#24696 = CARTESIAN_POINT ( 'NONE',  ( 19.06497207195981858, -38.31983398719641087, 18.24870850772724040 ) ) ;
#24697 = CARTESIAN_POINT ( 'NONE',  ( 5.009865950673426660, 14.14399394884953409, 49.09576456953139001 ) ) ;
#24698 = FACE_OUTER_BOUND ( 'NONE', #23539, .T. ) ;
#24699 = EDGE_CURVE ( 'NONE', #8490, #13725, #14858, .T. ) ;
#24700 = CARTESIAN_POINT ( 'NONE',  ( 57.59792236341147031, -26.56190807104670171, -30.00663442387710234 ) ) ;
#24701 = CARTESIAN_POINT ( 'NONE',  ( 199.0083531997975967, 19.99451597160352989, -0.2840371431019264592 ) ) ;
#24702 = ADVANCED_FACE ( 'NONE', ( #820 ), #10797, .T. ) ;
#24704 = CARTESIAN_POINT ( 'NONE',  ( 192.4448373802101173, -40.00000000000005684, 19.99999999996046185 ) ) ;
#24703 = CARTESIAN_POINT ( 'NONE',  ( -135.8532207217289738, 21.81201906317798134, -21.81201906317747685 ) ) ;
#24705 = CARTESIAN_POINT ( 'NONE',  ( -259.2033419157646676, 49.83842185052017015, 6.730120644404137487 ) ) ;
#24706 = CARTESIAN_POINT ( 'NONE',  ( 20.69615274308407393, 43.59383154590945963, -23.88537831999326855 ) ) ;
#24707 = CARTESIAN_POINT ( 'NONE',  ( 14.38125909742180752, 55.17850393971008316, -40.00000000000002132 ) ) ;
#24708 = CARTESIAN_POINT ( 'NONE',  ( -91.56559293963834989, -16.03295912088706388, -16.03295912088710651 ) ) ;
#24709 = CARTESIAN_POINT ( 'NONE',  ( 184.8905102610680444, -20.92133201514440799, 0.000000000000000000 ) ) ;
#24710 = CARTESIAN_POINT ( 'NONE',  ( -77.90022806218901508, -20.16431395584850250, 8.352332316461128059 ) ) ;
#24711 = AXIS2_PLACEMENT_3D ( 'NONE', #7267, #5411, #13512 ) ;
#24712 = CARTESIAN_POINT ( 'NONE',  ( 14.38125909742180752, 55.17850393974265444, 40.00000000000002132 ) ) ;
#24713 = VERTEX_POINT ( 'NONE', #18774 ) ;
#24714 = CARTESIAN_POINT ( 'NONE',  ( 23.30631261066140780, 23.35506702543256097, -42.87793822514780828 ) ) ;
#24715 = AXIS2_PLACEMENT_3D ( 'NONE', #24324, #13567, #3593 ) ;
#24716 = CARTESIAN_POINT ( 'NONE',  ( -208.1127848780264742, -17.67593391476659548, 38.89260858015730804 ) ) ;
#24717 = CARTESIAN_POINT ( 'NONE',  ( -16.37606550806344785, -16.46709356867778595, 39.75508062653803876 ) ) ;
#24718 = CARTESIAN_POINT ( 'NONE',  ( 11.71430589688568169, 14.17293196763019303, -49.28686712666840464 ) ) ;
#24719 = CARTESIAN_POINT ( 'NONE',  ( 199.0253131443098766, -18.94683372192476156, 6.427280041807147626 ) ) ;
#24720 = LINE ( 'NONE', #6476, #14296 ) ;
#24721 = DIRECTION ( 'NONE',  ( 0.01051738792036946944, 0.9166396752533303438, -0.3995761383050819293 ) ) ;
#24722 = CARTESIAN_POINT ( 'NONE',  ( -197.4153392276050170, -14.14666332908280211, 49.11379398046769040 ) ) ;
#24723 = CARTESIAN_POINT ( 'NONE',  ( 130.8568914410475088, -39.99999999999992895, -5.949712681207114606 ) ) ;
#24724 = CARTESIAN_POINT ( 'NONE',  ( -91.56559293963834989, -16.03295912088728414, 16.03295912088688269 ) ) ;
#24725 = CARTESIAN_POINT ( 'NONE',  ( -90.07798792367796636, -22.27377874500496802, 0.000000000000000000 ) ) ;
#24726 = AXIS2_PLACEMENT_3D ( 'NONE', #7698, #7964, #22222 ) ;
#24728 = CARTESIAN_POINT ( 'NONE',  ( 170.2234770963711128, 39.20704971665372796, 17.36149277827039583 ) ) ;
#24727 = CARTESIAN_POINT ( 'NONE',  ( -188.2871287166139496, 23.44689273421231945, -43.00155302796424905 ) ) ;
#24729 = CARTESIAN_POINT ( 'NONE',  ( 136.1360204305621551, 3.511608612530062512, 53.05693388239318864 ) ) ;
#24730 = CARTESIAN_POINT ( 'NONE',  ( 14.38125909742182884, -55.17850393974264733, -40.00000000000002132 ) ) ;
#24731 = CARTESIAN_POINT ( 'NONE',  ( -208.1127848780265026, 55.00245453012668406, 2.449293598294708485E-15 ) ) ;
#24732 = CARTESIAN_POINT ( 'NONE',  ( 192.4448373802101173, -39.99999999999977973, -19.99999999996102673 ) ) ;
#24733 = CARTESIAN_POINT ( 'NONE',  ( 200.0000000000000000, -14.14213562373106114, 42.42640687119278908 ) ) ;
#24734 = DIRECTION ( 'NONE',  ( 0.000000000000000000, 1.000000000000000000, 0.000000000000000000 ) ) ;
#24735 = CARTESIAN_POINT ( 'NONE',  ( 14.38125909742182529, -39.01709431150879936, -39.01709431150948859 ) ) ;
#24736 = CARTESIAN_POINT ( 'NONE',  ( 199.9999999999999432, 14.14213562373113398, -14.14213562373094923 ) ) ;
#24737 = ORIENTED_EDGE ( 'NONE', *, *, #15341, .T. ) ;
#24738 = CARTESIAN_POINT ( 'NONE',  ( -213.1075012329537230, -18.58567234101155208, 37.98287015391234434 ) ) ;
#24739 = DIRECTION ( 'NONE',  ( 0.000000000000000000, 1.000000000000000000, 0.000000000000000000 ) ) ;
#24740 = ITEM_DEFINED_TRANSFORMATION ( 'NONE', 'NONE', #11256,  #21058 ) ;
#24741 = CARTESIAN_POINT ( 'NONE',  ( 170.2234770963711128, 17.36149277826973503, 39.20704971665401217 ) ) ;
#24742 = CARTESIAN_POINT ( 'NONE',  ( 17.49521241101099633, -44.30201726250688665, -18.35049639065449867 ) ) ;
#24743 = VERTEX_POINT ( 'NONE', #4417 ) ;
#24744 = CARTESIAN_POINT ( 'NONE',  ( -99.29480781227000818, -20.80016781325181441, 8.165122821357652327 ) ) ;
#24745 = EDGE_CURVE ( 'NONE', #25083, #2152, #16125, .T. ) ;
#24746 = ORIENTED_EDGE ( 'NONE', *, *, #26072, .T. ) ;
#24747 = CARTESIAN_POINT ( 'NONE',  ( 200.0000000000005116, 16.46820326627658204, -9.481692438271846157 ) ) ;
#24748 = AXIS2_PLACEMENT_3D ( 'NONE', #4725, #25080, #6831 ) ;
#24749 = CARTESIAN_POINT ( 'NONE',  ( -1.828631717510329713, 13.94691770814087661, -47.79123445024869454 ) ) ;
#24750 = CARTESIAN_POINT ( 'NONE',  ( -190.5535808405085163, -43.70553721440995076, -18.10342626500903052 ) ) ;
#24751 = CARTESIAN_POINT ( 'NONE',  ( -105.3755690713226727, -8.549198663894545631E-14, 18.24025645688352881 ) ) ;
#24752 = CARTESIAN_POINT ( 'NONE',  ( 151.7948205124836250, 6.767089262349059275, 2.449293598294708485E-15 ) ) ;
#24753 = CARTESIAN_POINT ( 'NONE',  ( 192.4448373802100889, -14.14213562375896061, 14.14213562375865330 ) ) ;
#24754 = CARTESIAN_POINT ( 'NONE',  ( 199.0261637166634330, -10.98746419350304748, 16.71832627740758070 ) ) ;
#24755 = EDGE_CURVE ( 'NONE', #6305, #1888, #18502, .T. ) ;
#24756 = CARTESIAN_POINT ( 'NONE',  ( 19.06497207195981858, -1.881589693694111225E-13, 54.19242893257843008 ) ) ;
#24757 = CARTESIAN_POINT ( 'NONE',  ( -259.2033419157646676, 40.00000000000000711, -9.517827891722491884 ) ) ;
#24758 = CARTESIAN_POINT ( 'NONE',  ( -90.07798792367799479, 15.74993999324186156, -15.74993999324171234 ) ) ;
#24759 = CARTESIAN_POINT ( 'NONE',  ( -192.9588430854690273, -14.46834944099973264, -40.00000000000002132 ) ) ;
#24760 = CARTESIAN_POINT ( 'NONE',  ( -280.0000000000000000, -20.00000000000006750, -2.449293598294708485E-15 ) ) ;
#24761 = CARTESIAN_POINT ( 'NONE',  ( 57.59792236341148453, 1.722363176414758668, 54.84617931850880268 ) ) ;
#24762 = CARTESIAN_POINT ( 'NONE',  ( 118.9130007099546305, -10.68958087202327789, -25.80693111732292166 ) ) ;
#24763 = CARTESIAN_POINT ( 'NONE',  ( -110.0904723790853410, 16.34339323355447959, -11.87257855583790800 ) ) ;
#24764 = CARTESIAN_POINT ( 'NONE',  ( 146.6084372240433709, 39.99999999999968026, 34.62501878078347772 ) ) ;
#24765 = CARTESIAN_POINT ( 'NONE',  ( 14.38125909742182529, -40.00000000000021316, 55.17850393974251944 ) ) ;
#24766 = CARTESIAN_POINT ( 'NONE',  ( 199.0260481038674811, -10.14773143618404383, 17.24088832081764622 ) ) ;
#24767 = CARTESIAN_POINT ( 'NONE',  ( -175.9235640283763757, -42.70623598288129585, -12.95568063866271480 ) ) ;
#24768 = CARTESIAN_POINT ( 'NONE',  ( -114.5523123854248695, -19.58652998792717881, 9.959192389756644559 ) ) ;
#24769 = CARTESIAN_POINT ( 'NONE',  ( 4.995406935893297984, -39.06748935135182421, -17.50105314357212549 ) ) ;
#24770 = ORIENTED_EDGE ( 'NONE', *, *, #18586, .F. ) ;
#24771 = DIRECTION ( 'NONE',  ( -1.000000000000000000, 0.000000000000000000, 0.000000000000000000 ) ) ;
#24772 = CARTESIAN_POINT ( 'NONE',  ( 127.8236149080042878, 28.75948073575762720, -11.91256696755847067 ) ) ;
#24773 = CARTESIAN_POINT ( 'NONE',  ( -135.8532207217289454, -30.84685318188648750, -40.00000000000002132 ) ) ;
#24774 = SHAPE_REPRESENTATION ( 'Pump housing', ( #21058 ), #9559 ) ;
#24775 = CARTESIAN_POINT ( 'NONE',  ( 169.9999999999674571, -17.64300463372919836, -17.64300463252165585 ) ) ;
#24776 = CARTESIAN_POINT ( 'NONE',  ( -198.0356074513804572, 10.87444709759730088, -10.87444709759707173 ) ) ;
#24777 =( NAMED_UNIT ( * ) PLANE_ANGLE_UNIT ( ) SI_UNIT ( $, .RADIAN. ) );
#24778 = ORIENTED_EDGE ( 'NONE', *, *, #19245, .T. ) ;
#24779 = VERTEX_POINT ( 'NONE', #4554 ) ;
#24780 = CARTESIAN_POINT ( 'NONE',  ( -200.0000000000000000, 71.50000000000011369, -66.50000000000005684 ) ) ;
#24781 = CARTESIAN_POINT ( 'NONE',  ( -93.01741312759801872, 8.946232117438750464, -20.50009083235881135 ) ) ;
#24782 = CARTESIAN_POINT ( 'NONE',  ( 22.75856136761766635, 17.88529938203902958, 43.17893233522205065 ) ) ;
#24783 = VERTEX_POINT ( 'NONE', #21038 ) ;
#24784 = EDGE_CURVE ( 'NONE', #5675, #12661, #4684, .T. ) ;
#24785 = EDGE_LOOP ( 'NONE', ( #11218, #22356, #11548, #2064, #15508 ) ) ;
#24786 = CARTESIAN_POINT ( 'NONE',  ( -105.3755690713226585, -15.38646221621796251, 41.18208027870593924 ) ) ;
#24787 = CARTESIAN_POINT ( 'NONE',  ( 199.0248198352711313, -19.48551319141294869, 4.538181572781159190 ) ) ;
#24788 = CARTESIAN_POINT ( 'NONE',  ( -105.2054292635175869, -15.19799821370180126, -15.19799821370278892 ) ) ;
#24789 = CARTESIAN_POINT ( 'NONE',  ( -105.4894168351564048, 19.67999904371083275, 8.151722511394638104 ) ) ;
#24790 = CARTESIAN_POINT ( 'NONE',  ( -199.9999999999999147, -16.85576820966601019, 47.13392792189009839 ) ) ;
#24791 = EDGE_CURVE ( 'NONE', #23081, #3931, #119, .T. ) ;
#24792 = ADVANCED_FACE ( 'NONE', ( #11055 ), #19167, .T. ) ;
#24793 = LINE ( 'NONE', #14654, #11888 ) ;
#24794 = CARTESIAN_POINT ( 'NONE',  ( 14.38125909742180930, 40.00000000000060396, -55.17850393974224232 ) ) ;
#24795 = CARTESIAN_POINT ( 'NONE',  ( 151.7948205124836534, 39.99999999999970157, 33.23291073765595627 ) ) ;
#24796 = CARTESIAN_POINT ( 'NONE',  ( 180.0000000000000000, -66.50000000000001421, -66.50000000000005684 ) ) ;
#24797 = DIRECTION ( 'NONE',  ( 0.000000000000000000, 1.000000000000000000, 0.000000000000000000 ) ) ;
#24798 = CARTESIAN_POINT ( 'NONE',  ( 199.0062801269303350, 18.72091001596172433, -7.031396878026334285 ) ) ;
#24799 = CARTESIAN_POINT ( 'NONE',  ( -189.5227390968106818, 18.00253259953367291, 43.46195835885502845 ) ) ;
#24800 = CARTESIAN_POINT ( 'NONE',  ( -135.8532207217289738, -21.81201906317806305, 34.75652343174590442 ) ) ;
#24801 = DIRECTION ( 'NONE',  ( 1.000000000000000000, 1.836970198721025990E-16, 0.000000000000000000 ) ) ;
#24802 = CARTESIAN_POINT ( 'NONE',  ( 4.995406935893301537, -10.78321810390187530, 67.35176059882529387 ) ) ;
#24803 = FACE_OUTER_BOUND ( 'NONE', #22513, .T. ) ;
#24804 = CARTESIAN_POINT ( 'NONE',  ( -135.8532207217289738, 34.75652343174625258, -21.81201906317744132 ) ) ;
#24805 = CARTESIAN_POINT ( 'NONE',  ( -648.3028445202884313, 35.38721658766822031, 27.84362906246311553 ) ) ;
#24806 = CARTESIAN_POINT ( 'NONE',  ( -105.3755690713226869, 21.75974354311648540, -0.000000000000000000 ) ) ;
#24807 = CARTESIAN_POINT ( 'NONE',  ( 91.82158438592158234, -12.16597498397778843, 12.16597498397750954 ) ) ;
#24808 = CARTESIAN_POINT ( 'NONE',  ( 136.1360204305621266, 35.03383547441298163, 40.00000000000002132 ) ) ;
#24809 = CARTESIAN_POINT ( 'NONE',  ( -624.5354243231303144, 28.28427124746188781, -34.99999999999999289 ) ) ;
#24810 = CARTESIAN_POINT ( 'NONE',  ( 57.59792236341147742, 4.064940816252731242E-13, -37.56421063658186199 ) ) ;
#24811 = CARTESIAN_POINT ( 'NONE',  ( 199.0079621347063892, 1.362236960746584069, -19.95249283290727860 ) ) ;
#24812 = CARTESIAN_POINT ( 'NONE',  ( 144.9504669809063273, -12.48392651407863596, 30.13886470195687295 ) ) ;
#24813 = ORIENTED_EDGE ( 'NONE', *, *, #2404, .T. ) ;
#24814 = ORIENTED_EDGE ( 'NONE', *, *, #15794, .T. ) ;
#24815 = CARTESIAN_POINT ( 'NONE',  ( -91.56559293963834989, 17.32597176626808988, 40.00000000000002132 ) ) ;
#24816 = CARTESIAN_POINT ( 'NONE',  ( -716.9846540392142060, -66.50000000000001421, -66.50000000000005684 ) ) ;
#24817 = CARTESIAN_POINT ( 'NONE',  ( 146.6084372240433709, 32.08495691632030145, 24.48358557860365181 ) ) ;
#24818 = B_SPLINE_CURVE_WITH_KNOTS ( 'NONE', 3,
 ( #23201, #19576, #21706, #15070, #21205, #5479, #19701, #9341, #11208, #19323, #9465, #2977, #17449, #11085, #13579, #25588 ),
 .UNSPECIFIED., .F., .F.,
 ( 4, 2, 2, 2, 2, 2, 2, 4 ),
 ( -5.998499569545109335E-08, 0.003520343011582055190, 0.007040746008159805801, 0.01408155200131531309, 0.01760195499789306978, 0.02112235799447082299, 0.02464276099104858314, 0.02816316398762633982 ),
 .UNSPECIFIED. ) ;
#24819 = CARTESIAN_POINT ( 'NONE',  ( -114.6375327213568340, -21.34761811098216455, 5.510795915293953406 ) ) ;
#24820 = CARTESIAN_POINT ( 'NONE',  ( -163.5815439473242634, 12.03526835478819557, -38.33196286486828797 ) ) ;
#24821 = LINE ( 'NONE', #8711, #18575 ) ;
#24822 = CARTESIAN_POINT ( 'NONE',  ( 199.9999999999998579, -2.482523633563583410, -18.84177167654976515 ) ) ;
#24823 =( REPRESENTATION_RELATIONSHIP ('NONE','NONE', #23888, #14572 ) REPRESENTATION_RELATIONSHIP_WITH_TRANSFORMATION ( #5973 )SHAPE_REPRESENTATION_RELATIONSHIP( ) );
#24824 = CARTESIAN_POINT ( 'NONE',  ( 199.9999999999999147, 5.804186778207960806, -18.09503644758711260 ) ) ;
#24825 = CARTESIAN_POINT ( 'NONE',  ( -56.48582580120559982, -6.472252184283581400, -50.09629031063973059 ) ) ;
#24826 = CARTESIAN_POINT ( 'NONE',  ( -100.7734535825088500, 16.03295912088691821, 16.03295912088721309 ) ) ;
#24827 = CARTESIAN_POINT ( 'NONE',  ( 170.0000000000000000, 3.122849337825751958E-14, 0.000000000000000000 ) ) ;
#24828 = CARTESIAN_POINT ( 'NONE',  ( -100.7734535825088500, 39.99999999999976552, 22.67402823373233645 ) ) ;
#24829 = CARTESIAN_POINT ( 'NONE',  ( 151.7948205124836250, 23.49921654116328540, 23.49921654116366554 ) ) ;
#24830 = CARTESIAN_POINT ( 'NONE',  ( 20.59573805978978456, 13.93986955483944534, 47.74081960064682306 ) ) ;
#24831 = CARTESIAN_POINT ( 'NONE',  ( -208.1127848780265026, 10.60833733269537049, 10.60833733269544510 ) ) ;
#24832 = CARTESIAN_POINT ( 'NONE',  ( -208.1127848780264742, -38.89260858015758515, 38.89260858015713751 ) ) ;
#24833 = CARTESIAN_POINT ( 'NONE',  ( 199.0060273340149024, 18.25277364203476438, -8.166168630484282431 ) ) ;
#24835 = CARTESIAN_POINT ( 'NONE',  ( -30.26275506840323359, -1.535832457777009877E-13, 41.69427246844629309 ) ) ;
#24834 = CARTESIAN_POINT ( 'NONE',  ( -100.7734535825088500, -44.31723036834885932, -12.25131212657538171 ) ) ;
#24836 = CARTESIAN_POINT ( 'NONE',  ( 192.4448373802101173, 14.14213562370261279, 42.42640687122091236 ) ) ;
#24837 = CARTESIAN_POINT ( 'NONE',  ( 22.86726691379442045, 43.14849715852157885, -17.87269271907634760 ) ) ;
#24838 = CARTESIAN_POINT ( 'NONE',  ( 4.995406935893288214, 15.24977328854832770, -40.00000000000002132 ) ) ;
#24839 = CARTESIAN_POINT ( 'NONE',  ( -238.4067589809705794, -27.60227080167069147, 28.96627169325319429 ) ) ;
#24840 = CARTESIAN_POINT ( 'NONE',  ( 0.2972598230769930017, 54.33493731733936016, 40.00000000000002132 ) ) ;
#24841 = CARTESIAN_POINT ( 'NONE',  ( -17.28139728210402382, -42.38047544432864555, 12.88180358343662846 ) ) ;
#24842 = CARTESIAN_POINT ( 'NONE',  ( 163.1118516004056573, -27.26290988616869626, 40.00000000000002132 ) ) ;
#24843 = ORIENTED_EDGE ( 'NONE', *, *, #15245, .F. ) ;
#24844 = CARTESIAN_POINT ( 'NONE',  ( 23.23639021239541691, 23.37084785298121403, -42.89921396172169921 ) ) ;
#24845 = CARTESIAN_POINT ( 'NONE',  ( 151.7948205124836250, -23.49921654116339553, -23.49921654116350211 ) ) ;
#24846 = CARTESIAN_POINT ( 'NONE',  ( -4.151555265633219527, -23.42746911247767017, 42.97219445042060926 ) ) ;
#24847 = ADVANCED_FACE ( 'NONE', ( #10792 ), #14378, .T. ) ;
#24848 = CARTESIAN_POINT ( 'NONE',  ( -3.786831587087909679, 13.84155926340511478, -47.08106124085716004 ) ) ;
#24849 = CARTESIAN_POINT ( 'NONE',  ( 199.9999999999997442, -9.911795474730137556, 16.22255894585034852 ) ) ;
#24850 = CARTESIAN_POINT ( 'NONE',  ( -208.1127848780264742, 38.89260858015707356, 17.67593391476696141 ) ) ;
#24851 = CARTESIAN_POINT ( 'NONE',  ( -77.78745312850900007, -20.88824371468822250, 6.815361097891073250 ) ) ;
#24852 = CARTESIAN_POINT ( 'NONE',  ( 190.0000000000000000, -52.49999999999970868, 82.49999999999998579 ) ) ;
#24853 = CARTESIAN_POINT ( 'NONE',  ( -192.6563370915827420, -18.27409561807003868, 44.11756948122302191 ) ) ;
#24854 = CARTESIAN_POINT ( 'NONE',  ( -238.4067589809705794, -0.6820004457913585449, -0.6820004457913265705 ) ) ;
#24855 = CARTESIAN_POINT ( 'NONE',  ( 136.1360204305621551, -53.05693388239309627, -3.511608612531332163 ) ) ;
#24856 = CARTESIAN_POINT ( 'NONE',  ( -259.2033419157646676, 35.01439189186559275, -21.55415060305807984 ) ) ;
#24858 = CARTESIAN_POINT ( 'NONE',  ( 184.8905102610680444, 13.49065550809826952, -13.49065550809790359 ) ) ;
#24857 = CARTESIAN_POINT ( 'NONE',  ( 130.8568914410475372, 24.07718906447210472, 24.07718906447249907 ) ) ;
#24859 = CARTESIAN_POINT ( 'NONE',  ( 151.7948205124836534, 4.785054706297857230, 51.78348778862544322 ) ) ;
#24860 = CARTESIAN_POINT ( 'NONE',  ( 4.995406935893307754, -55.24977328854835434, -2.449293598294708485E-15 ) ) ;
#24861 = CARTESIAN_POINT ( 'NONE',  ( -259.2033419157646676, 30.48217210827734647, 2.449293598294708485E-15 ) ) ;
#24862 = CARTESIAN_POINT ( 'NONE',  ( 4.995406935893297984, -39.99999999999986500, -15.24977328854874870 ) ) ;
#24863 = CARTESIAN_POINT ( 'NONE',  ( -238.4067589809705794, 0.6820004457912757223, 0.6820004457913219076 ) ) ;
#24864 = FACE_OUTER_BOUND ( 'NONE', #21711, .T. ) ;
#24865 = PRODUCT ( 'Discharge flange', 'Discharge flange', '', ( #17932 ) ) ;
#24866 = CARTESIAN_POINT ( 'NONE',  ( 200.0000000000000000, 14.14213562373142352, -42.42640687119268961 ) ) ;
#24867 = CARTESIAN_POINT ( 'NONE',  ( -100.7734535825088500, 16.03295912088713848, -16.03295912088698927 ) ) ;
#24868 = ORIENTED_EDGE ( 'NONE', *, *, #20621, .T. ) ;
#24869 = CARTESIAN_POINT ( 'NONE',  ( -135.8532207217289738, 21.81201906317767936, 21.81201906317778239 ) ) ;
#24870 = CARTESIAN_POINT ( 'NONE',  ( -716.9846540392142060, -66.50000000000001421, -61.50000000000006395 ) ) ;
#24871 = CONTEXT_DEPENDENT_SHAPE_REPRESENTATION ( #23942, #25890 ) ;
#24872 = CARTESIAN_POINT ( 'NONE',  ( -162.0762913951020892, -29.48230308784785692, 29.48230308784751230 ) ) ;
#24873 = CARTESIAN_POINT ( 'NONE',  ( -4.022465846214346996, -43.01021959554127250, -23.45302613997624874 ) ) ;
#24874 = ORIENTED_EDGE ( 'NONE', *, *, #26231, .F. ) ;
#24875 = CARTESIAN_POINT ( 'NONE',  ( -4.039451493210481026, -46.99046209229796034, -13.82811171175467102 ) ) ;
#24876 = DIRECTION ( 'NONE',  ( -0.01051738777842141370, -0.9166396752737698828, 0.3995761382619288926 ) ) ;
#24877 = VERTEX_POINT ( 'NONE', #4550 ) ;
#24878 = CARTESIAN_POINT ( 'NONE',  ( 200.0000000000001137, 18.27430636540404407, -5.205727087885991367 ) ) ;
#24879 = CARTESIAN_POINT ( 'NONE',  ( -114.6318783467508240, -21.31802243455910784, -5.473070270850431740 ) ) ;
#24880 = CARTESIAN_POINT ( 'NONE',  ( -280.0000000000000000, 19.99999999999996092, 2.449293598294708485E-15 ) ) ;
#24881 = CARTESIAN_POINT ( 'NONE',  ( -162.0762913951020892, 1.198031840385732849, -1.198031840385733515 ) ) ;
#24882 = CARTESIAN_POINT ( 'NONE',  ( 199.0120816426991155, 18.34336195414084969, 7.966874786652939910 ) ) ;
#24883 = AXIS2_PLACEMENT_3D ( 'NONE', #22950, #1127, #8843 ) ;
#24884 = VECTOR ( 'NONE', #19605, 1000.000000000000000 ) ;
#24885 = CARTESIAN_POINT ( 'NONE',  ( -91.56559293963836410, -12.25131212657524138, 44.31723036834888774 ) ) ;
#24886 = CARTESIAN_POINT ( 'NONE',  ( -162.0762913951020892, 39.99999999999985079, 41.69427287692695216 ) ) ;
#24887 = CARTESIAN_POINT ( 'NONE',  ( -208.1127848780264742, 39.99999999999979394, 55.00245453010936103 ) ) ;
#24888 = CARTESIAN_POINT ( 'NONE',  ( -86.86493150571116928, -8.366608963953867217, -19.60045294882765887 ) ) ;
#24889 = CARTESIAN_POINT ( 'NONE',  ( -86.96347745069645896, 21.75974354311648895, -40.00000000000002132 ) ) ;
#24890 = CARTESIAN_POINT ( 'NONE',  ( -597.2601520101716233, 39.79372847804995672, 4.185400860730163153 ) ) ;
#24891 = CARTESIAN_POINT ( 'NONE',  ( 184.8905102610680444, -19.07866798485553872, -40.00000000000002132 ) ) ;
#24892 = CARTESIAN_POINT ( 'NONE',  ( -238.4067589809705794, 27.60227080167040370, 28.96627169325338613 ) ) ;
#24893 = CARTESIAN_POINT ( 'NONE',  ( 121.8740240556053180, -11.10671848392261829, -26.81399039734618839 ) ) ;
#24894 = CARTESIAN_POINT ( 'NONE',  ( -110.0791661673351172, 10.82529631555651761, -17.04053483147850301 ) ) ;
#24895 = CARTESIAN_POINT ( 'NONE',  ( 14.38125909742181818, 5.830552384690105017E-13, -55.17850393972636880 ) ) ;
#24896 = CARTESIAN_POINT ( 'NONE',  ( -86.96347745069645896, 39.99999999999994316, 18.24025645688366737 ) ) ;
#24897 = CARTESIAN_POINT ( 'NONE',  ( 199.0263607205240532, -13.20175300279655062, 15.04466839055514527 ) ) ;
#24898 = CARTESIAN_POINT ( 'NONE',  ( -114.4364955367323091, -20.29001642039124675, -8.064892380834873364 ) ) ;
#24899 = CARTESIAN_POINT ( 'NONE',  ( -114.5450021253288782, -9.945938879692020507, 19.55077795857343403 ) ) ;
#24900 = CARTESIAN_POINT ( 'NONE',  ( 0.2972598230770100991, -38.42060263243686791, 38.42060263243645579 ) ) ;
#24901 = EDGE_LOOP ( 'NONE', ( #9191, #24379, #163, #10234 ) ) ;
#24903 = DIRECTION ( 'NONE',  ( 0.000000000000000000, 0.000000000000000000, 1.000000000000000000 ) ) ;
#24902 = CARTESIAN_POINT ( 'NONE',  ( -30.26275506840324070, -1.198031551616016266, -1.198031551616031587 ) ) ;
#24904 = CARTESIAN_POINT ( 'NONE',  ( 144.9504669809064694, 30.13886470195707545, -12.48392651407830911 ) ) ;
#24905 = CARTESIAN_POINT ( 'NONE',  ( 151.7948205124835681, 33.23291073765556547, -40.00000000000002132 ) ) ;
#24906 = DIRECTION ( 'NONE',  ( 1.000000000000000000, -1.937599346585394162E-16, -0.000000000000000000 ) ) ;
#24907 = CARTESIAN_POINT ( 'NONE',  ( 192.4448373802100889, -14.14213562375896061, 14.14213562375865330 ) ) ;
#24908 =( NAMED_UNIT ( * ) PLANE_ANGLE_UNIT ( ) SI_UNIT ( $, .RADIAN. ) );
#24909 = EDGE_LOOP ( 'NONE', ( #24140, #7429, #4694, #11517 ) ) ;
#24910 =( GEOMETRIC_REPRESENTATION_CONTEXT ( 3 ) GLOBAL_UNCERTAINTY_ASSIGNED_CONTEXT ( ( #24294 ) ) GLOBAL_UNIT_ASSIGNED_CONTEXT ( ( #22264, #20397, #24253 ) ) REPRESENTATION_CONTEXT ( 'NONE', 'WORKASPACE' ) );
#24911 = VERTEX_POINT ( 'NONE', #10520 ) ;
#24912 = VECTOR ( 'NONE', #5185, 1000.000000000000000 ) ;
#24913 = EDGE_CURVE ( 'NONE', #7180, #12655, #8054, .T. ) ;
#24914 = CARTESIAN_POINT ( 'NONE',  ( 199.9999999999999716, 3.394816402666279931, 18.70522384341381894 ) ) ;
#24915 = CARTESIAN_POINT ( 'NONE',  ( -105.4741150117382205, 7.943527260749760899, -19.77569912955142684 ) ) ;
#24916 = CARTESIAN_POINT ( 'NONE',  ( 22.57783252599927337, 17.90541116499370844, 43.22748647440086955 ) ) ;
#24917 = ORIENTED_EDGE ( 'NONE', *, *, #20785, .T. ) ;
#24918 = ORIENTED_EDGE ( 'NONE', *, *, #24438, .T. ) ;
#24919 = CARTESIAN_POINT ( 'NONE',  ( -259.2033419157646676, -6.730120644403667640, 49.83842185052029805 ) ) ;
#24920 = CARTESIAN_POINT ( 'NONE',  ( 199.0178460907175690, -16.45326163792621443, -11.37340206338170923 ) ) ;
#24921 = CARTESIAN_POINT ( 'NONE',  ( -105.2055636155232889, -1.377569041481722545, 21.49233843348530115 ) ) ;
#24922 = CARTESIAN_POINT ( 'NONE',  ( -198.0356074513804572, -17.40982414986482141, 39.15871834505909987 ) ) ;
#24923 = AXIS2_PLACEMENT_3D ( 'NONE', #9521, #7390, #15501 ) ;
#24924 = CARTESIAN_POINT ( 'NONE',  ( -91.56559293963834989, -16.03295912088706388, -16.03295912088710651 ) ) ;
#24925 = CARTESIAN_POINT ( 'NONE',  ( -213.1075012329537230, 39.99999999999979394, 53.71589010950180665 ) ) ;
#24926 = VECTOR ( 'NONE', #16518, 1000.000000000000000 ) ;
#24927 = FACE_BOUND ( 'NONE', #12350, .T. ) ;
#24928 = DIRECTION ( 'NONE',  ( 1.000000000000000000, -0.000000000000000000, -0.000000000000000000 ) ) ;
#24929 = CARTESIAN_POINT ( 'NONE',  ( 4.995406935893291767, 40.00000000000059686, -55.24977328853165659 ) ) ;
#24930 = CARTESIAN_POINT ( 'NONE',  ( -100.7734535825088500, 39.99999999999976552, 22.67402823373233645 ) ) ;
#24931 = CARTESIAN_POINT ( 'NONE',  ( 170.0000000000000853, 9.369682556672316309, -22.62041470344884075 ) ) ;
#24932 = AXIS2_PLACEMENT_3D ( 'NONE', #3722, #1865, #1465 ) ;
#24933 = CYLINDRICAL_SURFACE ( 'NONE', #20891, 20.53474504356812247 ) ;
#24934 = CARTESIAN_POINT ( 'NONE',  ( 199.0125740919301336, 17.92725630381683644, 8.864156431172764528 ) ) ;
#24935 = CARTESIAN_POINT ( 'NONE',  ( -185.5190358316759500, 17.55874045217352020, 42.39054933781988410 ) ) ;
#24936 = CARTESIAN_POINT ( 'NONE',  ( 57.59792236341147031, -26.56190807104712448, 30.00663442387673285 ) ) ;
#24937 = EDGE_CURVE ( 'NONE', #9554, #151, #19480, .T. ) ;
#24938 =( BOUNDED_SURFACE ( )  B_SPLINE_SURFACE ( 3, 3, ( 
 ( #14012, #18402, #2055, #47, #5768, #10162, #16411, #26141, #9761, #1919, #3779, #13877, #8160, #16273, #4053, #10024, #12154, #26283, #24402, #8022, #7885, #6168, #22415, #24539, #4191, #6295, #14413, #22543, #22010, #11883 ),
 ( #20003, #16138, #24269, #1789, #9893, #17996, #6042, #22279, #24804, #10962, #4447, #10555, #22806, #25071, #4583, #22936, #18536, #8419, #16540, #4846, #19069, #6556, #17069, #4323, #10826, #8694, #20539, #16805, #10419, #4716 ),
 ( #850, #14940, #20943, #12680, #24942, #14544, #12952, #12542, #6690, #12413, #23075, #21070, #318, #2854, #25203, #2310, #24670, #8960, #6950, #12821, #18941, #2443, #16673, #2581, #18667, #721, #6426, #15068, #454, #14670 ),
 ( #2721, #8826, #22674, #20810, #20674, #10696, #6822, #8558, #18807, #587, #14804, #16936, #1234, #7460, #9463, #23199, #13329, #11083, #19321, #9086, #3350, #11579, #21704, #25707, #19699, #4979, #17447, #5477, #13086, #15324 ),
 ( #19446, #1105, #1365, #5350, #1487, #13457, #15573, #17698, #11450, #23697, #21203, #981, #17192, #9593, #13577, #3102, #21451, #19199, #25458, #25842, #17570, #7209, #21331, #3482, #7332, #9339, #21576, #11206, #7586, #23329 ),
 ( #2975, #25330, #17324, #7087, #15201, #19574, #25586, #5104, #15445, #13209, #23573, #3226, #11330, #9213, #23451, #5225, #7847, #1885, #25976, #16241, #23957, #9990, #23822, #13, #24370, #14241, #10259, #24234, #9859, #21836 ),
 ( #5605, #22381, #7984, #22243, #9727, #15698, #13837, #13711, #22108, #5732, #1620, #6133, #21971, #15968, #18100, #3605, #8124, #4157, #12252, #18369, #6007, #17961, #11715, #19834, #17829, #26249, #20374, #16102, #3884, #26108 ) ),
 .UNSPECIFIED., .T., .F., .F. ) 
 B_SPLINE_SURFACE_WITH_KNOTS ( ( 4, 3, 4 ),
 ( 4, 2, 2, 2, 2, 2, 2, 2, 2, 2, 2, 2, 2, 2, 4 ),
 ( 0.000000000000000000, 0.5000000000000000000, 1.000000000000000000 ),
 ( 0.000000000000000000, 0.1357259735107005372, 0.1651108541090157700, 0.1944957347073310028, 0.3598804999793158710, 0.3867117631979620773, 0.4135430264166082281, 0.5789277916885930964, 0.6062785021374117456, 0.6336292125862302838, 0.8508620842112317728, 0.8814014469398914198, 0.9119408096685510667, 0.9559704048342755334, 1.000000000000000000 ),
 .UNSPECIFIED. ) 
 GEOMETRIC_REPRESENTATION_ITEM ( )  RATIONAL_B_SPLINE_SURFACE ( (
 ( 1.000000000000000000, 1.000000000000000000, 1.000000000000000000, 1.000000000000000000, 1.000000000000000000, 1.000000000000000000, 1.000000000000000000, 1.000000000000000000, 1.000000000000000000, 1.000000000000000000, 1.000000000000000000, 1.000000000000000000, 1.000000000000000000, 1.000000000000000000, 1.000000000000000000, 1.000000000000000000, 1.000000000000000000, 1.000000000000000000, 1.000000000000000000, 1.000000000000000000, 1.000000000000000000, 1.000000000000000000, 1.000000000000000000, 1.000000000000000000, 1.000000000000000000, 1.000000000000000000, 1.000000000000000000, 1.000000000000000000, 1.000000000000000000, 1.000000000000000000),
 ( 0.3333333333333333703, 0.3333333333333333703, 0.3333333333333333703, 0.3333333333333333703, 0.3333333333333333703, 0.3333333333333333703, 0.3333333333333333703, 0.3333333333333333703, 0.3333333333333333703, 0.3333333333333333703, 0.3333333333333333703, 0.3333333333333333703, 0.3333333333333333703, 0.3333333333333333703, 0.3333333333333333703, 0.3333333333333333703, 0.3333333333333333703, 0.3333333333333333703, 0.3333333333333333703, 0.3333333333333333703, 0.3333333333333333703, 0.3333333333333333703, 0.3333333333333333703, 0.3333333333333333703, 0.3333333333333333703, 0.3333333333333333703, 0.3333333333333333703, 0.3333333333333333703, 0.3333333333333333703, 0.3333333333333333703),
 ( 0.3333333333333333703, 0.3333333333333333703, 0.3333333333333333703, 0.3333333333333333703, 0.3333333333333333703, 0.3333333333333333703, 0.3333333333333333703, 0.3333333333333333703, 0.3333333333333333703, 0.3333333333333333703, 0.3333333333333333703, 0.3333333333333333703, 0.3333333333333333703, 0.3333333333333333703, 0.3333333333333333703, 0.3333333333333333703, 0.3333333333333333703, 0.3333333333333333703, 0.3333333333333333703, 0.3333333333333333703, 0.3333333333333333703, 0.3333333333333333703, 0.3333333333333333703, 0.3333333333333333703, 0.3333333333333333703, 0.3333333333333333703, 0.3333333333333333703, 0.3333333333333333703, 0.3333333333333333703, 0.3333333333333333703),
 ( 1.000000000000000000, 1.000000000000000000, 1.000000000000000000, 1.000000000000000000, 1.000000000000000000, 1.000000000000000000, 1.000000000000000000, 1.000000000000000000, 1.000000000000000000, 1.000000000000000000, 1.000000000000000000, 1.000000000000000000, 1.000000000000000000, 1.000000000000000000, 1.000000000000000000, 1.000000000000000000, 1.000000000000000000, 1.000000000000000000, 1.000000000000000000, 1.000000000000000000, 1.000000000000000000, 1.000000000000000000, 1.000000000000000000, 1.000000000000000000, 1.000000000000000000, 1.000000000000000000, 1.000000000000000000, 1.000000000000000000, 1.000000000000000000, 1.000000000000000000),
 ( 0.3333333333333333703, 0.3333333333333333703, 0.3333333333333333703, 0.3333333333333333703, 0.3333333333333333703, 0.3333333333333333703, 0.3333333333333333703, 0.3333333333333333703, 0.3333333333333333703, 0.3333333333333333703, 0.3333333333333333703, 0.3333333333333333703, 0.3333333333333333703, 0.3333333333333333703, 0.3333333333333333703, 0.3333333333333333703, 0.3333333333333333703, 0.3333333333333333703, 0.3333333333333333703, 0.3333333333333333703, 0.3333333333333333703, 0.3333333333333333703, 0.3333333333333333703, 0.3333333333333333703, 0.3333333333333333703, 0.3333333333333333703, 0.3333333333333333703, 0.3333333333333333703, 0.3333333333333333703, 0.3333333333333333703),
 ( 0.3333333333333333703, 0.3333333333333333703, 0.3333333333333333703, 0.3333333333333333703, 0.3333333333333333703, 0.3333333333333333703, 0.3333333333333333703, 0.3333333333333333703, 0.3333333333333333703, 0.3333333333333333703, 0.3333333333333333703, 0.3333333333333333703, 0.3333333333333333703, 0.3333333333333333703, 0.3333333333333333703, 0.3333333333333333703, 0.3333333333333333703, 0.3333333333333333703, 0.3333333333333333703, 0.3333333333333333703, 0.3333333333333333703, 0.3333333333333333703, 0.3333333333333333703, 0.3333333333333333703, 0.3333333333333333703, 0.3333333333333333703, 0.3333333333333333703, 0.3333333333333333703, 0.3333333333333333703, 0.3333333333333333703),
 ( 1.000000000000000000, 1.000000000000000000, 1.000000000000000000, 1.000000000000000000, 1.000000000000000000, 1.000000000000000000, 1.000000000000000000, 1.000000000000000000, 1.000000000000000000, 1.000000000000000000, 1.000000000000000000, 1.000000000000000000, 1.000000000000000000, 1.000000000000000000, 1.000000000000000000, 1.000000000000000000, 1.000000000000000000, 1.000000000000000000, 1.000000000000000000, 1.000000000000000000, 1.000000000000000000, 1.000000000000000000, 1.000000000000000000, 1.000000000000000000, 1.000000000000000000, 1.000000000000000000, 1.000000000000000000, 1.000000000000000000, 1.000000000000000000, 1.000000000000000000) ) ) 
 REPRESENTATION_ITEM ( '' )  SURFACE ( )  );
#24939 = FACE_OUTER_BOUND ( 'NONE', #187, .T. ) ;
#24940 = CARTESIAN_POINT ( 'NONE',  ( 91.82158438592159655, 12.16597498400028776, 44.40256751092339016 ) ) ;
#24941 = CARTESIAN_POINT ( 'NONE',  ( -210.0000000000000284, -69.99999999999998579, 8.572527594031471415E-15 ) ) ;
#24942 = CARTESIAN_POINT ( 'NONE',  ( -208.1127848780264742, -10.60833733270725787, -67.17687982763172272 ) ) ;
#24943 = DIRECTION ( 'NONE',  ( -1.000000000000000000, 0.000000000000000000, -0.000000000000000000 ) ) ;
#24944 = CARTESIAN_POINT ( 'NONE',  ( 151.7948205124836250, 33.23291073765556547, 0.000000000000000000 ) ) ;
#24945 = AXIS2_PLACEMENT_3D ( 'NONE', #16720, #4632, #14855 ) ;
#24946 = CARTESIAN_POINT ( 'NONE',  ( -30.26275506840325136, 29.48230279907760121, 27.08623969584625613 ) ) ;
#24947 = CARTESIAN_POINT ( 'NONE',  ( -208.1127848780264742, -15.00245453012673202, 40.00000000000002132 ) ) ;
#24948 = CARTESIAN_POINT ( 'NONE',  ( -599.4962176833719241, 39.44053679066730922, -21.67249732420721031 ) ) ;
#24949 = ORIENTED_EDGE ( 'NONE', *, *, #10297, .T. ) ;
#24950 = CARTESIAN_POINT ( 'NONE',  ( -213.1075012329537230, -39.99999999999991473, -13.71589010951953647 ) ) ;
#24951 = ADVANCED_FACE ( 'NONE', ( #14632 ), #16765, .F. ) ;
#24952 = CARTESIAN_POINT ( 'NONE',  ( 199.0056803851548750, 10.03079491058490724, -17.30956630377439254 ) ) ;
#24953 = EDGE_CURVE ( 'NONE', #6082, #12932, #16902, .T. ) ;
#24954 = CARTESIAN_POINT ( 'NONE',  ( 200.0000000000000000, 63.70262460423112572, -57.69613583541415380 ) ) ;
#24955 = ORIENTED_EDGE ( 'NONE', *, *, #2313, .T. ) ;
#24956 = ORIENTED_EDGE ( 'NONE', *, *, #18731, .F. ) ;
#24957 = CARTESIAN_POINT ( 'NONE',  ( 151.7948205124836534, 6.767089262349056611, 40.00000000000002132 ) ) ;
#24958 = LINE ( 'NONE', #4862, #25328 ) ;
#24959 = CARTESIAN_POINT ( 'NONE',  ( -110.0960685945383091, -20.07406508573906834, -2.528047301430426330 ) ) ;
#24960 = AXIS2_PLACEMENT_3D ( 'NONE', #19035, #22898, #8789 ) ;
#24961 = CARTESIAN_POINT ( 'NONE',  ( -163.5815439473248603, -12.03526835478804635, 38.33196286486853666 ) ) ;
#24962 = CARTESIAN_POINT ( 'NONE',  ( -135.8532207217289738, 7.002209520526292428E-15, -9.153146818113572891 ) ) ;
#24963 = CARTESIAN_POINT ( 'NONE',  ( 200.0000000000000284, 15.35911892145054303, -11.18589804280325772 ) ) ;
#24964 = CARTESIAN_POINT ( 'NONE',  ( -105.2276019244895053, 2.726957955475640016, -21.34775676748449769 ) ) ;
#24965 = CARTESIAN_POINT ( 'NONE',  ( -192.9588430854690273, -18.05360324515400094, -38.51493924976961836 ) ) ;
#24966 = CARTESIAN_POINT ( 'NONE',  ( -259.2033419157646676, 6.730120644403426944, 6.730120644403592145 ) ) ;
#24967 = CARTESIAN_POINT ( 'NONE',  ( -110.1017833366170748, -14.28014421838191694, -14.28014421838201287 ) ) ;
#24968 = CARTESIAN_POINT ( 'NONE',  ( 130.8568914410475088, 39.99999999999969447, 34.05028731879830417 ) ) ;
#24969 = CARTESIAN_POINT ( 'NONE',  ( 151.7948205124835681, -4.785054706298876859, 51.78348778862533663 ) ) ;
#24970 = CARTESIAN_POINT ( 'NONE',  ( -4.039451493210489019, 13.82811171175440812, 46.99046209229809534 ) ) ;
#24971 = CARTESIAN_POINT ( 'NONE',  ( -259.2033419157646676, -6.730120644403570829, -6.730120644403545960 ) ) ;
#24972 = CARTESIAN_POINT ( 'NONE',  ( 130.8568914410475372, -4.207082182992846420, 4.207082182992822439 ) ) ;
#24973 = CARTESIAN_POINT ( 'NONE',  ( 199.0084097827293590, 19.99587590986774188, -0.1328658178166673143 ) ) ;
#24975 = CARTESIAN_POINT ( 'NONE',  ( -91.56559293963834989, 6.234561990864368500E-14, -22.67402823373191723 ) ) ;
#24974 = CARTESIAN_POINT ( 'NONE',  ( -135.8532207217289738, -6.472252184284280396, 6.472252184284099208 ) ) ;
#24976 = CARTESIAN_POINT ( 'NONE',  ( 37.15749683989781005, 38.58455518501556014, -20.52531616266200132 ) ) ;
#24977 = CARTESIAN_POINT ( 'NONE',  ( -162.0762913951020892, 1.694272876828294194, 0.000000000000000000 ) ) ;
#24978 = CARTESIAN_POINT ( 'NONE',  ( 200.0000000000000000, -42.42640687119293119, 14.14213562373082134 ) ) ;
#24979 = CARTESIAN_POINT ( 'NONE',  ( 130.8568914410475088, -34.05028731879786363, 40.00000000000002132 ) ) ;
#24980 = VERTEX_POINT ( 'NONE', #14899 ) ;
#24981 = CARTESIAN_POINT ( 'NONE',  ( 3.774039766349060354, -44.61221010186880420, 18.47898247163330154 ) ) ;
#24982 = CARTESIAN_POINT ( 'NONE',  ( 151.7948205124836534, 6.767089262349056611, 40.00000000000002132 ) ) ;
#24983 = ORIENTED_EDGE ( 'NONE', *, *, #43, .F. ) ;
#24984 = CARTESIAN_POINT ( 'NONE',  ( 0.4311942631275938465, 24.25071831022430402, -44.08816696360397458 ) ) ;
#24985 = CARTESIAN_POINT ( 'NONE',  ( -259.2033419157646676, -6.730120644403570829, -6.730120644403545960 ) ) ;
#24986 = CARTESIAN_POINT ( 'NONE',  ( -4.121597284766226998, -13.82232031191914245, 46.96202426942505070 ) ) ;
#24987 = CARTESIAN_POINT ( 'NONE',  ( 6.371015797563456928, 18.55864253217522020, -44.80452650039788409 ) ) ;
#24988 = CARTESIAN_POINT ( 'NONE',  ( 199.0263356842403653, -15.36141226383640301, 12.81629321302553848 ) ) ;
#24989 = CARTESIAN_POINT ( 'NONE',  ( 19.06497207195979726, 38.31983398719604139, 18.24870850772803976 ) ) ;
#24990 = CARTESIAN_POINT ( 'NONE',  ( -87.10437264497180365, -21.30276644672514053, 2.718829733159835005 ) ) ;
#24991 = CARTESIAN_POINT ( 'NONE',  ( -109.1264249741455785, -13.72187187124632501, -33.12752917268957731 ) ) ;
#24992 = CARTESIAN_POINT ( 'NONE',  ( -188.8753834511958019, -17.93496043754513991, 43.29882472894604462 ) ) ;
#24993 = CARTESIAN_POINT ( 'NONE',  ( -208.1127848780265026, -10.60833733269537227, -10.60833733269551793 ) ) ;
#24994 = CARTESIAN_POINT ( 'NONE',  ( 146.6084372240433709, 24.48358557860311180, 32.08495691632071356 ) ) ;
#24995 = CARTESIAN_POINT ( 'NONE',  ( -86.96347745069644475, -15.38646221621807442, 15.38646221621768184 ) ) ;
#24996 = CARTESIAN_POINT ( 'NONE',  ( -280.0000000000000568, 42.42640687119294540, -14.14213562373059041 ) ) ;
#24998 = CARTESIAN_POINT ( 'NONE',  ( -280.0000000000000000, 14.14213562373108246, -14.14213562373078581 ) ) ;
#24997 = CARTESIAN_POINT ( 'NONE',  ( -30.26275506840324070, -1.198031551616016266, -1.198031551616031587 ) ) ;
#24999 = CARTESIAN_POINT ( 'NONE',  ( -91.56559293963834989, -16.03295912088728414, 16.03295912088688269 ) ) ;
#25000 = CARTESIAN_POINT ( 'NONE',  ( 170.2234770963711128, -15.44714144992813409, 40.00000000000002132 ) ) ;
#25001 = CARTESIAN_POINT ( 'NONE',  ( -198.0356074513804572, 15.37879056873066830, -40.00000000000002132 ) ) ;
#25002 = CARTESIAN_POINT ( 'NONE',  ( 136.1360204305621551, 3.511608612530801032, -53.05693388239316022 ) ) ;
#25003 = CARTESIAN_POINT ( 'NONE',  ( -103.9663809734080786, 19.92521373365561033, -8.574562932722885833 ) ) ;
#25004 = CARTESIAN_POINT ( 'NONE',  ( -259.2033419157646676, 6.730120644403918995, -49.83842185052024831 ) ) ;
#25005 = DIRECTION ( 'NONE',  ( 0.000000000000000000, -1.000000000000000000, 0.000000000000000000 ) ) ;
#25006 = ORIENTED_EDGE ( 'NONE', *, *, #8079, .T. ) ;
#25007 = CARTESIAN_POINT ( 'NONE',  ( -162.0762913951021176, 1.198031840315997298, 57.76657433523996588 ) ) ;
#25008 = CARTESIAN_POINT ( 'NONE',  ( -82.30220482034329166, -18.51665893431366072, -7.992411108784819085 ) ) ;
#25009 = CARTESIAN_POINT ( 'NONE',  ( 170.2234770963711128, -10.92277846919202666, 10.92277846919193962 ) ) ;
#25010 = CARTESIAN_POINT ( 'NONE',  ( -3.434479974377945499, -43.30650750418227091, -17.93814274724467239 ) ) ;
#25011 = ORIENTED_EDGE ( 'NONE', *, *, #6156, .T. ) ;
#25012 = CARTESIAN_POINT ( 'NONE',  ( -105.4741150117398263, -19.77569912953930498, 7.943527260776862775 ) ) ;
#25013 = CARTESIAN_POINT ( 'NONE',  ( -114.5516609237780585, -9.951797154676993884, -19.58913668464228053 ) ) ;
#25014 = CARTESIAN_POINT ( 'NONE',  ( 200.0000000000000000, 17.99825158093497635, -6.097534595090909448 ) ) ;
#25015 = CARTESIAN_POINT ( 'NONE',  ( 200.0000000000000000, 75.52305771588345351, -68.47933392563552957 ) ) ;
#25016 = CARTESIAN_POINT ( 'NONE',  ( -259.2033419157646676, 30.48217210827734647, 2.449293598294708485E-15 ) ) ;
#25017 = CARTESIAN_POINT ( 'NONE',  ( -198.0356074513804572, -17.40982414986427429, -39.15871834505933435 ) ) ;
#25018 = CARTESIAN_POINT ( 'NONE',  ( 199.0135736376541615, 16.97384353125803003, 10.58053792802146020 ) ) ;
#25019 = EDGE_CURVE ( 'NONE', #2784, #19812, #17271, .T. ) ;
#25020 = CARTESIAN_POINT ( 'NONE',  ( -192.9588430854690273, -38.51493924976957572, 18.05360324515410397 ) ) ;
#25021 = CARTESIAN_POINT ( 'NONE',  ( -30.26275506840323359, -1.535832457777009877E-13, 41.69427246844629309 ) ) ;
#25022 = CARTESIAN_POINT ( 'NONE',  ( -91.56559293963836410, 40.00000000000008527, -22.67402823373177867 ) ) ;
#25023 = CARTESIAN_POINT ( 'NONE',  ( -188.2995950289364089, -23.44932284465861727, -43.00522595870986464 ) ) ;
#25024 = CARTESIAN_POINT ( 'NONE',  ( -198.0356074513804288, -55.37879056873077133, -2.449293598294708485E-15 ) ) ;
#25026 = CARTESIAN_POINT ( 'NONE',  ( -135.8532207217289738, 6.472252184284186249, -6.472252184284142729 ) ) ;
#25025 = CARTESIAN_POINT ( 'NONE',  ( 22.90311673803731196, -13.82691048573729908, -46.98314248934561732 ) ) ;
#25027 = CARTESIAN_POINT ( 'NONE',  ( 163.1118516004056573, -12.73709011382472234, -2.449293598294708485E-15 ) ) ;
#25028 = CARTESIAN_POINT ( 'NONE',  ( 130.8568914410475372, -4.207082182992846420, 4.207082182992822439 ) ) ;
#25029 = CARTESIAN_POINT ( 'NONE',  ( -135.8532207217289738, -1.208299557080134822E-13, 9.153146818113572891 ) ) ;
#25030 = CARTESIAN_POINT ( 'NONE',  ( -105.3239292022353055, 10.85048923520651520, -18.46172643728406726 ) ) ;
#25031 = CARTESIAN_POINT ( 'NONE',  ( 184.8905102610680444, 40.00000000000025580, -19.07866798485515503 ) ) ;
#25032 = CARTESIAN_POINT ( 'NONE',  ( 146.6084372240433993, -24.48358557860319706, -24.48358557860330720 ) ) ;
#25033 = FACE_BOUND ( 'NONE', #23663, .T. ) ;
#25034 = CARTESIAN_POINT ( 'NONE',  ( -88.39148973765161088, -8.577159256668537068, -19.92926839984431098 ) ) ;
#25035 = CARTESIAN_POINT ( 'NONE',  ( -213.1075012329536946, -37.98287015391263566, 37.98287015391218802 ) ) ;
#25036 = ORIENTED_EDGE ( 'NONE', *, *, #20398, .T. ) ;
#25038 = CARTESIAN_POINT ( 'NONE',  ( -188.5332406156470313, 23.50029615585822640, -43.07394490459756042 ) ) ;
#25037 = CARTESIAN_POINT ( 'NONE',  ( 151.7948205124836250, 23.49921654116328540, 23.49921654116366554 ) ) ;
#25039 = CYLINDRICAL_SURFACE ( 'NONE', #17394, 5.000000000000004441 ) ;
#25040 = CARTESIAN_POINT ( 'NONE',  ( -105.3755690713226727, -18.24025645688354302, -2.449293598294708485E-15 ) ) ;
#25041 = VECTOR ( 'NONE', #7705, 999.9999999999998863 ) ;
#25042 = ADVANCED_FACE ( 'NONE', ( #8657 ), #6654, .T. ) ;
#25043 = CARTESIAN_POINT ( 'NONE',  ( -114.6318783467488203, 11.20407312249095533, -18.94416332741571196 ) ) ;
#25044 = CARTESIAN_POINT ( 'NONE',  ( -190.0000000000000000, -66.50000000000001421, 66.50000000000005684 ) ) ;
#25045 = ORIENTED_EDGE ( 'NONE', *, *, #19861, .F. ) ;
#25046 =( BOUNDED_SURFACE ( )  B_SPLINE_SURFACE ( 3, 2, ( 
 ( #15391, #25008, #13395 ),
 ( #17387, #19512, #788 ),
 ( #17004, #25526, #23516 ),
 ( #25141, #5288, #1297 ),
 ( #2917, #6892, #16876 ),
 ( #17134, #14873, #23140 ) ),
 .UNSPECIFIED., .F., .F., .F. ) 
 B_SPLINE_SURFACE_WITH_KNOTS ( ( 4, 2, 4 ),
 ( 3, 3 ),
 ( 0.04143185595419456024, 0.04845767571923142308, 0.05548349548426828592 ),
 ( 0.000000000000000000, 1.000000000000000000 ),
 .UNSPECIFIED. ) 
 GEOMETRIC_REPRESENTATION_ITEM ( )  RATIONAL_B_SPLINE_SURFACE ( (
 ( 1.000000000000000000, 0.9541700779530466470, 1.000000000000000000),
 ( 1.000000000000000000, 0.9520118410151657828, 1.000000000000000000),
 ( 1.000000000000000000, 0.9503153331900817680, 1.000000000000000000),
 ( 1.000000000000000000, 0.9480088290653094774, 1.000000000000000000),
 ( 1.000000000000000000, 0.9474362546590832102, 1.000000000000000000),
 ( 1.000000000000000000, 0.9474350314971536902, 1.000000000000000000) ) ) 
 REPRESENTATION_ITEM ( '' )  SURFACE ( )  );
#25047 = EDGE_LOOP ( 'NONE', ( #9436, #6668, #8896, #23392 ) ) ;
#25048 = CARTESIAN_POINT ( 'NONE',  ( 200.0000000000000284, 4.759886302454138018, 18.40685213041688328 ) ) ;
#25049 = DIRECTION ( 'NONE',  ( 0.000000000000000000, 1.000000000000000000, 0.000000000000000000 ) ) ;
#25050 = ORIENTED_EDGE ( 'NONE', *, *, #21855, .T. ) ;
#25051 = VERTEX_POINT ( 'NONE', #10924 ) ;
#25052 = CARTESIAN_POINT ( 'NONE',  ( -86.96347745069644475, -43.67073346367983788, 12.89780903124397149 ) ) ;
#25053 = CARTESIAN_POINT ( 'NONE',  ( 199.0179304339989415, -16.54579169021749863, -11.23843401478282544 ) ) ;
#25054 = CARTESIAN_POINT ( 'NONE',  ( -114.7465989397623645, 2.774003790519791846, 21.93543632637892671 ) ) ;
#25055 = CARTESIAN_POINT ( 'NONE',  ( 4.995406935893294431, -17.50105314357198694, 39.06748935135188816 ) ) ;
#25056 = CARTESIAN_POINT ( 'NONE',  ( -105.4000354196369784, 20.24155804474649401, 6.858112701554157198 ) ) ;
#25057 = CARTESIAN_POINT ( 'NONE',  ( 200.0000000000000000, 40.00000000000012790, -19.99999999999996092 ) ) ;
#25058 = CARTESIAN_POINT ( 'NONE',  ( 190.0000000000000000, -61.50000000000001421, 66.50000000000005684 ) ) ;
#25059 = DIRECTION ( 'NONE',  ( -0.2259624730577678986, 0.9741360073262960162, 0.000000000000000000 ) ) ;
#25060 = CARTESIAN_POINT ( 'NONE',  ( -100.7734535825088500, -40.00000000000027711, 22.67402823373149801 ) ) ;
#25061 = CARTESIAN_POINT ( 'NONE',  ( -91.56559293963836410, 39.99999999999976552, 22.67402823373234000 ) ) ;
#25062 = CARTESIAN_POINT ( 'NONE',  ( -87.08360718067700645, 17.46847230663351525, 12.46771266860896255 ) ) ;
#25063 = DIRECTION ( 'NONE',  ( -1.000000000000000000, -1.836970198721030181E-16, 0.000000000000000000 ) ) ;
#25064 = CARTESIAN_POINT ( 'NONE',  ( 199.0087145623001277, 19.98798542585446469, 0.6659850717246563745 ) ) ;
#25065 = VECTOR ( 'NONE', #17506, 1000.000000000000000 ) ;
#25066 = CARTESIAN_POINT ( 'NONE',  ( -188.3065677117174914, 23.45084385698005391, 43.00727648871502140 ) ) ;
#25067 = CARTESIAN_POINT ( 'NONE',  ( 170.2234770963711128, -10.92277846919235529, 45.64576402573175073 ) ) ;
#25068 = CARTESIAN_POINT ( 'NONE',  ( -190.1935165880708496, -47.62328200654635424, 13.92226094463972963 ) ) ;
#25069 = CARTESIAN_POINT ( 'NONE',  ( -198.0356074513804572, 17.40982414986446969, 39.15871834505921356 ) ) ;
#25070 = CARTESIAN_POINT ( 'NONE',  ( -82.29192131168281321, -18.26745044309027222, 8.580784324611526515 ) ) ;
#25071 = CARTESIAN_POINT ( 'NONE',  ( -56.48582580120559982, 34.75652343174628101, -21.81201906317743067 ) ) ;
#25072 = CARTESIAN_POINT ( 'NONE',  ( 200.0000000000000000, 60.00000000000007105, 7.347880794884118356E-15 ) ) ;
#25073 = CARTESIAN_POINT ( 'NONE',  ( 151.7948205124835681, 33.23291073765556547, 40.00000000000002132 ) ) ;
#25074 = CARTESIAN_POINT ( 'NONE',  ( 19.06497207195980792, 10.03556273973447155, -10.03556273973422286 ) ) ;
#25075 = CARTESIAN_POINT ( 'NONE',  ( 192.4448373802101173, -19.99999999996057554, 40.00000000000002132 ) ) ;
#25076 = CARTESIAN_POINT ( 'NONE',  ( -86.86493150571116928, 19.77569912839177846, -7.943527260495974573 ) ) ;
#25077 = ORIENTED_EDGE ( 'NONE', *, *, #14186, .T. ) ;
#25078 = CARTESIAN_POINT ( 'NONE',  ( 200.0000000000000000, -39.99999999999977973, -20.00000000000034817 ) ) ;
#25079 = CARTESIAN_POINT ( 'NONE',  ( 199.0061245020890510, 7.715982321041501280, -18.44633997128330805 ) ) ;
#25080 = DIRECTION ( 'NONE',  ( -1.303213150798907793E-16, 1.000000000000000000, -1.682156097916904081E-16 ) ) ;
#25081 = ORIENTED_EDGE ( 'NONE', *, *, #2098, .T. ) ;
#25082 = ORIENTED_EDGE ( 'NONE', *, *, #18091, .T. ) ;
#25083 = VERTEX_POINT ( 'NONE', #22511 ) ;
#25084 = CARTESIAN_POINT ( 'NONE',  ( -100.7734535825088358, 17.32597176626809343, 2.449293598294708485E-15 ) ) ;
#25085 = CYLINDRICAL_SURFACE ( 'NONE', #5325, 5.000000000000004441 ) ;
#25086 = ADVANCED_FACE ( 'NONE', ( #22638 ), #19316, .F. ) ;
#25087 = AXIS2_PLACEMENT_3D ( 'NONE', #421, #6659, #6922 ) ;
#25088 = CARTESIAN_POINT ( 'NONE',  ( -105.3178975793522199, -20.76461410733032409, 5.416379678195457181 ) ) ;
#25089 = EDGE_CURVE ( 'NONE', #23960, #9969, #21199, .T. ) ;
#25090 = B_SPLINE_CURVE_WITH_KNOTS ( 'NONE', 3,
 ( #4689, #6532, #12792, #8936, #20918, #24645, #13185, #19673, #9562, #23672, #21306, #19808 ),
 .UNSPECIFIED., .F., .F.,
 ( 4, 2, 2, 2, 2, 4 ),
 ( 1.457502235237144910E-15, 0.004698945756008141884, 0.007048418634011504626, 0.009397891512014868234, 0.01409683726802163535, 0.01879578302402840420 ),
 .UNSPECIFIED. ) ;
#25091 = CARTESIAN_POINT ( 'NONE',  ( 160.7895100360861136, -20.14405787076863064, -20.14405787076872656 ) ) ;
#25092 =( BOUNDED_CURVE ( )  B_SPLINE_CURVE ( 3, ( #1938, #16158, #5787, #20028 ),
 .UNSPECIFIED., .F., .F. ) 
 B_SPLINE_CURVE_WITH_KNOTS ( ( 4, 4 ),
 ( 0.004183487405659287901, 0.01388163287021764933 ),
 .UNSPECIFIED. ) 
 CURVE ( )  GEOMETRIC_REPRESENTATION_ITEM ( )  RATIONAL_B_SPLINE_CURVE ( ( 0.6809743333591588010, 0.7608653435686177913, 0.8672072324488981909, 1.000000000000000000 ) ) 
 REPRESENTATION_ITEM ( '' )  );
#25093 = CARTESIAN_POINT ( 'NONE',  ( 151.7948205124836250, 1.439163438361279259E-13, -33.23291073765553705 ) ) ;
#25094 = CARTESIAN_POINT ( 'NONE',  ( 199.9999999999999147, -3.403913688674531812, -18.69557029314349705 ) ) ;
#25095 = EDGE_CURVE ( 'NONE', #12893, #7090, #18253, .T. ) ;
#25096 = CARTESIAN_POINT ( 'NONE',  ( 199.9999999999999147, 7.548244939093340378, -17.43950459141031573 ) ) ;
#25097 = CARTESIAN_POINT ( 'NONE',  ( -213.1075012329537230, 9.698598906438871126, -66.26714140136179765 ) ) ;
#25098 = CARTESIAN_POINT ( 'NONE',  ( -238.4067589809705794, -0.6820004457913585449, -0.6820004457913265705 ) ) ;
#25099 = DIRECTION ( 'NONE',  ( 0.000000000000000000, 1.000000000000000000, 0.000000000000000000 ) ) ;
#25100 = CARTESIAN_POINT ( 'NONE',  ( 200.0000000000000000, -39.99999999999977973, -20.00000000000034817 ) ) ;
#25101 = CARTESIAN_POINT ( 'NONE',  ( 190.0000000000000000, -52.49999999999972289, -82.49999999999998579 ) ) ;
#25102 = CARTESIAN_POINT ( 'NONE',  ( -259.2033419157646676, 9.517827891722584255, -0.000000000000000000 ) ) ;
#25103 = CARTESIAN_POINT ( 'NONE',  ( -208.1127848780264742, -10.60833733268345469, 67.17687982760682530 ) ) ;
#25104 = CARTESIAN_POINT ( 'NONE',  ( 199.0075046806690295, 19.82372177647270917, -2.703293726033221045 ) ) ;
#25106 = CARTESIAN_POINT ( 'NONE',  ( -198.0356074513804572, -9.007331120208026888E-14, 15.37879056873070560 ) ) ;
#25105 = CARTESIAN_POINT ( 'NONE',  ( 0.2972598230769938343, 10.13633138497486286, -10.13633138497461594 ) ) ;
#25107 = LINE ( 'NONE', #12985, #26196 ) ;
#25108 = CARTESIAN_POINT ( 'NONE',  ( 19.06497207195981858, 10.03556273973424062, 66.60410523465820631 ) ) ;
#25109 = CARTESIAN_POINT ( 'NONE',  ( 91.82158438592158234, -17.20528682183298486, 40.00000000000002132 ) ) ;
#25110 = B_SPLINE_CURVE_WITH_KNOTS ( 'NONE', 3,
 ( #18664, #18936, #23072, #718, #4713, #16670, #22803, #11081, #9083, #8554, #12949, #6687 ),
 .UNSPECIFIED., .F., .F.,
 ( 4, 2, 2, 2, 2, 4 ),
 ( 1.326269557315125156E-15, 0.004680202113614923519, 0.009360404227228521709, 0.01170050528403532124, 0.01404060634084211903, 0.01872080845445575625 ),
 .UNSPECIFIED. ) ;
#25111 = ORIENTED_EDGE ( 'NONE', *, *, #14339, .T. ) ;
#25112 = CARTESIAN_POINT ( 'NONE',  ( 12.77879914705803444, -44.80239647190084185, 18.55776024549615855 ) ) ;
#25113 = CARTESIAN_POINT ( 'NONE',  ( -135.8532207217289738, -9.153146818113595984, -40.00000000000002132 ) ) ;
#25114 = CARTESIAN_POINT ( 'NONE',  ( -87.02146317964799493, -10.86006974119950463, 18.50839211081909852 ) ) ;
#25115 = CARTESIAN_POINT ( 'NONE',  ( -238.4067589809705794, 0.6820004457912757223, 0.6820004457913219076 ) ) ;
#25116 = CARTESIAN_POINT ( 'NONE',  ( -77.90022806219006668, -8.352332316461408723, 20.16431395584796249 ) ) ;
#25117 = CARTESIAN_POINT ( 'NONE',  ( -82.24426486890021692, 20.04463774090378791, 2.459032291083046662 ) ) ;
#25118 = CARTESIAN_POINT ( 'NONE',  ( -62.62756078652115121, 10.52198127423075213, -25.40230989557676367 ) ) ;
#25119 = CARTESIAN_POINT ( 'NONE',  ( 199.0203632001705216, -18.77805633539013996, -6.891912269405206182 ) ) ;
#25120 = CARTESIAN_POINT ( 'NONE',  ( -56.48582580120559271, -6.472252184284276844, 6.472252184284108978 ) ) ;
#25121 = EDGE_CURVE ( 'NONE', #26265, #23307, #22552, .T. ) ;
#25122 = CARTESIAN_POINT ( 'NONE',  ( -77.55640685876514340, -22.13135000837104727, -2.449293598294710063E-15 ) ) ;
#25123 = CARTESIAN_POINT ( 'NONE',  ( -188.8532066752250671, -17.93248812771289380, 43.29285604501835394 ) ) ;
#25124 = CARTESIAN_POINT ( 'NONE',  ( -208.1127848780264742, 17.67593391476678377, -38.89260858015718014 ) ) ;
#25125 = CARTESIAN_POINT ( 'NONE',  ( -100.7734535825088500, 16.03295912088713848, -16.03295912088698927 ) ) ;
#25126 = CARTESIAN_POINT ( 'NONE',  ( 14.38125909742181285, -17.55144818341421598, -39.01709431150935359 ) ) ;
#25127 = CARTESIAN_POINT ( 'NONE',  ( 200.0000000000000000, 7.347880794884121511E-14, 0.000000000000000000 ) ) ;
#25129 = CARTESIAN_POINT ( 'NONE',  ( -86.96347745069644475, 12.89780903124419353, -12.89780903124389333 ) ) ;
#25128 = CARTESIAN_POINT ( 'NONE',  ( -100.7734535825088500, 44.31723036834907958, -12.25131212657445801 ) ) ;
#25130 = CARTESIAN_POINT ( 'NONE',  ( 170.2234770963711128, 10.92277846919216522, -10.92277846919186501 ) ) ;
#25131 = CARTESIAN_POINT ( 'NONE',  ( -105.3755690713226585, 21.75974354311648185, 40.00000000000002132 ) ) ;
#25132 = CARTESIAN_POINT ( 'NONE',  ( 192.4448373802101173, -20.00000000003938538, -40.00000000000002132 ) ) ;
#25133 = CARTESIAN_POINT ( 'NONE',  ( 184.8905102610680444, 13.49065550809817715, -43.07788698682574591 ) ) ;
#25134 = DIRECTION ( 'NONE',  ( 0.000000000000000000, -1.000000000000000000, 0.000000000000000000 ) ) ;
#25135 = CARTESIAN_POINT ( 'NONE',  ( 192.4448373802101173, -42.42640687116510634, 14.14213562375845257 ) ) ;
#25136 = AXIS2_PLACEMENT_3D ( 'NONE', #21637, #21514, #23388 ) ;
#25137 = CARTESIAN_POINT ( 'NONE',  ( -114.4364955367337444, 20.04994829327354822, -8.644468109217221752 ) ) ;
#25138 = ORIENTED_EDGE ( 'NONE', *, *, #1126, .T. ) ;
#25139 = CARTESIAN_POINT ( 'NONE',  ( -208.1127848780264742, 10.60833733270764867, 67.17687982763166588 ) ) ;
#25140 = AXIS2_PLACEMENT_3D ( 'NONE', #2047, #8277, #26133 ) ;
#25141 = CARTESIAN_POINT ( 'NONE',  ( -77.58456235491127018, -17.49514130593958328, -13.58502979129033328 ) ) ;
#25142 = CARTESIAN_POINT ( 'NONE',  ( -162.0762913951020607, -1.198031840455708430, 57.76657433537920383 ) ) ;
#25143 = CARTESIAN_POINT ( 'NONE',  ( -5.859158571312020669, -46.35984297724550629, -13.69949429424737275 ) ) ;
#25144 = ORIENTED_EDGE ( 'NONE', *, *, #25405, .T. ) ;
#25145 = DIRECTION ( 'NONE',  ( 1.000000000000000000, -1.836970198721030181E-16, -0.000000000000000000 ) ) ;
#25146 = CARTESIAN_POINT ( 'NONE',  ( -114.7544835083390780, -13.58506800096324163, -17.49509852148034383 ) ) ;
#25147 = CARTESIAN_POINT ( 'NONE',  ( 199.9999999999998863, 18.88157209772827017, -2.150785294275829429 ) ) ;
#25148 = CARTESIAN_POINT ( 'NONE',  ( -114.7827960788993096, -22.13220202243095969, 0.6714470530277172333 ) ) ;
#25149 = CARTESIAN_POINT ( 'NONE',  ( -135.8532207217289738, 30.84685318188643066, 2.449293598294708485E-15 ) ) ;
#25150 = FACE_OUTER_BOUND ( 'NONE', #17800, .T. ) ;
#25151 = CARTESIAN_POINT ( 'NONE',  ( 199.0188463327468185, 9.707946089746242180, 17.48826952134088941 ) ) ;
#25152 = CARTESIAN_POINT ( 'NONE',  ( -280.0000000000000000, 14.14213562373078581, 14.14213562373108424 ) ) ;
#25153 = CARTESIAN_POINT ( 'NONE',  ( 19.06497207195982924, -40.00000000000021316, 54.19242893257830218 ) ) ;
#25154 = CARTESIAN_POINT ( 'NONE',  ( 4.995406935893292655, 39.99999999999982947, 55.24977328856478209 ) ) ;
#25155 = DIRECTION ( 'NONE',  ( -1.000000000000000000, 1.836970198721030181E-16, 0.000000000000000000 ) ) ;
#25156 = CARTESIAN_POINT ( 'NONE',  ( -91.56559293963834989, -17.32597176626812185, -40.00000000000002132 ) ) ;
#25158 = CARTESIAN_POINT ( 'NONE',  ( 130.8568914410475372, 24.07718906447243867, -24.07718906447216156 ) ) ;
#25157 = CARTESIAN_POINT ( 'NONE',  ( 22.82148508083543348, -17.87803012130470748, -43.16138278736961098 ) ) ;
#25159 = CARTESIAN_POINT ( 'NONE',  ( 192.4448373802101173, -19.99999999996056843, -40.00000000000002132 ) ) ;
#25160 = CARTESIAN_POINT ( 'NONE',  ( 57.59792236341147031, 1.722363176415065089, -1.722363176415036445 ) ) ;
#25161 = CARTESIAN_POINT ( 'NONE',  ( 91.82158438592158234, -1.633484621919921769E-13, 17.20528682183300262 ) ) ;
#25162 = CARTESIAN_POINT ( 'NONE',  ( -175.9234121931127390, -21.03678983223290189, 39.35887396220598333 ) ) ;
#25163 = CARTESIAN_POINT ( 'NONE',  ( -56.48582580120557850, -39.99999999999970868, -30.84685318188687120 ) ) ;
#25164 = CARTESIAN_POINT ( 'NONE',  ( -91.56559293963834989, -16.03295912088706388, -16.03295912088710651 ) ) ;
#25165 = CARTESIAN_POINT ( 'NONE',  ( -53.37769371738423985, -27.95780717557995843, 13.65853730965386248 ) ) ;
#25166 = CARTESIAN_POINT ( 'NONE',  ( 192.4448373802100889, -14.14213562375896061, 14.14213562375865330 ) ) ;
#25167 = CARTESIAN_POINT ( 'NONE',  ( 163.1118516004056573, -9.006482792069636645, 9.006482792069567367 ) ) ;
#25168 = ORIENTED_EDGE ( 'NONE', *, *, #2256, .F. ) ;
#25170 = CARTESIAN_POINT ( 'NONE',  ( -6.342283169554576716, 46.19215417243025712, -13.66521761903544174 ) ) ;
#25169 = CARTESIAN_POINT ( 'NONE',  ( -87.01701082927731079, 18.46482525711258660, -10.86389608310530619 ) ) ;
#25171 = CARTESIAN_POINT ( 'NONE',  ( 189.9999999999999716, 82.50000000000008527, -52.49999999999977973 ) ) ;
#25172 = CARTESIAN_POINT ( 'NONE',  ( -162.0762913951020607, -41.69427287692683848, 40.00000000000002132 ) ) ;
#25173 = CARTESIAN_POINT ( 'NONE',  ( -362.0709805440841365, -4.857225732735059864E-14, 0.000000000000000000 ) ) ;
#25174 = CARTESIAN_POINT ( 'NONE',  ( -188.6013476421509552, 47.09841799633670689, -13.84412643133189391 ) ) ;
#25175 = ORIENTED_EDGE ( 'NONE', *, *, #12062, .T. ) ;
#25176 = ORIENTED_EDGE ( 'NONE', *, *, #22923, .T. ) ;
#25177 = AXIS2_PLACEMENT_3D ( 'NONE', #21799, #3572, #7682 ) ;
#25178 = CARTESIAN_POINT ( 'NONE',  ( 199.9999999999998863, -1.253919976928773661, 19.00818551405020784 ) ) ;
#25179 = CARTESIAN_POINT ( 'NONE',  ( -99.31267923331542136, 8.544756979562974308, -20.62886818714414616 ) ) ;
#25180 = ORIENTED_EDGE ( 'NONE', *, *, #11242, .F. ) ;
#25181 = ORIENTED_EDGE ( 'NONE', *, *, #24438, .F. ) ;
#25182 = PRODUCT_DEFINITION ( 'UNKNOWN', '', #12999, #13227 ) ;
#25183 = CARTESIAN_POINT ( 'NONE',  ( 91.82158438592158234, -12.16597498397761967, -12.16597498397768007 ) ) ;
#25184 = CARTESIAN_POINT ( 'NONE',  ( 199.0201284062958962, -18.60237515726647572, -7.352601386804158423 ) ) ;
#25185 = CARTESIAN_POINT ( 'NONE',  ( -114.4940140762809619, -7.440456728164089206, 20.58897208711081106 ) ) ;
#25186 = CARTESIAN_POINT ( 'NONE',  ( -238.4067589809705794, 0.6820004457340470561, 57.25054294065803617 ) ) ;
#25187 = DIRECTION ( 'NONE',  ( 1.000000000000000000, -0.000000000000000000, -0.000000000000000000 ) ) ;
#25188 = CARTESIAN_POINT ( 'NONE',  ( -259.2033419157646676, 40.00000000000000711, -9.517827891722491884 ) ) ;
#25189 = FACE_OUTER_BOUND ( 'NONE', #19427, .T. ) ;
#25190 = DIRECTION ( 'NONE',  ( 0.000000000000000000, 0.000000000000000000, 1.000000000000000000 ) ) ;
#25191 = EDGE_CURVE ( 'NONE', #25529, #12893, #3596, .T. ) ;
#25192 = CARTESIAN_POINT ( 'NONE',  ( 192.4448373802101173, -40.00000000000019185, 20.00000000003900524 ) ) ;
#25193 = CARTESIAN_POINT ( 'NONE',  ( 57.59792236341147031, 40.00000000000042633, -37.56421063658144277 ) ) ;
#25194 = CARTESIAN_POINT ( 'NONE',  ( -77.55640685875366103, 16.16066924852440678, 15.13778608694647332 ) ) ;
#25195 = CIRCLE ( 'NONE', #18368, 5.000000000000095035 ) ;
#25196 = CARTESIAN_POINT ( 'NONE',  ( -265.0000000000000000, -4.857225732735059864E-14, 0.000000000000000000 ) ) ;
#25197 = CARTESIAN_POINT ( 'NONE',  ( 199.0117592729713465, 18.59672480091233737, 7.361113620700817428 ) ) ;
#25198 = CARTESIAN_POINT ( 'NONE',  ( -199.9999999999999716, -44.86878812508714276, 24.82633483071253622 ) ) ;
#25199 = CARTESIAN_POINT ( 'NONE',  ( -280.0000000000000568, -14.14213562373137556, 42.42640687119276066 ) ) ;
#25200 = DIRECTION ( 'NONE',  ( 1.000000000000000000, 0.000000000000000000, 0.000000000000000000 ) ) ;
#25201 = CARTESIAN_POINT ( 'NONE',  ( -105.3755690713226727, 15.38646221621793231, -15.38646221621779020 ) ) ;
#25202 = CARTESIAN_POINT ( 'NONE',  ( -87.13368444202060914, -14.72469439729719554, 15.67192210925610496 ) ) ;
#25203 = CARTESIAN_POINT ( 'NONE',  ( -30.26275506840323359, -1.198031551615522439, -57.76657404653986561 ) ) ;
#25204 = CARTESIAN_POINT ( 'NONE',  ( -654.4889232350201382, 39.44889917058262796, 21.67367656778695917 ) ) ;
#25205 = DIRECTION ( 'NONE',  ( -1.000000000000000000, -1.836970198721030181E-16, 0.000000000000000000 ) ) ;
#25206 = ORIENTED_EDGE ( 'NONE', *, *, #19215, .F. ) ;
#25207 = CARTESIAN_POINT ( 'NONE',  ( -30.26275506840325136, 57.76657404653985139, -1.198031551615314161 ) ) ;
#25208 = CARTESIAN_POINT ( 'NONE',  ( -56.48582580120559271, 9.153146818113576444, -0.000000000000000000 ) ) ;
#25209 = CARTESIAN_POINT ( 'NONE',  ( -592.0438061236260410, 44.95394254848083904, 2.361432597285608725 ) ) ;
#25210 = ORIENTED_EDGE ( 'NONE', *, *, #19899, .T. ) ;
#25211 = CARTESIAN_POINT ( 'NONE',  ( -86.96347745069643054, -39.99999999999985079, -18.24025645688394448 ) ) ;
#25212 = CARTESIAN_POINT ( 'NONE',  ( 199.0105764394585890, -4.988040173753162776, -19.37759405569597959 ) ) ;
#25213 = CARTESIAN_POINT ( 'NONE',  ( 170.0000000000000853, -9.369682556672300322, 22.62041470344878746 ) ) ;
#25214 = VERTEX_POINT ( 'NONE', #7753 ) ;
#25215 = ORIENTED_EDGE ( 'NONE', *, *, #18249, .F. ) ;
#25216 = ORIENTED_EDGE ( 'NONE', *, *, #379, .T. ) ;
#25217 = CARTESIAN_POINT ( 'NONE',  ( -56.48582580120559271, 30.84685318188643066, 2.449293598294708485E-15 ) ) ;
#25218 = CARTESIAN_POINT ( 'NONE',  ( -114.4364955367323660, -8.064892380834915997, 20.29001642039123610 ) ) ;
#25219 = CARTESIAN_POINT ( 'NONE',  ( 199.9999999999999432, 1.065690307512836407E-13, -20.00000000000010303 ) ) ;
#25220 = CARTESIAN_POINT ( 'NONE',  ( 199.9999999999999147, 1.697088945475840660, -18.92594139730135439 ) ) ;
#25221 = CARTESIAN_POINT ( 'NONE',  ( 200.0000000000000000, 9.228668854417362510, -16.61132610550090760 ) ) ;
#25222 = CARTESIAN_POINT ( 'NONE',  ( 57.59792236341147031, -1.722363176414363206, -54.84617931850881689 ) ) ;
#25223 = CARTESIAN_POINT ( 'NONE',  ( 19.06497207195981147, -10.03556273973425483, -10.03556273973443247 ) ) ;
#25224 = DIRECTION ( 'NONE',  ( 1.000000000000000000, -0.000000000000000000, -0.000000000000000000 ) ) ;
#25225 = CARTESIAN_POINT ( 'NONE',  ( 130.8568914410475372, 8.880724697947696879E-14, -5.949712681206690945 ) ) ;
#25226 = CARTESIAN_POINT ( 'NONE',  ( 136.1360204305621266, 24.77266263493104148, 24.77266263493145004 ) ) ;
#25227 = CARTESIAN_POINT ( 'NONE',  ( -56.48582580120559271, 9.153146818113576444, -0.000000000000000000 ) ) ;
#25228 = CARTESIAN_POINT ( 'NONE',  ( 91.82158438592159655, -44.40256751092324095, -12.16597498400075139 ) ) ;
#25229 = CARTESIAN_POINT ( 'NONE',  ( 200.0000000000000000, 7.347880794884121511E-14, 0.000000000000000000 ) ) ;
#25230 = EDGE_CURVE ( 'NONE', #11453, #12520, #13448, .T. ) ;
#25232 = CARTESIAN_POINT ( 'NONE',  ( -238.4067589809705794, -4.716212492215116094E-14, 0.9644942799825824142 ) ) ;
#25231 = CARTESIAN_POINT ( 'NONE',  ( 57.59792236341147031, -1.722363176414363206, -54.84617931850881689 ) ) ;
#25233 = CARTESIAN_POINT ( 'NONE',  ( 200.0000000000000000, -20.00000000000006750, -40.00000000000002132 ) ) ;
#25234 = CARTESIAN_POINT ( 'NONE',  ( -280.0000000000000568, -14.14213562373108601, 42.42640687119285303 ) ) ;
#25235 = CARTESIAN_POINT ( 'NONE',  ( 91.82158438592158234, 22.79471317813471742, 40.00000000000002132 ) ) ;
#25236 = ORIENTED_EDGE ( 'NONE', *, *, #12545, .F. ) ;
#25237 = CARTESIAN_POINT ( 'NONE',  ( 11.38508063387934754, -44.88728980639579902, 24.83994849158430540 ) ) ;
#25238 = CARTESIAN_POINT ( 'NONE',  ( 91.82158438592158234, -17.20528682183298486, -40.00000000000002132 ) ) ;
#25239 = DIRECTION ( 'NONE',  ( 0.000000000000000000, -1.000000000000000000, 0.000000000000000000 ) ) ;
#25240 =( BOUNDED_SURFACE ( )  B_SPLINE_SURFACE ( 3, 2, ( 
 ( #21657, #19526, #17525 ),
 ( #23407, #19275, #13286 ),
 ( #15277, #5299, #13409 ),
 ( #3307, #3430, #25663 ),
 ( #11531, #9677, #21787 ),
 ( #1573, #3559, #25927 ) ),
 .UNSPECIFIED., .F., .F., .F. ) 
 B_SPLINE_SURFACE_WITH_KNOTS ( ( 4, 2, 4 ),
 ( 3, 3 ),
 ( 0.04143178499028438849, 0.04845752250266459338, 0.05548326001504480520 ),
 ( 0.000000000000000000, 1.000000000000000000 ),
 .UNSPECIFIED. ) 
 GEOMETRIC_REPRESENTATION_ITEM ( )  RATIONAL_B_SPLINE_SURFACE ( (
 ( 1.000000000000000000, 0.9541700779530452037, 1.000000000000000000),
 ( 1.000000000000000000, 0.9520119333866750022, 1.000000000000000000),
 ( 1.000000000000000000, 0.9503150296563032118, 1.000000000000000000),
 ( 1.000000000000000000, 0.9480088385138416562, 1.000000000000000000),
 ( 1.000000000000000000, 0.9474362539901676206, 1.000000000000000000),
 ( 1.000000000000000000, 0.9474350314971542453, 1.000000000000000000) ) ) 
 REPRESENTATION_ITEM ( '' )  SURFACE ( )  );
#25241 = CARTESIAN_POINT ( 'NONE',  ( 130.8568914410475372, 4.207082182992862407, 4.207082182992856190 ) ) ;
#25242 = CARTESIAN_POINT ( 'NONE',  ( 91.82158438592159655, -39.99999999999994316, -17.20528682183314118 ) ) ;
#25243 = CARTESIAN_POINT ( 'NONE',  ( -77.90255099906774205, 20.29001641120652621, -8.064892378658626626 ) ) ;
#25244 = CARTESIAN_POINT ( 'NONE',  ( 12.01676479903291650, -14.17570730777163668, -49.30523874212537550 ) ) ;
#25245 = CARTESIAN_POINT ( 'NONE',  ( 199.0234688043258018, -20.00162938710794691, 0.3307560783973806373 ) ) ;
#25246 = CARTESIAN_POINT ( 'NONE',  ( -198.0356074513804572, 67.44298959250878056, -10.87444709758402261 ) ) ;
#25247 = FACE_OUTER_BOUND ( 'NONE', #10564, .T. ) ;
#25248 = SURFACE_STYLE_FILL_AREA ( #12599 ) ;
#25249 = CARTESIAN_POINT ( 'NONE',  ( -259.2033419157646676, 6.730120644403521979, -6.730120644403498886 ) ) ;
#25250 = CARTESIAN_POINT ( 'NONE',  ( 163.1118516004056573, 19.27778845538753316, 19.27778845538783870 ) ) ;
#25251 = CIRCLE ( 'NONE', #11622, 5.000000000000004441 ) ;
#25252 = CARTESIAN_POINT ( 'NONE',  ( 184.8905102610680444, 43.07788698682572459, 13.49065550809829439 ) ) ;
#25253 = DIRECTION ( 'NONE',  ( -1.000000000000000000, 1.836970198721030181E-16, 0.000000000000000000 ) ) ;
#25254 = CARTESIAN_POINT ( 'NONE',  ( -114.4364955367328349, 20.29001642038852538, -8.064892380842216824 ) ) ;
#25256 = CARTESIAN_POINT ( 'NONE',  ( -259.2033419157646676, 49.83842185052017015, 6.730120644404137487 ) ) ;
#25255 = CARTESIAN_POINT ( 'NONE',  ( -200.4318156386386534, 24.83634777281940487, -44.88237417767393111 ) ) ;
#25257 = CARTESIAN_POINT ( 'NONE',  ( -91.56559293963834989, -16.03295912088659492, -40.53558337403696044 ) ) ;
#25258 = CARTESIAN_POINT ( 'NONE',  ( -56.48582580120559982, -9.153146818113595984, -40.00000000000002132 ) ) ;
#25259 = CARTESIAN_POINT ( 'NONE',  ( -86.96347745069644475, 12.89780903124410472, -43.67073346367977393 ) ) ;
#25260 = ADVANCED_FACE ( 'NONE', ( #23860 ), #22746, .T. ) ;
#25261 = CARTESIAN_POINT ( 'NONE',  ( -280.0000000000000000, 1.839446121267387017E-14, -20.00000000000001421 ) ) ;
#25262 = CARTESIAN_POINT ( 'NONE',  ( -208.1127848780264742, -67.17687982760682530, -10.60833733268364298 ) ) ;
#25263 = EDGE_CURVE ( 'NONE', #11173, #2989, #13594, .T. ) ;
#25264 = CARTESIAN_POINT ( 'NONE',  ( -83.21262154144228873, -33.12752917117752105, 13.72187187063023650 ) ) ;
#25265 = ORIENTED_EDGE ( 'NONE', *, *, #6208, .F. ) ;
#25266 = CARTESIAN_POINT ( 'NONE',  ( -100.7734535825088358, 12.25131212657480440, 12.25131212657487012 ) ) ;
#25267 = CARTESIAN_POINT ( 'NONE',  ( -16.41532015104117193, 42.70629200743962173, -12.95569205199923957 ) ) ;
#25268 = CARTESIAN_POINT ( 'NONE',  ( -56.48582580120559982, 34.75652343174597547, 21.81201906317791384 ) ) ;
#25269 = CARTESIAN_POINT ( 'NONE',  ( -4.081455915266338330, -43.13234798823421556, -17.86600351372032591 ) ) ;
#25270 = EDGE_CURVE ( 'NONE', #7651, #16549, #25942, .T. ) ;
#25271 = EDGE_CURVE ( 'NONE', #25810, #20782, #13130, .T. ) ;
#25272 = ORIENTED_EDGE ( 'NONE', *, *, #17665, .T. ) ;
#25273 = CARTESIAN_POINT ( 'NONE',  ( -187.7698581930904140, -42.84913646251419550, 23.34605429454595082 ) ) ;
#25274 = CARTESIAN_POINT ( 'NONE',  ( 200.0000000000001705, -16.91021041590709473, -8.683373960011902426 ) ) ;
#25275 = CARTESIAN_POINT ( 'NONE',  ( 90.71511022971527893, -8.335579104983011689, 21.46756116496406364 ) ) ;
#25276 = CARTESIAN_POINT ( 'NONE',  ( -213.1075012329537230, 13.71589010951907817, -40.00000000000002132 ) ) ;
#25277 = CARTESIAN_POINT ( 'NONE',  ( 67.90397382968500040, 14.12691053360184412, -28.69135535065072773 ) ) ;
#25278 = CARTESIAN_POINT ( 'NONE',  ( 199.0116003924211725, 18.71458825927322422, 7.055789865482638312 ) ) ;
#25279 = CARTESIAN_POINT ( 'NONE',  ( -105.3755690713226585, -12.89780903124444578, 43.67073346367968156 ) ) ;
#25280 = CARTESIAN_POINT ( 'NONE',  ( 4.995406935893298872, -1.944352046434030652E-13, 55.24977328854835434 ) ) ;
#25281 = CARTESIAN_POINT ( 'NONE',  ( -716.9846540392142060, 0.000000000000000000, 0.000000000000000000 ) ) ;
#25282 = CARTESIAN_POINT ( 'NONE',  ( -199.9999999999999147, -19.98641303047005024, -45.65206365911544140 ) ) ;
#25283 = CARTESIAN_POINT ( 'NONE',  ( -30.26275506840323004, -41.69427246844627888, -40.00000000000002132 ) ) ;
#25285 = CARTESIAN_POINT ( 'NONE',  ( -604.6053156620442905, 34.65218274561313905, 19.98475300726100201 ) ) ;
#25284 = CARTESIAN_POINT ( 'NONE',  ( 21.60666276257293461, -18.00814241471057642, -43.47550165074667916 ) ) ;
#25286 = CARTESIAN_POINT ( 'NONE',  ( -213.1075012329537230, -13.71589010951915810, 40.00000000000002132 ) ) ;
#25287 = CARTESIAN_POINT ( 'NONE',  ( 146.6084372240433709, 52.76785682606519146, 3.800685668858932775 ) ) ;
#25288 = CARTESIAN_POINT ( 'NONE',  ( -56.48582580120559982, 40.00000000000034106, -30.84685318188602210 ) ) ;
#25289 = CARTESIAN_POINT ( 'NONE',  ( -110.0822598093739657, 11.09289860106540893, -16.86905266168659523 ) ) ;
#25290 = CARTESIAN_POINT ( 'NONE',  ( 91.82158438592159655, -40.00000000000017764, 17.20528682183258340 ) ) ;
#25291 = CARTESIAN_POINT ( 'NONE',  ( 199.0256575778758474, -7.963596585350240176, 18.35421432800287533 ) ) ;
#25292 = DIRECTION ( 'NONE',  ( 0.000000000000000000, 0.000000000000000000, 1.000000000000000000 ) ) ;
#25293 = CARTESIAN_POINT ( 'NONE',  ( -208.1127848780264742, 67.17687982763172272, -10.60833733270698254 ) ) ;
#25294 = CARTESIAN_POINT ( 'NONE',  ( 136.1360204305621266, 53.05693388239316022, 3.511608612530967566 ) ) ;
#25295 = EDGE_LOOP ( 'NONE', ( #19423, #18276, #25910, #9476 ) ) ;
#25297 = CARTESIAN_POINT ( 'NONE',  ( 6.615221834188973027, 49.23097633541777185, -14.16446777330068763 ) ) ;
#25296 = CARTESIAN_POINT ( 'NONE',  ( -210.0000000000000284, 75.52305771588336825, -68.47933392563552957 ) ) ;
#25298 = CARTESIAN_POINT ( 'NONE',  ( 158.3379117892987438, 26.51167085133959134, -10.98149362779631666 ) ) ;
#25299 = CARTESIAN_POINT ( 'NONE',  ( 184.8905102610680444, -19.07866798485555293, -2.449293598294708485E-15 ) ) ;
#25300 = CARTESIAN_POINT ( 'NONE',  ( -188.3610564113212149, 47.01267209787937418, -13.83140491817310824 ) ) ;
#25301 = APPLICATION_PROTOCOL_DEFINITION ( 'draft international standard', 'automotive_design', 1998, #9846 ) ;
#25302 = VERTEX_POINT ( 'NONE', #14809 ) ;
#25303 = ORIENTED_EDGE ( 'NONE', *, *, #1200, .F. ) ;
#25304 = CARTESIAN_POINT ( 'NONE',  ( -192.9588430854689989, -10.23066800230756890, 10.23066800230742501 ) ) ;
#25305 = CARTESIAN_POINT ( 'NONE',  ( 146.5090579137181805, 12.40347562390462066, -29.94463907179407514 ) ) ;
#25306 = CARTESIAN_POINT ( 'NONE',  ( 130.8568914410475372, 1.429239637432775288E-13, -34.05028731879788495 ) ) ;
#25307 = ORIENTED_EDGE ( 'NONE', *, *, #21220, .T. ) ;
#25308 = CARTESIAN_POINT ( 'NONE',  ( 199.9999999999999716, -3.868950841772955673, 18.61236034055575317 ) ) ;
#25309 = COLOUR_RGB ( '',0.7921568627450980005, 0.8196078431372548767, 0.9333333333333333481 ) ;
#25310 = AXIS2_PLACEMENT_3D ( 'NONE', #4052, #5631, #14803 ) ;
#25311 = CARTESIAN_POINT ( 'NONE',  ( -83.21262154144248768, 33.12752917118412199, -13.72187187061503444 ) ) ;
#25312 = CARTESIAN_POINT ( 'NONE',  ( 57.59792236341147031, -30.00663442387700641, 26.56190807104681895 ) ) ;
#25313 = CARTESIAN_POINT ( 'NONE',  ( 170.2234770963711128, -17.36149277826985937, -17.36149277826995174 ) ) ;
#25314 = CARTESIAN_POINT ( 'NONE',  ( 130.8568914410475088, 40.00000000000015632, -34.05028731879774284 ) ) ;
#25315 = CYLINDRICAL_SURFACE ( 'NONE', #20256, 30.00000000000003908 ) ;
#25316 = FACE_BOUND ( 'NONE', #15771, .T. ) ;
#25317 = CARTESIAN_POINT ( 'NONE',  ( -192.9588430854690273, -39.99999999999948841, -54.46834944098263520 ) ) ;
#25318 = AXIS2_PLACEMENT_3D ( 'NONE', #12543, #16937, #24943 ) ;
#25319 = CARTESIAN_POINT ( 'NONE',  ( 4.995406935893298872, 5.820775922023080204E-13, -55.24977328854835434 ) ) ;
#25320 = CARTESIAN_POINT ( 'NONE',  ( -77.59736708337840128, 17.53068837882001674, 13.45304834675272332 ) ) ;
#25321 = CARTESIAN_POINT ( 'NONE',  ( -213.1075012329537230, -66.26714140138676612, 9.698598906462487790 ) ) ;
#25322 = DIRECTION ( 'NONE',  ( 0.000000000000000000, -0.9166903767334039221, -0.3995982397413309073 ) ) ;
#25323 = CARTESIAN_POINT ( 'NONE',  ( -200.4317933031571499, 24.83634732651995236, 44.88237357214655532 ) ) ;
#25324 = CARTESIAN_POINT ( 'NONE',  ( -348.0000000000001137, -4.857225732735059864E-14, 28.79780246617542616 ) ) ;
#25325 = CARTESIAN_POINT ( 'NONE',  ( -109.1264249741459480, -33.12752917269222763, 13.72187187123999053 ) ) ;
#25326 = CARTESIAN_POINT ( 'NONE',  ( 91.82158438592158234, 12.16597498397773869, -12.16597498397759303 ) ) ;
#25327 = CARTESIAN_POINT ( 'NONE',  ( -82.23866184892956710, -13.36787606754601399, 15.15017645652793199 ) ) ;
#25328 = VECTOR ( 'NONE', #6704, 1000.000000000000000 ) ;
#25329 = CIRCLE ( 'NONE', #17231, 5.000000000000004441 ) ;
#25330 = CARTESIAN_POINT ( 'NONE',  ( -259.2033419157646676, -21.55415060305872998, 35.01439189186525880 ) ) ;
#25331 = CARTESIAN_POINT ( 'NONE',  ( -641.7036307566764890, 31.87148209193353665, -31.77421052347908415 ) ) ;
#25332 = CARTESIAN_POINT ( 'NONE',  ( -87.13361725327075646, 15.19799821270843765, 15.19799821270837015 ) ) ;
#25333 = ORIENTED_EDGE ( 'NONE', *, *, #2014, .F. ) ;
#25334 = CARTESIAN_POINT ( 'NONE',  ( 199.9999999999999432, -14.14213562373115884, 14.14213562373085153 ) ) ;
#25335 = FACE_OUTER_BOUND ( 'NONE', #2166, .T. ) ;
#25336 = CARTESIAN_POINT ( 'NONE',  ( -619.2650551519561759, 29.31345288821323791, 34.14316883558051074 ) ) ;
#25337 = ORIENTED_EDGE ( 'NONE', *, *, #17104, .T. ) ;
#25338 =( REPRESENTATION_RELATIONSHIP ('NONE','NONE', #23888, #9131 ) REPRESENTATION_RELATIONSHIP_WITH_TRANSFORMATION ( #24740 )SHAPE_REPRESENTATION_RELATIONSHIP( ) );
#25339 = CARTESIAN_POINT ( 'NONE',  ( -135.8532207217289738, 3.005970985514575011E-13, -30.84685318188645553 ) ) ;
#25340 = CARTESIAN_POINT ( 'NONE',  ( 199.0232538779058302, -20.00218003532801703, -0.2559617245760326676 ) ) ;
#25341 = CARTESIAN_POINT ( 'NONE',  ( -199.9999999999999432, -4.865628651907146107, -55.16984130227028515 ) ) ;
#25342 = VECTOR ( 'NONE', #4072, 1000.000000000000000 ) ;
#25343 = ORIENTED_EDGE ( 'NONE', *, *, #1264, .T. ) ;
#25344 = ORIENTED_EDGE ( 'NONE', *, *, #12400, .T. ) ;
#25345 = CARTESIAN_POINT ( 'NONE',  ( -213.1075012329537230, 53.71589010950162191, -40.00000000000002132 ) ) ;
#25346 = EDGE_CURVE ( 'NONE', #24441, #17844, #16571, .T. ) ;
#25347 = CARTESIAN_POINT ( 'NONE',  ( -103.9663809734175999, -20.15238534381313684, -8.026122150562576607 ) ) ;
#25348 = CARTESIAN_POINT ( 'NONE',  ( -77.70077460412316839, -11.21025402036352325, 18.98542998413487837 ) ) ;
#25349 = CARTESIAN_POINT ( 'NONE',  ( 192.4448373802100889, 1.051811698935164031E-13, -20.00000000003942091 ) ) ;
#25350 = CARTESIAN_POINT ( 'NONE',  ( 200.0000000000000000, -14.79283710360616944, -11.93388616463377438 ) ) ;
#25351 = EDGE_CURVE ( 'NONE', #15984, #4199, #459, .T. ) ;
#25352 = VECTOR ( 'NONE', #15912, 1000.000000000000000 ) ;
#25353 = CARTESIAN_POINT ( 'NONE',  ( -626.9846540392142060, 26.45751311064579880, -30.00000000000005329 ) ) ;
#25354 = CARTESIAN_POINT ( 'NONE',  ( -40.07203023092074545, -16.33025453607757882, -32.10811084135991678 ) ) ;
#25355 = CARTESIAN_POINT ( 'NONE',  ( -135.8532207217289738, 34.75652343174625258, -21.81201906317744132 ) ) ;
#25356 = CARTESIAN_POINT ( 'NONE',  ( -99.31680025536471135, 20.62455315994730398, 8.542969636735133321 ) ) ;
#25357 = CARTESIAN_POINT ( 'NONE',  ( -259.2033419157646676, -39.99999999999975131, -30.48217210827782608 ) ) ;
#25358 = CARTESIAN_POINT ( 'NONE',  ( 163.1118516004056573, -9.006482792074626431, 47.56205970284951690 ) ) ;
#25359 = CARTESIAN_POINT ( 'NONE',  ( -198.0356074513804572, -15.37879056873074290, -40.00000000000002132 ) ) ;
#25360 = EDGE_CURVE ( 'NONE', #12649, #18983, #20434, .T. ) ;
#25361 = CARTESIAN_POINT ( 'NONE',  ( 14.38125909742181996, -10.73282306403606157, 67.30136555895948902 ) ) ;
#25362 = CARTESIAN_POINT ( 'NONE',  ( 130.8568914410475088, 34.05028731879790627, -40.00000000000002132 ) ) ;
#25364 = CARTESIAN_POINT ( 'NONE',  ( 184.8905102610680444, 39.99999999999999289, 19.07866798485573057 ) ) ;
#25363 = CARTESIAN_POINT ( 'NONE',  ( 19.06497207195981858, 10.03556273973516078, -66.60410523465806421 ) ) ;
#25365 = VECTOR ( 'NONE', #1094, 1000.000000000000000 ) ;
#25366 = CARTESIAN_POINT ( 'NONE',  ( 136.1360204305621551, -35.03383547441293899, -40.00000000000002132 ) ) ;
#25367 = CARTESIAN_POINT ( 'NONE',  ( 163.1118516004056573, -47.56205970284957374, 9.006482792074162802 ) ) ;
#25368 = CARTESIAN_POINT ( 'NONE',  ( -238.4067589809705794, 40.96449428006337001, -40.00000000000002132 ) ) ;
#25369 = VERTEX_POINT ( 'NONE', #1111 ) ;
#25370 = ADVANCED_FACE ( 'NONE', ( #13583 ), #17705, .F. ) ;
#25371 = CARTESIAN_POINT ( 'NONE',  ( -1.087763065864006062, -47.95583523903733436, 13.97201973055748603 ) ) ;
#25372 = CARTESIAN_POINT ( 'NONE',  ( 192.4448373802100889, 19.99999999996064304, 2.449293598294708485E-15 ) ) ;
#25373 = CARTESIAN_POINT ( 'NONE',  ( -210.0000000000000284, -82.49999999999990052, 52.49999999999977263 ) ) ;
#25374 = CIRCLE ( 'NONE', #19817, 29.99999999999999289 ) ;
#25375 = CARTESIAN_POINT ( 'NONE',  ( 0.2972598230770011618, 10.13633138497462305, 66.70487387989858519 ) ) ;
#25376 = CARTESIAN_POINT ( 'NONE',  ( -238.4067589809705794, -40.00000000000007105, 0.9644942799824426372 ) ) ;
#25377 = CARTESIAN_POINT ( 'NONE',  ( -87.05902966484931937, 21.00921308708589308, -4.297868118821011940 ) ) ;
#25378 = CARTESIAN_POINT ( 'NONE',  ( -5.859158571311539276, 13.69949429424878851, -46.35984297724471048 ) ) ;
#25379 = CARTESIAN_POINT ( 'NONE',  ( 200.0000000000000000, -3.101357108925543837, 18.75734389255849521 ) ) ;
#25380 = CARTESIAN_POINT ( 'NONE',  ( -642.9364793054111260, 30.88727062095852816, -25.42494723607509499 ) ) ;
#25381 = CARTESIAN_POINT ( 'NONE',  ( -87.10570614283763291, 2.723277571087649118, -21.31140251566250399 ) ) ;
#25382 = CARTESIAN_POINT ( 'NONE',  ( 151.7948205124836250, -23.49921654116371883, 23.49921654116317526 ) ) ;
#25383 = CARTESIAN_POINT ( 'NONE',  ( -162.0762913951021176, 27.08623940707639477, -29.48230308784743059 ) ) ;
#25384 = CARTESIAN_POINT ( 'NONE',  ( -91.56559293963836410, 44.31723036834890905, 12.25131212657507795 ) ) ;
#25385 = DIRECTION ( 'NONE',  ( -1.000000000000000000, 0.000000000000000000, 0.000000000000000000 ) ) ;
#25386 = CARTESIAN_POINT ( 'NONE',  ( -135.8532207217289738, 6.472252184284096543, 6.472252184284234211 ) ) ;
#25388 = CARTESIAN_POINT ( 'NONE',  ( -30.26275506840324070, -27.08623969584554558, -29.48230279907826912 ) ) ;
#25387 = CARTESIAN_POINT ( 'NONE',  ( -100.7734535825088500, 16.03295912088691821, 16.03295912088721309 ) ) ;
#25389 = CARTESIAN_POINT ( 'NONE',  ( -86.96347745069644475, 41.18208027870576871, 15.38646221621837107 ) ) ;
#25390 = CARTESIAN_POINT ( 'NONE',  ( 151.7948205124836534, 6.767089262349062828, -40.00000000000002132 ) ) ;
#25391 = CARTESIAN_POINT ( 'NONE',  ( -30.26275506840324070, 1.198031551616013601, 1.198031551616023371 ) ) ;
#25392 = AXIS2_PLACEMENT_3D ( 'NONE', #25281, #1188, #7289 ) ;
#25393 = CARTESIAN_POINT ( 'NONE',  ( -135.8532207217289738, 7.002209520526292428E-15, -9.153146818113572891 ) ) ;
#25394 = CARTESIAN_POINT ( 'NONE',  ( 136.1360204305621551, -31.79587985999279454, 24.77266263493094911 ) ) ;
#25395 = CARTESIAN_POINT ( 'NONE',  ( -129.2920181227953549, 25.26067667711114950, -10.46331487475240074 ) ) ;
#25396 = EDGE_LOOP ( 'NONE', ( #23548, #17335, #5572, #3846, #19178, #12553 ) ) ;
#25397 = CARTESIAN_POINT ( 'NONE',  ( 192.4448373802100889, 14.14213562370310662, 14.14213562370312438 ) ) ;
#25398 = CARTESIAN_POINT ( 'NONE',  ( -53.37769371643639715, 29.42719939405414920, -10.11111068829008275 ) ) ;
#25399 = CARTESIAN_POINT ( 'NONE',  ( 23.42154907652747298, 23.32998349128558147, 42.84253412640366321 ) ) ;
#25400 = CARTESIAN_POINT ( 'NONE',  ( -70.30307074924525068, -23.14841682968063452, -8.711708293734362840 ) ) ;
#25401 = ORIENTED_EDGE ( 'NONE', *, *, #9331, .T. ) ;
#25402 = CARTESIAN_POINT ( 'NONE',  ( -121.8425418806976381, -22.74408238789939674, 9.420907390773301415 ) ) ;
#25403 = CARTESIAN_POINT ( 'NONE',  ( 200.0000000000001137, -16.46591192518303970, -9.498466322123544359 ) ) ;
#25404 = CARTESIAN_POINT ( 'NONE',  ( 23.35928221536216398, -13.80178577956153063, 46.81377789283308033 ) ) ;
#25405 = EDGE_CURVE ( 'NONE', #13305, #20820, #18832, .T. ) ;
#25406 = CARTESIAN_POINT ( 'NONE',  ( 199.0076515966382260, 19.86999350167783263, -2.263549309587763680 ) ) ;
#25407 = ADVANCED_FACE ( 'NONE', ( #1627 ), #1371, .F. ) ;
#25408 = CARTESIAN_POINT ( 'NONE',  ( -162.0762913951021176, -29.48230308784793152, 27.08623940707591515 ) ) ;
#25409 = CARTESIAN_POINT ( 'NONE',  ( -105.3755690713226585, 40.00000000000007816, -21.75974354311636461 ) ) ;
#25410 = CARTESIAN_POINT ( 'NONE',  ( -162.0762913951020892, -3.568845385355699554E-14, 1.694272876828323948 ) ) ;
#25411 = DIRECTION ( 'NONE',  ( 0.000000000000000000, 1.000000000000000000, 0.000000000000000000 ) ) ;
#25412 = CARTESIAN_POINT ( 'NONE',  ( -162.0762913951020607, -41.69427287682838568, -2.449293598294708485E-15 ) ) ;
#25414 = CARTESIAN_POINT ( 'NONE',  ( -624.9005621318009389, 26.45751311064577749, 30.00000000000004974 ) ) ;
#25413 = CARTESIAN_POINT ( 'NONE',  ( 20.69615274309022723, -13.93598092274699773, -47.71500688528268341 ) ) ;
#25415 = EDGE_CURVE ( 'NONE', #10231, #22478, #10925, .T. ) ;
#25416 = CARTESIAN_POINT ( 'NONE',  ( -259.2033419157646676, 9.517827891722584255, -0.000000000000000000 ) ) ;
#25417 = EDGE_CURVE ( 'NONE', #15830, #14785, #12759, .T. ) ;
#25418 = CARTESIAN_POINT ( 'NONE',  ( 163.1118516004056573, 47.56205970284957374, 9.006482792074494981 ) ) ;
#25419 = CARTESIAN_POINT ( 'NONE',  ( 14.38125909742180930, 40.00000000000060396, -55.17850393974224232 ) ) ;
#25420 = CARTESIAN_POINT ( 'NONE',  ( -105.4293522940765229, 9.002736003387274977, -19.36070119847539672 ) ) ;
#25421 = CARTESIAN_POINT ( 'NONE',  ( 19.06497207195981858, -39.99999999999987210, -14.19242893257882621 ) ) ;
#25422 = CARTESIAN_POINT ( 'NONE',  ( 118.9119131903919993, -25.80655941808602094, -10.68942690915843841 ) ) ;
#25423 = CARTESIAN_POINT ( 'NONE',  ( -208.1127848780264742, 38.89260858015707356, 17.67593391476696141 ) ) ;
#25424 = CARTESIAN_POINT ( 'NONE',  ( -208.1127848780264742, -10.60833733268345469, 67.17687982760682530 ) ) ;
#25425 = EDGE_LOOP ( 'NONE', ( #19587, #8940 ) ) ;
#25427 = CARTESIAN_POINT ( 'NONE',  ( 12.96694272564693406, 49.19577900140143356, -14.15914421027473047 ) ) ;
#25426 = DIRECTION ( 'NONE',  ( -1.000000000000000000, -1.836970198721030181E-16, 0.000000000000000000 ) ) ;
#25428 = CARTESIAN_POINT ( 'NONE',  ( 151.7948205124835681, 33.23291073765556547, 40.00000000000002132 ) ) ;
#25429 = PRESENTATION_STYLE_ASSIGNMENT (( #9309 ) ) ;
#25430 = CARTESIAN_POINT ( 'NONE',  ( -189.1815713358188304, 43.37724571962049680, -17.96744347545783427 ) ) ;
#25431 = DIRECTION ( 'NONE',  ( 1.000000000000000000, 0.000000000000000000, 0.000000000000000000 ) ) ;
#25432 = ORIENTED_EDGE ( 'NONE', *, *, #17354, .T. ) ;
#25433 = ORIENTED_EDGE ( 'NONE', *, *, #13609, .F. ) ;
#25434 = CARTESIAN_POINT ( 'NONE',  ( 19.06497207195981147, -10.03556273973439517, 10.03556273973429214 ) ) ;
#25435 = DIRECTION ( 'NONE',  ( -1.000000000000000000, -1.836970198721030427E-16, 0.000000000000000000 ) ) ;
#25436 = CARTESIAN_POINT ( 'NONE',  ( -88.39148973765155404, 8.027153355909614874, -20.15708830332384949 ) ) ;
#25437 = ORIENTED_EDGE ( 'NONE', *, *, #24118, .F. ) ;
#25438 = CARTESIAN_POINT ( 'NONE',  ( 199.9999999999999147, -9.100092698529554269, 16.69133291234032868 ) ) ;
#25439 = LINE ( 'NONE', #25689, #10271 ) ;
#25440 = CARTESIAN_POINT ( 'NONE',  ( -280.0000000000000568, -14.14213562373108601, 42.42640687119285303 ) ) ;
#25441 = CARTESIAN_POINT ( 'NONE',  ( 136.1360204305621266, 1.473277640373554421E-13, -35.03383547441296741 ) ) ;
#25442 = ADVANCED_FACE ( 'NONE', ( #11337 ), #13717, .F. ) ;
#25443 = DIRECTION ( 'NONE',  ( 1.000000000000000000, 1.836970198721030181E-16, -0.000000000000000000 ) ) ;
#25444 = DIRECTION ( 'NONE',  ( 0.000000000000000000, 1.000000000000000000, 0.000000000000000000 ) ) ;
#25445 = CARTESIAN_POINT ( 'NONE',  ( 192.4448373802100889, 2.472897170449861688E-13, -19.99999999996060751 ) ) ;
#25446 = CARTESIAN_POINT ( 'NONE',  ( -105.3755690713226585, 40.00000000000019185, -18.24025645688310249 ) ) ;
#25447 = CARTESIAN_POINT ( 'NONE',  ( -105.3846709045749890, -19.12138504414901519, 9.637707283831149496 ) ) ;
#25448 = CARTESIAN_POINT ( 'NONE',  ( -192.9588430854690273, -38.51493924976932703, -18.05360324515463688 ) ) ;
#25449 = FACE_OUTER_BOUND ( 'NONE', #10635, .T. ) ;
#25450 = EDGE_CURVE ( 'NONE', #24210, #555, #9345, .T. ) ;
#25451 = CARTESIAN_POINT ( 'NONE',  ( -163.5815475691942140, 35.61501186087246396, -18.59457173339175284 ) ) ;
#25452 = DIRECTION ( 'NONE',  ( 0.000000000000000000, 0.000000000000000000, 1.000000000000000000 ) ) ;
#25453 = AXIS2_PLACEMENT_3D ( 'NONE', #15886, #24014, #7515 ) ;
#25454 = CARTESIAN_POINT ( 'NONE',  ( -77.55625318716889183, 15.17516088037486277, -16.12447834766239296 ) ) ;
#25455 = LINE ( 'NONE', #5222, #1718 ) ;
#25456 = CARTESIAN_POINT ( 'NONE',  ( -87.02115643449447191, -10.85297647556013345, 18.51269039639111824 ) ) ;
#25457 = CARTESIAN_POINT ( 'NONE',  ( -100.7734535825088358, 12.25131212657480440, 12.25131212657487012 ) ) ;
#25458 = CARTESIAN_POINT ( 'NONE',  ( 19.06497207195982924, -66.60410523465809263, -10.03556273973493163 ) ) ;
#25459 = CARTESIAN_POINT ( 'NONE',  ( -114.4364955367313428, -8.644468109216784768, -20.04994829327278438 ) ) ;
#25460 = LINE ( 'NONE', #1107, #22359 ) ;
#25461 = ORIENTED_EDGE ( 'NONE', *, *, #13064, .F. ) ;
#25462 = CARTESIAN_POINT ( 'NONE',  ( -238.4067589809705794, 0.6820004458491113475, -57.25054294077229144 ) ) ;
#25463 = CARTESIAN_POINT ( 'NONE',  ( 170.0000000000428315, 17.64300463311351308, -17.64300463311329992 ) ) ;
#25464 = DIRECTION ( 'NONE',  ( 1.000000000000000000, 1.836970198721030427E-16, -0.000000000000000000 ) ) ;
#25465 = VERTEX_POINT ( 'NONE', #17453 ) ;
#25466 = CARTESIAN_POINT ( 'NONE',  ( 192.4448373802101173, -40.00000000000019185, 20.00000000003900524 ) ) ;
#25467 = CARTESIAN_POINT ( 'NONE',  ( -1.815588850254800546, -23.89016120430182966, 43.60036197523994161 ) ) ;
#25468 = CARTESIAN_POINT ( 'NONE',  ( 1.564253033640336188, -44.28527310957331053, 24.39614062124470450 ) ) ;
#25469 = EDGE_LOOP ( 'NONE', ( #21073, #11687, #4030, #627 ) ) ;
#25470 = ORIENTED_EDGE ( 'NONE', *, *, #11900, .T. ) ;
#25471 = CARTESIAN_POINT ( 'NONE',  ( -197.6433718613163251, -44.74793361790577961, -18.53520099270188837 ) ) ;
#25472 = CARTESIAN_POINT ( 'NONE',  ( 91.82158438592156813, 40.00000000000009948, -17.20528682183286051 ) ) ;
#25473 = CARTESIAN_POINT ( 'NONE',  ( -99.31364972217929221, -20.48028939131244996, -8.933506367407366255 ) ) ;
#25474 = CONICAL_SURFACE ( 'NONE', #23733, 75.00000000000000000, 0.4944367829892072352 ) ;
#25475 =( BOUNDED_SURFACE ( )  B_SPLINE_SURFACE ( 3, 2, ( 
 ( #23434, #7315, #5210 ),
 ( #11434, #13314, #21434 ),
 ( #3207, #10107, #26091 ),
 ( #7827, #16223, #10239 ),
 ( #11967, #24485, #18208 ),
 ( #22489, #18479, #24214 ),
 ( #12357, #26232, #4269 ),
 ( #3864, #22091, #15946 ),
 ( #14224, #6369, #9581 ),
 ( #17945, #130, #22362 ),
 ( #24075, #20091, #12099 ),
 ( #14488, #8102, #9973 ),
 ( #20223, #6247, #11830 ),
 ( #14095, #3727, #18080 ),
 ( #20487, #1870, #7966 ),
 ( #12231, #2131, #260 ),
 ( #16085, #8234, #24352 ),
 ( #6116, #4139, #4000 ),
 ( #5986, #2261, #20356 ),
 ( #22224, #18350, #9841 ),
 ( #1999, #13957, #16352 ),
 ( #14360, #10368, #8368 ),
 ( #16491, #24616, #19948 ),
 ( #1732, #5851, #10502 ),
 ( #399, #20615, #6504 ),
 ( #12490, #24750, #2391 ),
 ( #18615, #8503, #22621 ),
 ( #4396, #16616, #9611 ),
 ( #23841, #25720, #3362 ),
 ( #17716, #7602, #9746 ),
 ( #17338, #7733, #1505 ),
 ( #19717, #25471, #7473 ),
 ( #25601, #7347, #15845 ),
 ( #15587, #15459, #11344 ) ),
 .UNSPECIFIED., .F., .F., .F. ) 
 B_SPLINE_SURFACE_WITH_KNOTS ( ( 4, 2, 2, 2, 2, 2, 2, 2, 2, 2, 2, 2, 2, 2, 2, 2, 4 ),
 ( 3, 3 ),
 ( 0.005135431517081588682, 0.02907016617530113270, 0.05300490083352067672, 0.07693963549174021033, 0.08292331915629509720, 0.08441924007243381545, 0.08446598760106314996, 0.08448936136537782415, 0.08451273512969248447, 0.08460623018695115349, 0.08479322030146849154, 0.08516720053050318151, 0.08591516098857254757, 0.08890700282084998407, 0.09189884465312742057, 0.09489068648540487094, 0.1008743701499597578 ),
 ( 0.000000000000000000, 1.000000000000000000 ),
 .UNSPECIFIED. ) 
 GEOMETRIC_REPRESENTATION_ITEM ( )  RATIONAL_B_SPLINE_SURFACE ( (
 ( 1.000000000000000000, 0.9997813423552077694, 1.000000000000000000),
 ( 1.000000000000000000, 0.9991063894446133853, 1.000000000000000000),
 ( 1.000000000000000000, 0.9968824679666075106, 1.000000000000000000),
 ( 1.000000000000000000, 0.9891556708435274015, 1.000000000000000000),
 ( 1.000000000000000000, 0.9836552227702378692, 1.000000000000000000),
 ( 1.000000000000000000, 0.9690804699600285010, 1.000000000000000000),
 ( 1.000000000000000000, 0.9600093828087571390, 1.000000000000000000),
 ( 1.000000000000000000, 0.9461484455229860480, 1.000000000000000000),
 ( 1.000000000000000000, 0.9432496483672391241, 1.000000000000000000),
 ( 1.000000000000000000, 0.9394619383806329660, 1.000000000000000000),
 ( 1.000000000000000000, 0.9386961831921698529, 1.000000000000000000),
 ( 1.000000000000000000, 0.9378979462694481128, 1.000000000000000000),
 ( 1.000000000000000000, 0.9378737491732476173, 1.000000000000000000),
 ( 1.000000000000000000, 0.9378374413774223095, 1.000000000000000000),
 ( 1.000000000000000000, 0.9378252326299115760, 1.000000000000000000),
 ( 1.000000000000000000, 0.9378013115143154499, 1.000000000000000000),
 ( 1.000000000000000000, 0.9377893564346068134, 1.000000000000000000),
 ( 1.000000000000000000, 0.9377296084626393080, 1.000000000000000000),
 ( 1.000000000000000000, 0.9376818978498918655, 1.000000000000000000),
 ( 1.000000000000000000, 0.9375390306864356260, 1.000000000000000000),
 ( 1.000000000000000000, 0.9374441388112084717, 1.000000000000000000),
 ( 1.000000000000000000, 0.9371605328928015455, 1.000000000000000000),
 ( 1.000000000000000000, 0.9369728885716435141, 1.000000000000000000),
 ( 1.000000000000000000, 0.9364143219790276307, 1.000000000000000000),
 ( 1.000000000000000000, 0.9360477663173705221, 1.000000000000000000),
 ( 1.000000000000000000, 0.9342452504720827333, 1.000000000000000000),
 ( 1.000000000000000000, 0.9329001521055318991, 1.000000000000000000),
 ( 1.000000000000000000, 0.9304320728630436355, 1.000000000000000000),
 ( 1.000000000000000000, 0.9293115496648971519, 1.000000000000000000),
 ( 1.000000000000000000, 0.9273349178231704570, 1.000000000000000000),
 ( 1.000000000000000000, 0.9264755994062942035, 1.000000000000000000),
 ( 1.000000000000000000, 0.9243018539387418686, 1.000000000000000000),
 ( 1.000000000000000000, 0.9233922906947681364, 1.000000000000000000),
 ( 1.000000000000000000, 0.9230540990195943429, 1.000000000000000000) ) ) 
 REPRESENTATION_ITEM ( '' )  SURFACE ( )  );
#25476 = PRODUCT_DEFINITION_CONTEXT ( 'detailed design', #11214, 'design' ) ;
#25477 = AXIS2_PLACEMENT_3D ( 'NONE', #1100, #979, #9210 ) ;
#25478 = CARTESIAN_POINT ( 'NONE',  ( -238.4067589809705794, 28.96627169325354956, -28.96627169325289231 ) ) ;
#25479 = CARTESIAN_POINT ( 'NONE',  ( 130.8568914410475088, -39.99999999999988631, -34.05028731879802706 ) ) ;
#25480 = CARTESIAN_POINT ( 'NONE',  ( 199.9999999999999147, -18.52330518485242195, -4.309840028370497400 ) ) ;
#25481 = CARTESIAN_POINT ( 'NONE',  ( -82.30220482034332008, 7.992411108785294260, 18.51665893431345111 ) ) ;
#25482 = CARTESIAN_POINT ( 'NONE',  ( -8.720657192082322595, -13.49580954685952072, -45.36528685024973129 ) ) ;
#25483 = CARTESIAN_POINT ( 'NONE',  ( 0.2972598230770048811, -10.13633138497415942, -66.70487387989865624 ) ) ;
#25484 = DIRECTION ( 'NONE',  ( 0.000000000000000000, 1.000000000000000000, 0.000000000000000000 ) ) ;
#25485 = CARTESIAN_POINT ( 'NONE',  ( -135.8532207217289738, 3.005970985514575011E-13, -30.84685318188645553 ) ) ;
#25486 = DIRECTION ( 'NONE',  ( 0.7071067811865500152, 0.000000000000000000, -0.7071067811865451302 ) ) ;
#25487 = CARTESIAN_POINT ( 'NONE',  ( -238.4067589809705794, -0.9644942799826263791, -40.00000000000002132 ) ) ;
#25488 = CARTESIAN_POINT ( 'NONE',  ( 163.1118516004056573, 19.27778845539212327, 37.29075403953164169 ) ) ;
#25489 = CARTESIAN_POINT ( 'NONE',  ( 184.8905102610680444, 20.92133201514447194, -40.00000000000002132 ) ) ;
#25491 = CARTESIAN_POINT ( 'NONE',  ( 192.4448373802101173, 40.00000000000012790, -20.00000000003928236 ) ) ;
#25490 = CARTESIAN_POINT ( 'NONE',  ( -2.652172544013597033, -43.38951316025622162, -23.73409167602006420 ) ) ;
#25492 = CARTESIAN_POINT ( 'NONE',  ( -198.0356074513804572, 1.247057299367198800E-13, -15.37879056873070560 ) ) ;
#25493 = CARTESIAN_POINT ( 'NONE',  ( -192.9588430854690273, 66.79921049721887982, 10.23066800229522677 ) ) ;
#25494 = CARTESIAN_POINT ( 'NONE',  ( 136.1360204305621266, 4.966164525587089429, 2.449293598294708485E-15 ) ) ;
#25495 = ORIENTED_EDGE ( 'NONE', *, *, #20796, .T. ) ;
#25496 = CIRCLE ( 'NONE', #6794, 30.00000000000000355 ) ;
#25497 = CARTESIAN_POINT ( 'NONE',  ( 22.57783252600012247, -43.22748647439753711, 17.90541116499475649 ) ) ;
#25498 = EDGE_CURVE ( 'NONE', #7784, #25916, #7226, .T. ) ;
#25499 = CARTESIAN_POINT ( 'NONE',  ( 0.000000000000000000, 5.510910596163085611E-15, 44.99999999999997158 ) ) ;
#25500 = CARTESIAN_POINT ( 'NONE',  ( -198.0356074513804572, 10.87444709758468875, 67.44298959250869530 ) ) ;
#25501 = CARTESIAN_POINT ( 'NONE',  ( 19.06497207195981147, -4.605042221739098431E-14, 14.19242893257840521 ) ) ;
#25502 = DIRECTION ( 'NONE',  ( 0.000000000000000000, 0.000000000000000000, -1.000000000000000000 ) ) ;
#25503 = VECTOR ( 'NONE', #11194, 1000.000000000000000 ) ;
#25504 = CARTESIAN_POINT ( 'NONE',  ( 22.82385994800818452, -13.83113328680564358, -47.01156385802205762 ) ) ;
#25505 = CARTESIAN_POINT ( 'NONE',  ( 199.9999999999999147, 6.094537134382843391, 18.00666549647224812 ) ) ;
#25506 = CARTESIAN_POINT ( 'NONE',  ( -655.4136578433802924, 38.83551722856093136, -9.594100677173759806 ) ) ;
#25507 = ADVANCED_FACE ( 'NONE', ( #17199 ), #2570, .T. ) ;
#25508 = CARTESIAN_POINT ( 'NONE',  ( -82.26674357280019478, -5.016125564933051173, -19.55222226025773935 ) ) ;
#25509 = CARTESIAN_POINT ( 'NONE',  ( 151.7948205124836250, -33.23291073765550863, 0.000000000000000000 ) ) ;
#25510 = CARTESIAN_POINT ( 'NONE',  ( 4.995406935893287326, 17.50105314357225694, -39.06748935135176026 ) ) ;
#25511 = AXIS2_PLACEMENT_3D ( 'NONE', #6431, #4721, #12957 ) ;
#25512 = EDGE_CURVE ( 'NONE', #12615, #4688, #5123, .T. ) ;
#25513 = CARTESIAN_POINT ( 'NONE',  ( 184.8905102610680444, 14.79361573936366092, 41.77492675556006674 ) ) ;
#25514 = FACE_OUTER_BOUND ( 'NONE', #25559, .T. ) ;
#25515 = CARTESIAN_POINT ( 'NONE',  ( -30.26275506840322649, -29.48230279907769358, -29.48230279907820162 ) ) ;
#25517 = CARTESIAN_POINT ( 'NONE',  ( -213.1075012329537230, 9.698598906450543566, -9.698598906450348167 ) ) ;
#25516 = CARTESIAN_POINT ( 'NONE',  ( 200.0000000000000000, 14.14213562373142352, -42.42640687119268961 ) ) ;
#25518 = CARTESIAN_POINT ( 'NONE',  ( 146.6084372240433993, 3.800685668858732935, -3.800685668858610367 ) ) ;
#25519 = CARTESIAN_POINT ( 'NONE',  ( -91.56559293963834989, -22.67402823373193499, 0.000000000000000000 ) ) ;
#25520 = FACE_OUTER_BOUND ( 'NONE', #16210, .T. ) ;
#25521 = DIRECTION ( 'NONE',  ( 1.000000000000000000, 1.836970198721030427E-16, -0.000000000000000000 ) ) ;
#25522 = CARTESIAN_POINT ( 'NONE',  ( 136.1360204305621266, -3.511608612531119000, 53.05693388239312469 ) ) ;
#25523 = CARTESIAN_POINT ( 'NONE',  ( -188.8842190493874966, 43.30124183641388669, -17.93596163623950446 ) ) ;
#25524 = ORIENTED_EDGE ( 'NONE', *, *, #10438, .F. ) ;
#25525 = CARTESIAN_POINT ( 'NONE',  ( 192.4448373802101173, 42.42640687116508502, -14.14213562375874567 ) ) ;
#25526 = CARTESIAN_POINT ( 'NONE',  ( -82.26522933719705577, -17.41047943211789217, -10.29035321569880246 ) ) ;
#25527 = CARTESIAN_POINT ( 'NONE',  ( 37.15749683964845218, 20.52531616279084759, 38.58455518508856841 ) ) ;
#25528 = FACE_OUTER_BOUND ( 'NONE', #1118, .T. ) ;
#25529 = VERTEX_POINT ( 'NONE', #5111 ) ;
#25530 = CARTESIAN_POINT ( 'NONE',  ( -188.8531444083262159, -43.29283928523321379, 17.93248118558238602 ) ) ;
#25531 = VECTOR ( 'NONE', #4490, 1000.000000000000000 ) ;
#25532 = CARTESIAN_POINT ( 'NONE',  ( 200.0000000000000284, -15.36457271445731543, -11.18861246136148502 ) ) ;
#25533 = CARTESIAN_POINT ( 'NONE',  ( 22.81400246987424651, -17.87890238636459728, 43.16348862150608312 ) ) ;
#25534 = CARTESIAN_POINT ( 'NONE',  ( -114.4098922876147384, 20.15198150140922451, 8.347224046571190215 ) ) ;
#25535 = CARTESIAN_POINT ( 'NONE',  ( 199.0076473327615645, 2.278485796641462446, -19.86629856447459375 ) ) ;
#25536 = CYLINDRICAL_SURFACE ( 'NONE', #23637, 5.000000000000018652 ) ;
#25537 = CARTESIAN_POINT ( 'NONE',  ( -198.0356074513804572, 39.99999999999992895, 15.37879056873084771 ) ) ;
#25538 = DIRECTION ( 'NONE',  ( 0.000000000000000000, 0.000000000000000000, -1.000000000000000000 ) ) ;
#25539 = CARTESIAN_POINT ( 'NONE',  ( -200.0000000000000000, -17.28402242884604334, -46.84854965773187274 ) ) ;
#25540 = CARTESIAN_POINT ( 'NONE',  ( -100.7734535825088500, -17.32597176626812185, -40.00000000000002132 ) ) ;
#25542 = CARTESIAN_POINT ( 'NONE',  ( -608.6692201736730112, 32.15154313405594877, -23.83432366117598633 ) ) ;
#25541 = FACE_OUTER_BOUND ( 'NONE', #5541, .T. ) ;
#25543 = CARTESIAN_POINT ( 'NONE',  ( 0.2972598230770129857, -54.33493731733938148, 40.00000000000002132 ) ) ;
#25544 = CARTESIAN_POINT ( 'NONE',  ( -208.1127848780265026, -15.00245453012673202, 0.000000000000000000 ) ) ;
#25545 = VECTOR ( 'NONE', #9121, 999.9999999999998863 ) ;
#25546 = AXIS2_PLACEMENT_3D ( 'NONE', #584, #4843, #451 ) ;
#25547 = CARTESIAN_POINT ( 'NONE',  ( -259.2033419157646676, 40.00000000000029843, -30.48217210827696988 ) ) ;
#25548 = CONICAL_SURFACE ( 'NONE', #14059, 21.53474504356810115, 0.7853981633974378429 ) ;
#25549 = CARTESIAN_POINT ( 'NONE',  ( -280.0000000000000568, -40.00000000000028422, 19.99999999999959499 ) ) ;
#25550 = CARTESIAN_POINT ( 'NONE',  ( 190.0000000000000000, -66.50000000000001421, 66.50000000000005684 ) ) ;
#25551 = ORIENTED_EDGE ( 'NONE', *, *, #13952, .F. ) ;
#25553 = CARTESIAN_POINT ( 'NONE',  ( -4.027137536849644484, 46.99492183298354320, -13.82877337592798384 ) ) ;
#25552 = CARTESIAN_POINT ( 'NONE',  ( -87.11162894489403641, 21.34897934681861287, -2.713946817477653095 ) ) ;
#25554 = CARTESIAN_POINT ( 'NONE',  ( -91.56559293963836410, 22.67402823373190301, 40.00000000000002132 ) ) ;
#25555 = EDGE_CURVE ( 'NONE', #7172, #6927, #11843, .T. ) ;
#25556 = CARTESIAN_POINT ( 'NONE',  ( -188.4701769959647777, 47.05181236278308177, -13.83721050406937358 ) ) ;
#25557 = DIRECTION ( 'NONE',  ( 1.000000000000000000, 0.000000000000000000, 0.000000000000000000 ) ) ;
#25558 = ORIENTED_EDGE ( 'NONE', *, *, #6062, .F. ) ;
#25559 = EDGE_LOOP ( 'NONE', ( #17768, #5141 ) ) ;
#25560 = AXIS2_PLACEMENT_3D ( 'NONE', #12993, #23241, #18984 ) ;
#25561 = CARTESIAN_POINT ( 'NONE',  ( 14.38125909742181285, -10.73282306404727393, 10.73282306404716380 ) ) ;
#25562 = CARTESIAN_POINT ( 'NONE',  ( 130.8888609958233928, 12.21841679119731516, -29.49786752803534284 ) ) ;
#25563 = CARTESIAN_POINT ( 'NONE',  ( -105.4741150117382062, 7.943527260750565588, -19.77569912955109288 ) ) ;
#25564 = ORIENTED_EDGE ( 'NONE', *, *, #2485, .F. ) ;
#25565 = CARTESIAN_POINT ( 'NONE',  ( 199.0262887415137527, -15.87643591937917442, 12.17243215972436055 ) ) ;
#25566 = CIRCLE ( 'NONE', #5165, 5.000000000000004441 ) ;
#25567 = DIRECTION ( 'NONE',  ( 0.01051738792034601078, 0.9307051272717529189, 0.3656191332813465977 ) ) ;
#25568 = CARTESIAN_POINT ( 'NONE',  ( -238.4067589809705794, 57.25054294077225592, 0.6820004458485544596 ) ) ;
#25569 = AXIS2_PLACEMENT_3D ( 'NONE', #14931, #10688, #446 ) ;
#25570 = CARTESIAN_POINT ( 'NONE',  ( -192.9588430854689989, -8.596193650988133061E-14, 14.46834944099969533 ) ) ;
#25571 = CYLINDRICAL_SURFACE ( 'NONE', #22368, 5.000000000000004441 ) ;
#25572 = DIRECTION ( 'NONE',  ( 0.000000000000000000, 1.000000000000000000, 0.000000000000000000 ) ) ;
#25573 = CARTESIAN_POINT ( 'NONE',  ( -4.039451493210497901, 23.44932283416708074, -43.00522595893983890 ) ) ;
#25574 = CARTESIAN_POINT ( 'NONE',  ( -213.1075012329537230, -39.99999999999991473, -13.71589010951953647 ) ) ;
#25575 = CARTESIAN_POINT ( 'NONE',  ( 136.1360204305621266, 7.947488714877270288E-14, -4.966164525587064560 ) ) ;
#25576 = CARTESIAN_POINT ( 'NONE',  ( -82.30777374956703341, 18.64665802842208819, 7.678022728832912591 ) ) ;
#25577 = CARTESIAN_POINT ( 'NONE',  ( -100.7734535825088500, -12.25131212657462498, -44.31723036834905827 ) ) ;
#25578 = CARTESIAN_POINT ( 'NONE',  ( 146.6084372240433993, 1.478241399363601114E-13, -34.62501878078305850 ) ) ;
#25579 = CARTESIAN_POINT ( 'NONE',  ( -162.0762913951020892, -1.198031840385783919, 1.198031840385741731 ) ) ;
#25580 = CARTESIAN_POINT ( 'NONE',  ( 154.0339099654742370, 28.18615453125279657, 11.67508747798898661 ) ) ;
#25581 = CARTESIAN_POINT ( 'NONE',  ( -210.0000000000000284, 60.27431767988564104, -73.32453023895048716 ) ) ;
#25582 = CARTESIAN_POINT ( 'NONE',  ( 184.8905102610680444, 43.07788698682572459, 13.49065550809829439 ) ) ;
#25583 = CARTESIAN_POINT ( 'NONE',  ( -86.95438060917874168, -9.637778285156878511, 19.12135828302521290 ) ) ;
#25584 = CARTESIAN_POINT ( 'NONE',  ( -238.4067589809705794, 0.6820004457340470561, 57.25054294065803617 ) ) ;
#25585 = AXIS2_PLACEMENT_3D ( 'NONE', #3332, #15427, #19430 ) ;
#25586 = CARTESIAN_POINT ( 'NONE',  ( -192.9588430854690273, -38.51493924976957572, 18.05360324515410397 ) ) ;
#25587 = CARTESIAN_POINT ( 'NONE',  ( -657.0499062528585910, 41.27686082678435042, -17.95486116563373002 ) ) ;
#25588 = CARTESIAN_POINT ( 'NONE',  ( -4.039451493210496125, 23.44932283416649454, 43.00522595894017286 ) ) ;
#25589 = ORIENTED_EDGE ( 'NONE', *, *, #3142, .F. ) ;
#25590 = CARTESIAN_POINT ( 'NONE',  ( -105.3755690713226727, 12.89780903124418998, -12.89780903124389155 ) ) ;
#25591 = DIRECTION ( 'NONE',  ( -4.657398277317546459E-32, 1.682156097916904081E-16, 1.000000000000000000 ) ) ;
#25592 = EDGE_CURVE ( 'NONE', #17844, #15971, #6365, .T. ) ;
#25593 = DIRECTION ( 'NONE',  ( 1.000000000000000000, -0.000000000000000000, -0.000000000000000000 ) ) ;
#25594 = EDGE_LOOP ( 'NONE', ( #8262, #18813, #6400, #21804 ) ) ;
#25595 = CARTESIAN_POINT ( 'NONE',  ( -198.0356074513804572, 1.247057299367198800E-13, -15.37879056873070560 ) ) ;
#25596 = CARTESIAN_POINT ( 'NONE',  ( 199.0189539020448990, -17.60163767500414522, -9.515575210798317585 ) ) ;
#25597 = EDGE_CURVE ( 'NONE', #12394, #11522, #15645, .T. ) ;
#25598 = CARTESIAN_POINT ( 'NONE',  ( -16.41594856527310142, 21.03672846649599748, 39.35878123536664219 ) ) ;
#25599 = EDGE_LOOP ( 'NONE', ( #12833, #2867, #20645, #5194 ) ) ;
#25600 = ORIENTED_EDGE ( 'NONE', *, *, #12384, .T. ) ;
#25601 = CARTESIAN_POINT ( 'NONE',  ( -198.9233928135190581, -44.84148042516751786, -24.80620717268675790 ) ) ;
#25602 = CARTESIAN_POINT ( 'NONE',  ( 57.59792236341147031, 39.99999999999990763, 37.56421063658199699 ) ) ;
#25603 = EDGE_CURVE ( 'NONE', #23960, #8098, #4892, .T. ) ;
#25604 = ADVANCED_FACE ( 'NONE', ( #26115 ), #9866, .T. ) ;
#25605 = CARTESIAN_POINT ( 'NONE',  ( -94.58360650938176661, -20.58386743652064510, -9.000712009641768319 ) ) ;
#25606 = AXIS2_PLACEMENT_3D ( 'NONE', #23835, #3236, #11093 ) ;
#25607 = CARTESIAN_POINT ( 'NONE',  ( 163.1118516004056573, 9.006482792069759213, -9.006482792069505194 ) ) ;
#25608 = CARTESIAN_POINT ( 'NONE',  ( -100.7734535825088358, -8.145438380286941744E-14, 17.32597176626811120 ) ) ;
#25609 = CARTESIAN_POINT ( 'NONE',  ( 200.0000000000000568, -16.61842928396364272, -9.229186156037545885 ) ) ;
#25610 = CYLINDRICAL_SURFACE ( 'NONE', #10066, 4.999999999999997335 ) ;
#25611 = CARTESIAN_POINT ( 'NONE',  ( -162.0762913951020892, 1.198031840385732849, -1.198031840385733515 ) ) ;
#25612 = CARTESIAN_POINT ( 'NONE',  ( 19.06497207195980792, 18.24870850772790831, -38.31983398719609824 ) ) ;
#25613 = CARTESIAN_POINT ( 'NONE',  ( -86.91014751117384662, -19.35827336066798665, 9.009177718430992243 ) ) ;
#25614 = CARTESIAN_POINT ( 'NONE',  ( 192.4448373802100889, 2.472897170449861688E-13, -19.99999999996060751 ) ) ;
#25615 = CARTESIAN_POINT ( 'NONE',  ( 170.0000000000000284, -22.62041470344884431, 9.369682556672202622 ) ) ;
#25616 = CARTESIAN_POINT ( 'NONE',  ( -192.9588430854690273, -14.46834944099973264, 40.00000000000002132 ) ) ;
#25617 = CARTESIAN_POINT ( 'NONE',  ( 192.4448373802101173, -19.99999999996056843, -40.00000000000002132 ) ) ;
#25618 = CARTESIAN_POINT ( 'NONE',  ( -91.56559293963836410, 16.03295912088714203, -16.03295912088699282 ) ) ;
#25619 = CARTESIAN_POINT ( 'NONE',  ( -100.7734535825088500, 22.67402823373189946, -40.00000000000002132 ) ) ;
#25621 = CARTESIAN_POINT ( 'NONE',  ( -190.0000000000000000, -61.50000000000001421, -66.50000000000005684 ) ) ;
#25620 = CARTESIAN_POINT ( 'NONE',  ( 1.564570055219380640, -44.28524390194900207, -24.39611894128482916 ) ) ;
#25622 = DIRECTION ( 'NONE',  ( -1.000000000000000000, -1.836970198721030181E-16, 0.000000000000000000 ) ) ;
#25623 = CARTESIAN_POINT ( 'NONE',  ( 0.2972598230769959993, 38.42060263243659080, 38.42060263243672580 ) ) ;
#25624 = CARTESIAN_POINT ( 'NONE',  ( 4.995406935893289102, 55.24977328856464709, -40.00000000000002132 ) ) ;
#25625 = EDGE_LOOP ( 'NONE', ( #7731, #383 ) ) ;
#25626 =( BOUNDED_SURFACE ( )  B_SPLINE_SURFACE ( 3, 2, ( 
 ( #5226, #9214, #25459 ),
 ( #21577, #3351, #21332 ),
 ( #11084, #9594, #17571 ),
 ( #15325, #11451, #5478 ),
 ( #3483, #11207, #3227 ),
 ( #17699, #9087, #11580 ),
 ( #13087, #1235, #19700 ),
 ( #1488, #25843, #7587 ),
 ( #4980, #9340, #982 ),
 ( #19322, #1106, #7210 ),
 ( #23452, #25977, #18101 ),
 ( #6134, #19970, #24371 ),
 ( #21837, #7985, #2024 ),
 ( #12119, #21972, #13712 ),
 ( #5733, #24235, #12253 ),
 ( #22109, #23958, #5869 ),
 ( #6008, #14117, #17830 ),
 ( #1751, #10260, #13838 ),
 ( #14242, #13975, #18370 ),
 ( #26109, #20244, #4158 ),
 ( #9991, #20375, #11986 ),
 ( #3744, #10126, #3885 ),
 ( #26250, #20109, #24094 ),
 ( #17962, #22382, #16103 ),
 ( #11849, #18227, #3606 ),
 ( #14, #2150, #7848 ),
 ( #22244, #1886, #9860 ),
 ( #15969, #4019, #8125 ),
 ( #16242, #149, #8253 ),
 ( #23823, #5606, #19835 ),
 ( #11716, #1621, #7718 ),
 ( #9728, #15828, #26117 ),
 ( #4297, #24105, #20117 ),
 ( #7856, #3752, #22390 ) ),
 .UNSPECIFIED., .F., .F., .T. ) 
 B_SPLINE_SURFACE_WITH_KNOTS ( ( 4, 2, 2, 2, 2, 2, 2, 2, 2, 2, 2, 2, 2, 2, 2, 2, 4 ),
 ( 3, 3 ),
 ( 0.005135431517081092551, 0.02907016617530085861, 0.05300490083352062815, 0.07693963549174039074, 0.08292331915629533312, 0.08441924007243406525, 0.08446598760106339976, 0.08448936136537807395, 0.08451273512969273427, 0.08460623018695140329, 0.08479322030146874134, 0.08516720053050343131, 0.08591516098857279737, 0.08890700282085027550, 0.09189884465312775363, 0.09489068648540521789, 0.1008743701499601603 ),
 ( 0.000000000000000000, 1.000000000000000000 ),
 .UNSPECIFIED. ) 
 GEOMETRIC_REPRESENTATION_ITEM ( )  RATIONAL_B_SPLINE_SURFACE ( (
 ( 1.000000000000000000, 0.9997813423552077694, 1.000000000000000000),
 ( 1.000000000000000000, 0.9991063894442805404, 1.000000000000000000),
 ( 1.000000000000000000, 0.9968824679670508226, 1.000000000000000000),
 ( 1.000000000000000000, 0.9891556708430847555, 1.000000000000000000),
 ( 1.000000000000000000, 0.9836552227706814033, 1.000000000000000000),
 ( 1.000000000000000000, 0.9690804699595860772, 1.000000000000000000),
 ( 1.000000000000000000, 0.9600093828096437631, 1.000000000000000000),
 ( 1.000000000000000000, 0.9461484455227653356, 1.000000000000000000),
 ( 1.000000000000000000, 0.9432496483672401233, 1.000000000000000000),
 ( 1.000000000000000000, 0.9394619383806339652, 1.000000000000000000),
 ( 1.000000000000000000, 0.9386961831920875854, 1.000000000000000000),
 ( 1.000000000000000000, 0.9378979462694514435, 1.000000000000000000),
 ( 1.000000000000000000, 0.9378737491732502818, 1.000000000000000000),
 ( 1.000000000000000000, 0.9378374413774224205, 1.000000000000000000),
 ( 1.000000000000000000, 0.9378252326299112429, 1.000000000000000000),
 ( 1.000000000000000000, 0.9378013115143177814, 1.000000000000000000),
 ( 1.000000000000000000, 0.9377893564346067024, 1.000000000000000000),
 ( 1.000000000000000000, 0.9377296084626435269, 1.000000000000000000),
 ( 1.000000000000000000, 0.9376818978498911994, 1.000000000000000000),
 ( 1.000000000000000000, 0.9375390306864400669, 1.000000000000000000),
 ( 1.000000000000000000, 0.9374441388111988127, 1.000000000000000000),
 ( 1.000000000000000000, 0.9371605328928230838, 1.000000000000000000),
 ( 1.000000000000000000, 0.9369728885716236411, 1.000000000000000000),
 ( 1.000000000000000000, 0.9364143219790700412, 1.000000000000000000),
 ( 1.000000000000000000, 0.9360477663173711882, 1.000000000000000000),
 ( 1.000000000000000000, 0.9342452504720832884, 1.000000000000000000),
 ( 1.000000000000000000, 0.9329001521054770540, 1.000000000000000000),
 ( 1.000000000000000000, 0.9304320728630998127, 1.000000000000000000),
 ( 1.000000000000000000, 0.9293115496652294416, 1.000000000000000000),
 ( 1.000000000000000000, 0.9273349178228399436, 1.000000000000000000),
 ( 1.000000000000000000, 0.9264755994061858457, 1.000000000000000000),
 ( 1.000000000000000000, 0.9243018539389626920, 1.000000000000000000),
 ( 1.000000000000000000, 0.9233922906946046005, 1.000000000000000000),
 ( 1.000000000000000000, 0.9230540990195957862, 1.000000000000000000) ) ) 
 REPRESENTATION_ITEM ( '' )  SURFACE ( )  );
#25627 = CARTESIAN_POINT ( 'NONE',  ( 23.36462152323065311, -46.81175967489662071, 13.80148662728995568 ) ) ;
#25628 = FACE_OUTER_BOUND ( 'NONE', #2120, .T. ) ;
#25629 = CARTESIAN_POINT ( 'NONE',  ( -91.56559293963834989, 12.25131212657480440, 12.25131212657486834 ) ) ;
#25630 = CYLINDRICAL_SURFACE ( 'NONE', #24180, 30.00000000000004974 ) ;
#25631 = CARTESIAN_POINT ( 'NONE',  ( -87.01809839470989516, 20.74596926290789156, -5.316578559416913485 ) ) ;
#25632 = CARTESIAN_POINT ( 'NONE',  ( -16.87994666115289988, 12.91133298909479166, -42.52193590819778279 ) ) ;
#25633 = CARTESIAN_POINT ( 'NONE',  ( 200.0000000000005684, -1.253076495463282924, 18.97792690268338234 ) ) ;
#25634 = DIRECTION ( 'NONE',  ( 1.000000000000000000, 1.836970198721030181E-16, 0.000000000000000000 ) ) ;
#25635 = CARTESIAN_POINT ( 'NONE',  ( -86.99952317291963766, -5.713267018748582338, -20.62702873475882370 ) ) ;
#25636 = CARTESIAN_POINT ( 'NONE',  ( -91.56559293963834989, -16.03295912088728414, 16.03295912088688269 ) ) ;
#25637 = CARTESIAN_POINT ( 'NONE',  ( 146.6084372240433709, 24.48358557860356655, -32.08495691632035118 ) ) ;
#25638 = CARTESIAN_POINT ( 'NONE',  ( -105.2105218841390126, 21.45999192170251035, -1.182031380070910798 ) ) ;
#25639 = CARTESIAN_POINT ( 'NONE',  ( -200.0000000000000000, -52.49999999999972289, -82.49999999999998579 ) ) ;
#25640 = CARTESIAN_POINT ( 'NONE',  ( 57.59792236341148453, 1.722363176415528940, -54.84617931850878136 ) ) ;
#25642 = CARTESIAN_POINT ( 'NONE',  ( 57.59792236341147031, -30.00663442387662627, -26.56190807104723461 ) ) ;
#25641 = CARTESIAN_POINT ( 'NONE',  ( -135.8532207217289738, -21.81201906317757633, -21.81201906317793515 ) ) ;
#25643 = CARTESIAN_POINT ( 'NONE',  ( 0.2972598230769907257, 66.70487387989869887, -10.13633138497392494 ) ) ;
#25644 = CARTESIAN_POINT ( 'NONE',  ( -105.3220005116046849, -10.86457728905244124, 18.46446237100853338 ) ) ;
#25645 = DIRECTION ( 'NONE',  ( 1.000000000000000000, -0.000000000000000000, -0.000000000000000000 ) ) ;
#25646 = CARTESIAN_POINT ( 'NONE',  ( 0.2972598230770030492, -40.00000000000007816, 14.33493731733919496 ) ) ;
#25647 = CARTESIAN_POINT ( 'NONE',  ( -259.2033419157646676, -49.83842185052040463, 6.730120644403092101 ) ) ;
#25648 = CARTESIAN_POINT ( 'NONE',  ( 136.1360204305621551, 4.966164525587085876, 40.00000000000002132 ) ) ;
#25649 = ORIENTED_EDGE ( 'NONE', *, *, #13075, .F. ) ;
#25650 = CARTESIAN_POINT ( 'NONE',  ( 151.7948205124836534, 4.785054706298574878, -51.78348778862537927 ) ) ;
#25651 = CARTESIAN_POINT ( 'NONE',  ( -2.717871546781097880, 42.53710973099089188, 17.61944775472897717 ) ) ;
#25652 = LINE ( 'NONE', #7398, #12405 ) ;
#25653 = CARTESIAN_POINT ( 'NONE',  ( -5.859158571313241026, -42.46836465824206641, -23.09435402966316175 ) ) ;
#25654 = ORIENTED_EDGE ( 'NONE', *, *, #7013, .T. ) ;
#25655 = CARTESIAN_POINT ( 'NONE',  ( -105.2113312088911385, 16.16375985776740620, 14.17769269060415738 ) ) ;
#25656 = B_SPLINE_CURVE_WITH_KNOTS ( 'NONE', 3,
 ( #11769, #16559, #24419, #18557, #12431, #12174, #22826, #10440 ),
 .UNSPECIFIED., .F., .F.,
 ( 4, 2, 2, 4 ),
 ( 0.008471746897510642679, 0.01052245438202778841, 0.01257316186654493587, 0.01667457683557922732 ),
 .UNSPECIFIED. ) ;
#25657 = CARTESIAN_POINT ( 'NONE',  ( 199.9999999999999432, -9.907006709245502307, -16.21817530592209522 ) ) ;
#25658 = CARTESIAN_POINT ( 'NONE',  ( 90.71511022962279469, -9.285713562939564625, 21.07400258644036484 ) ) ;
#25659 = DIRECTION ( 'NONE',  ( 0.000000000000000000, 0.000000000000000000, 1.000000000000000000 ) ) ;
#25660 = CARTESIAN_POINT ( 'NONE',  ( 199.0066734863077897, 5.484006884120094405, -19.23138624862535195 ) ) ;
#25661 = CARTESIAN_POINT ( 'NONE',  ( -626.9846540392142060, 95.00000000000000000, -34.99999999999999289 ) ) ;
#25662 = CARTESIAN_POINT ( 'NONE',  ( -30.26275506840325136, 40.00000000000001421, 1.694272468446399227 ) ) ;
#25663 = CARTESIAN_POINT ( 'NONE',  ( -77.58456292359235817, -2.764817855541193747, 21.97699700613614837 ) ) ;
#25664 = FACE_OUTER_BOUND ( 'NONE', #1531, .T. ) ;
#25665 = CARTESIAN_POINT ( 'NONE',  ( 170.2234770963711128, -15.44714144992812876, -2.449293598294708485E-15 ) ) ;
#25667 = CARTESIAN_POINT ( 'NONE',  ( -613.5029046138316744, 29.69186907203735259, -26.80434989160759329 ) ) ;
#25666 = CARTESIAN_POINT ( 'NONE',  ( -114.4364955367313996, 8.064892380834940866, -20.29001642039080622 ) ) ;
#25668 = CARTESIAN_POINT ( 'NONE',  ( 200.0000000000000000, -19.99999999999989342, 40.00000000000002132 ) ) ;
#25669 = CARTESIAN_POINT ( 'NONE',  ( -56.48582580120559982, 34.75652343174597547, 21.81201906317791384 ) ) ;
#25670 = CARTESIAN_POINT ( 'NONE',  ( -213.1075012329537230, 13.71589010951907817, 40.00000000000002132 ) ) ;
#25671 = CARTESIAN_POINT ( 'NONE',  ( 192.4448373802101173, 39.99999999999985079, 20.00000000003984013 ) ) ;
#25672 = CARTESIAN_POINT ( 'NONE',  ( -135.8532207217289738, -39.99999999999972289, -30.84685318188688541 ) ) ;
#25673 = FACE_OUTER_BOUND ( 'NONE', #7692, .T. ) ;
#25674 = VERTEX_POINT ( 'NONE', #8131 ) ;
#25676 = CARTESIAN_POINT ( 'NONE',  ( 8.209392600928651973, 49.31072049265984703, -14.17653494425351290 ) ) ;
#25675 = FACE_OUTER_BOUND ( 'NONE', #24281, .T. ) ;
#25677 = CARTESIAN_POINT ( 'NONE',  ( 4.995406935893309530, -55.24977328856464709, 40.00000000000002132 ) ) ;
#25678 = CARTESIAN_POINT ( 'NONE',  ( -30.26275506840324070, 1.198031551616030033, -1.198031551616006496 ) ) ;
#25679 = CARTESIAN_POINT ( 'NONE',  ( -188.9266304146017887, 43.31220791188989239, -17.94050393342734040 ) ) ;
#25680 = CARTESIAN_POINT ( 'NONE',  ( -526.9846540392140923, 0.000000000000000000, 0.000000000000000000 ) ) ;
#25681 = ORIENTED_EDGE ( 'NONE', *, *, #12092, .T. ) ;
#25682 = ORIENTED_EDGE ( 'NONE', *, *, #6869, .F. ) ;
#25683 = CARTESIAN_POINT ( 'NONE',  ( -88.39148973765254880, -19.92926839984449217, 8.577159256668625886 ) ) ;
#25684 = CARTESIAN_POINT ( 'NONE',  ( 141.7948666911895259, 12.58737617328916158, -30.38861427224623668 ) ) ;
#25685 = ORIENTED_EDGE ( 'NONE', *, *, #26060, .F. ) ;
#25686 = CARTESIAN_POINT ( 'NONE',  ( -162.0762913951021176, 57.76657433523994456, -1.198031840315424867 ) ) ;
#25687 = EDGE_LOOP ( 'NONE', ( #8200, #19709, #10102, #10276 ) ) ;
#25688 = CARTESIAN_POINT ( 'NONE',  ( 199.9999999999998010, -6.124229907523811356, 17.99904841416608292 ) ) ;
#25689 = CARTESIAN_POINT ( 'NONE',  ( -200.0000000000000000, -52.49999999999991473, 82.49999999999998579 ) ) ;
#25690 = CARTESIAN_POINT ( 'NONE',  ( 163.1118516004056573, 37.29075403953160617, -19.27778845539222985 ) ) ;
#25691 = CYLINDRICAL_SURFACE ( 'NONE', #12717, 69.99999999999995737 ) ;
#25692 = CARTESIAN_POINT ( 'NONE',  ( 0.2972598230769957217, -4.999556039334937811E-14, 14.33493731733933352 ) ) ;
#25693 = CARTESIAN_POINT ( 'NONE',  ( -105.2054292635175869, -15.19799821370180126, -15.19799821370278892 ) ) ;
#25694 = LINE ( 'NONE', #1348, #10446 ) ;
#25695 = CARTESIAN_POINT ( 'NONE',  ( -16.41582555379474684, 21.03675245593366583, -39.35881747758678983 ) ) ;
#25696 = CARTESIAN_POINT ( 'NONE',  ( 98.29820294270304259, -18.47759065022024672, 7.653668647299475047 ) ) ;
#25697 = CARTESIAN_POINT ( 'NONE',  ( -280.0000000000000000, 1.605030083646939673E-13, -20.00000000000001421 ) ) ;
#25698 = CARTESIAN_POINT ( 'NONE',  ( -110.0368417077422691, -7.992411109419241377, 18.51665893311217559 ) ) ;
#25699 = CARTESIAN_POINT ( 'NONE',  ( 163.1118516004056573, 19.27778845538780317, -19.27778845538757224 ) ) ;
#25700 = CARTESIAN_POINT ( 'NONE',  ( 180.0000000000000000, -71.50000000000002842, 66.50000000000005684 ) ) ;
#25701 = CARTESIAN_POINT ( 'NONE',  ( -199.9999999999998863, -44.86878812508856385, -24.82633483071075986 ) ) ;
#25702 = CARTESIAN_POINT ( 'NONE',  ( 169.9999999999999432, 22.62041470344884075, 9.369682556672378482 ) ) ;
#25703 = FACE_OUTER_BOUND ( 'NONE', #3957, .T. ) ;
#25704 = CARTESIAN_POINT ( 'NONE',  ( 192.4448373802101173, 42.42640687122070631, 14.14213562370331623 ) ) ;
#25705 = CARTESIAN_POINT ( 'NONE',  ( -238.4067589809705794, -40.00000000000007105, 0.9644942799824426372 ) ) ;
#25706 = CARTESIAN_POINT ( 'NONE',  ( -56.48582580120559982, -6.472252184284282173, 50.09629031063965243 ) ) ;
#25707 = CARTESIAN_POINT ( 'NONE',  ( 146.6084372240433993, -3.800685668858596156, -3.800685668858692967 ) ) ;
#25708 = CARTESIAN_POINT ( 'NONE',  ( -661.4804418431098156, 44.60892237560697993, -5.950252532928291593 ) ) ;
#25709 = DIRECTION ( 'NONE',  ( 1.000000000000000000, 1.836970198721030181E-16, 0.000000000000000000 ) ) ;
#25710 = ORIENTED_EDGE ( 'NONE', *, *, #8923, .F. ) ;
#25711 = CARTESIAN_POINT ( 'NONE',  ( 91.82158438592158234, -12.16597498399995203, -44.40256751092347542 ) ) ;
#25712 = CARTESIAN_POINT ( 'NONE',  ( 200.0000000000000000, 61.50000000000009948, -66.50000000000005684 ) ) ;
#25713 = CARTESIAN_POINT ( 'NONE',  ( 199.0263771353515949, -14.14574067859894413, 14.14574067859863682 ) ) ;
#25714 = VERTEX_POINT ( 'NONE', #26256 ) ;
#25715 = CARTESIAN_POINT ( 'NONE',  ( 0.2972598230769957217, 1.502051041545559470E-13, -14.33493731733933352 ) ) ;
#25716 = CARTESIAN_POINT ( 'NONE',  ( 199.0255773684291967, -18.50957944509308462, 7.588431196845307980 ) ) ;
#25717 = CARTESIAN_POINT ( 'NONE',  ( -47.65341557557733410, 10.55973086684486262, 31.50022537349512319 ) ) ;
#25718 = ORIENTED_EDGE ( 'NONE', *, *, #8336, .F. ) ;
#25719 = ORIENTED_EDGE ( 'NONE', *, *, #10443, .T. ) ;
#25720 = CARTESIAN_POINT ( 'NONE',  ( -193.3669098796383139, -44.23532903079497203, -18.32287322058288126 ) ) ;
#25721 = CARTESIAN_POINT ( 'NONE',  ( -238.4067589809705794, 39.99999999999983658, 40.96449428006354765 ) ) ;
#25722 = CARTESIAN_POINT ( 'NONE',  ( -190.0000000000000000, -71.50000000000002842, -66.50000000000005684 ) ) ;
#25723 = AXIS2_PLACEMENT_3D ( 'NONE', #12926, #3451, #11179 ) ;
#25724 = EDGE_CURVE ( 'NONE', #17668, #17072, #3750, .T. ) ;
#25725 = CARTESIAN_POINT ( 'NONE',  ( -716.9846540392142060, -82.49999999999991473, 52.49999999999977263 ) ) ;
#25726 = CARTESIAN_POINT ( 'NONE',  ( -56.48582580120557850, -40.00000000000014211, 30.84685318188629921 ) ) ;
#25727 = CARTESIAN_POINT ( 'NONE',  ( 200.0000000000000284, -8.407999580957739028, -17.04516676560209376 ) ) ;
#25728 = PRESENTATION_LAYER_ASSIGNMENT (  '', '', ( #11689 ) ) ;
#25729 = AXIS2_PLACEMENT_3D ( 'NONE', #10294, #10161, #8159 ) ;
#25730 = CARTESIAN_POINT ( 'NONE',  ( 136.1360204305621551, 40.00000000000002842, 4.966164525587208445 ) ) ;
#25731 = CARTESIAN_POINT ( 'NONE',  ( -83.21262154144253032, -13.72187187061455127, -33.12752917118434937 ) ) ;
#25732 = CARTESIAN_POINT ( 'NONE',  ( -47.65341557555752416, -10.55973086695903618, -31.50022537343778595 ) ) ;
#25733 = CARTESIAN_POINT ( 'NONE',  ( -208.1127848780264742, -10.60833733270725787, -67.17687982763172272 ) ) ;
#25734 = CARTESIAN_POINT ( 'NONE',  ( 170.0000000000427178, -17.64300463311358769, 17.64300463311318268 ) ) ;
#25735 = CARTESIAN_POINT ( 'NONE',  ( 146.6084372240433709, -40.00000000000036238, 34.62501878078263218 ) ) ;
#25736 = CARTESIAN_POINT ( 'NONE',  ( 23.37394308801976450, 13.80096434448266685, 46.80823611210199431 ) ) ;
#25737 = CARTESIAN_POINT ( 'NONE',  ( 136.1360204305621551, -4.966164525587043244, 40.00000000000002132 ) ) ;
#25738 = CARTESIAN_POINT ( 'NONE',  ( 0.2972598230770129857, -54.33493731733936016, -40.00000000000002132 ) ) ;
#25739 = EDGE_CURVE ( 'NONE', #6802, #19642, #11467, .T. ) ;
#25740 = EDGE_CURVE ( 'NONE', #992, #15670, #19963, .T. ) ;
#25741 = CARTESIAN_POINT ( 'NONE',  ( -56.48582580120559271, 6.472252184284211118, -6.472252184284153387 ) ) ;
#25742 = VECTOR ( 'NONE', #25971, 1000.000000000000000 ) ;
#25743 = CARTESIAN_POINT ( 'NONE',  ( 14.38125909742181285, -15.17850393972633505, 0.000000000000000000 ) ) ;
#25745 = CARTESIAN_POINT ( 'NONE',  ( -317.0000000000000568, -4.857225732735059864E-14, 28.79780246617542616 ) ) ;
#25744 = CARTESIAN_POINT ( 'NONE',  ( 22.89172254855148481, -43.00256445985474585, -23.44749030158409298 ) ) ;
#25746 = AXIS2_PLACEMENT_3D ( 'NONE', #1208, #7556, #17168 ) ;
#25747 = FACE_OUTER_BOUND ( 'NONE', #17977, .T. ) ;
#25748 = CARTESIAN_POINT ( 'NONE',  ( 151.7948205124836250, 4.785054706301690608, 4.785054706301682614 ) ) ;
#25749 = CARTESIAN_POINT ( 'NONE',  ( -208.1127848780264742, 55.00245453010919050, -40.00000000000002132 ) ) ;
#25750 = ORIENTED_EDGE ( 'NONE', *, *, #13068, .F. ) ;
#25751 = CARTESIAN_POINT ( 'NONE',  ( 23.05038679986302341, -43.09692730307091324, 17.85133178553853739 ) ) ;
#25752 = CIRCLE ( 'NONE', #22781, 5.000000000000004441 ) ;
#25753 = B_SPLINE_CURVE_WITH_KNOTS ( 'NONE', 3,
 ( #8778, #2803, #934, #6378, #24758, #17019 ),
 .UNSPECIFIED., .F., .F.,
 ( 4, 2, 4 ),
 ( 0.3689590070116580689, 0.3867117631979620773, 0.4044645193949217288 ),
 .UNSPECIFIED. ) ;
#25754 = DIRECTION ( 'NONE',  ( 0.000000000000000000, 1.000000000000000000, 0.000000000000000000 ) ) ;
#25755 = CARTESIAN_POINT ( 'NONE',  ( -280.0000000000000568, 42.42640687119285303, -14.14213562373088351 ) ) ;
#25756 = CARTESIAN_POINT ( 'NONE',  ( 0.2972598230770030492, -40.00000000000007816, 14.33493731733919496 ) ) ;
#25757 = CARTESIAN_POINT ( 'NONE',  ( 170.2234770963711128, -17.36149277827010096, 17.36149277826970660 ) ) ;
#25758 = AXIS2_PLACEMENT_3D ( 'NONE', #23122, #4895, #21252 ) ;
#25759 = CARTESIAN_POINT ( 'NONE',  ( -238.4067589809705794, 0.9644942799825385604, -40.00000000000002132 ) ) ;
#25760 = CARTESIAN_POINT ( 'NONE',  ( 190.0000000000000000, 71.50000000000009948, -66.50000000000005684 ) ) ;
#25761 = CARTESIAN_POINT ( 'NONE',  ( 199.9999999999998863, -9.236595569432955344, 16.61620204157069125 ) ) ;
#25762 = CARTESIAN_POINT ( 'NONE',  ( -86.94888381182468606, -6.689462128214199055, -20.30418897962128000 ) ) ;
#25763 = CARTESIAN_POINT ( 'NONE',  ( -86.96347745069644475, 12.89780903124349898, 43.67073346367994446 ) ) ;
#25764 = CARTESIAN_POINT ( 'NONE',  ( -30.26275506840325136, 27.08623969584614244, -29.48230279907770779 ) ) ;
#25765 = CARTESIAN_POINT ( 'NONE',  ( 163.1118516004056573, 19.27778845538780317, -19.27778845538757224 ) ) ;
#25766 = CARTESIAN_POINT ( 'NONE',  ( -83.21262154144248768, 33.12752917118453411, -13.72187187061400415 ) ) ;
#25767 = CARTESIAN_POINT ( 'NONE',  ( 14.38125909742181996, -10.73282306405815234, -67.30136555898266693 ) ) ;
#25769 = CARTESIAN_POINT ( 'NONE',  ( 130.8568914410475088, -24.07718906446864793, -32.49135343045505664 ) ) ;
#25768 = CARTESIAN_POINT ( 'NONE',  ( -30.26275506840323359, -1.198031551615522439, -57.76657404653986561 ) ) ;
#25770 = CARTESIAN_POINT ( 'NONE',  ( 0.2972598230769990524, -18.14793986248671231, -38.42060263243687501 ) ) ;
#25771 = CYLINDRICAL_SURFACE ( 'NONE', #24036, 5.000000000000004441 ) ;
#25772 = PLANE ( 'NONE',  #1313 ) ;
#25773 = CARTESIAN_POINT ( 'NONE',  ( -198.0356074513804572, -40.00000000000011369, 15.37879056873056527 ) ) ;
#25774 = CARTESIAN_POINT ( 'NONE',  ( 151.7948205124836250, -23.49921654116371883, 23.49921654116317526 ) ) ;
#25775 = CARTESIAN_POINT ( 'NONE',  ( 14.38125909742180752, 55.17850393974265444, 40.00000000000002132 ) ) ;
#25776 = ORIENTED_EDGE ( 'NONE', *, *, #6452, .T. ) ;
#25777 = AXIS2_PLACEMENT_3D ( 'NONE', #13257, #21380, #3152 ) ;
#25778 = CARTESIAN_POINT ( 'NONE',  ( 200.0000000000000000, 42.42640687119288856, -14.14213562373094746 ) ) ;
#25779 = CARTESIAN_POINT ( 'NONE',  ( -41.56387280713217791, 32.03616492527998361, 13.26981399847223564 ) ) ;
#25780 = CARTESIAN_POINT ( 'NONE',  ( 98.29820294267331349, 7.653668647304012751, 18.47759065023121039 ) ) ;
#25781 = CARTESIAN_POINT ( 'NONE',  ( -105.2940237833723813, -4.710801307188510201, 20.91877113669150745 ) ) ;
#25782 = ORIENTED_EDGE ( 'NONE', *, *, #348, .T. ) ;
#25783 = CARTESIAN_POINT ( 'NONE',  ( -188.9524464570969258, -47.22058047019496740, 13.86227157644530017 ) ) ;
#25784 = CARTESIAN_POINT ( 'NONE',  ( 199.9999999999998295, -7.847915761074617080, -17.31000481134407565 ) ) ;
#25785 = CARTESIAN_POINT ( 'NONE',  ( 60.07376046262002944, -13.17995839195482333, 31.81923430127606167 ) ) ;
#25786 = CARTESIAN_POINT ( 'NONE',  ( 23.10188454848723083, 23.40120037233813477, -42.94013537404166669 ) ) ;
#25787 = CARTESIAN_POINT ( 'NONE',  ( 199.0073354103614918, 19.73522450985164411, -3.233483297802316692 ) ) ;
#25788 = UNCERTAINTY_MEASURE_WITH_UNIT (LENGTH_MEASURE( 1.000000000000000082E-05 ), #19170, 'distance_accuracy_value', 'NONE');
#25789 = CARTESIAN_POINT ( 'NONE',  ( -200.0000000000000000, 69.99999999999998579, 8.572527594031466682E-15 ) ) ;
#25790 = CARTESIAN_POINT ( 'NONE',  ( 151.7948205124836534, 40.00000000000002842, 6.767089262349174739 ) ) ;
#25792 = AXIS2_PLACEMENT_3D ( 'NONE', #3068, #13173, #6916 ) ;
#25791 = FACE_OUTER_BOUND ( 'NONE', #16118, .T. ) ;
#25793 = CARTESIAN_POINT ( 'NONE',  ( 23.23834162557336924, 46.85950693575997406, -13.80856396595088320 ) ) ;
#25794 = CARTESIAN_POINT ( 'NONE',  ( -213.1075012329537230, -13.71589010951915810, 40.00000000000002132 ) ) ;
#25796 = DIRECTION ( 'NONE',  ( -1.000000000000000000, 0.000000000000000000, 0.000000000000000000 ) ) ;
#25795 = CARTESIAN_POINT ( 'NONE',  ( 98.29820294267329928, -7.653668647303861761, -18.47759065023126013 ) ) ;
#25797 = CARTESIAN_POINT ( 'NONE',  ( -370.0000000000001137, -4.857225732735059864E-14, 10.00000000000004796 ) ) ;
#25798 = CARTESIAN_POINT ( 'NONE',  ( -213.1075012329537230, -53.71589010953668719, -40.00000000000002132 ) ) ;
#25799 = CARTESIAN_POINT ( 'NONE',  ( -56.48582580120559271, -9.153146818113595984, 0.000000000000000000 ) ) ;
#25800 = CARTESIAN_POINT ( 'NONE',  ( 170.2234770963711128, 40.00000000000021316, -15.44714144992773797 ) ) ;
#25801 = PLANE ( 'NONE',  #13555 ) ;
#25802 = CARTESIAN_POINT ( 'NONE',  ( -30.26275506840324070, -1.198031551616016266, -1.198031551616031587 ) ) ;
#25803 = ADVANCED_BREP_SHAPE_REPRESENTATION ( '', ( #25811, #21058 ), #9559 ) ;
#25804 = VERTEX_POINT ( 'NONE', #22116 ) ;
#25805 = CARTESIAN_POINT ( 'NONE',  ( 98.29820294267338454, 8.858778887860573548, -17.94316440882722929 ) ) ;
#25806 = CARTESIAN_POINT ( 'NONE',  ( 192.4448373802101173, 20.00000000003945644, 40.00000000000002132 ) ) ;
#25807 = SURFACE_STYLE_FILL_AREA ( #7176 ) ;
#25808 = DIRECTION ( 'NONE',  ( 0.000000000000000000, -1.000000000000000000, 0.000000000000000000 ) ) ;
#25809 = DIRECTION ( 'NONE',  ( 0.000000000000000000, 0.000000000000000000, 1.000000000000000000 ) ) ;
#25810 = VERTEX_POINT ( 'NONE', #9734 ) ;
#25811 = MANIFOLD_SOLID_BREP ( 'Boss-Extrude13', #3243 ) ;
#25812 = EDGE_LOOP ( 'NONE', ( #8805, #19211, #158, #23837, #20515 ) ) ;
#25813 = CARTESIAN_POINT ( 'NONE',  ( -100.0753760173624869, -20.41987330121788702, 8.894334231739227548 ) ) ;
#25814 = CARTESIAN_POINT ( 'NONE',  ( 158.3379117892984880, 10.98149362779651206, -26.51167085133954160 ) ) ;
#25815 = ORIENTED_EDGE ( 'NONE', *, *, #23857, .T. ) ;
#25816 = CARTESIAN_POINT ( 'NONE',  ( 0.2972598230769930017, 54.33493731733938148, -40.00000000000002132 ) ) ;
#25817 = CARTESIAN_POINT ( 'NONE',  ( -99.31364972221751941, -20.79869444138732959, 8.164808577175515225 ) ) ;
#25818 = ORIENTED_EDGE ( 'NONE', *, *, #58, .F. ) ;
#25819 = CARTESIAN_POINT ( 'NONE',  ( 199.9999999999999147, -11.82758851212937579, 14.88619241608240529 ) ) ;
#25820 = DIRECTION ( 'NONE',  ( 0.8802361161597901384, 5.811389476877143134E-17, 0.4745359626076072757 ) ) ;
#25821 = EDGE_CURVE ( 'NONE', #5675, #9962, #4295, .T. ) ;
#25822 = CARTESIAN_POINT ( 'NONE',  ( 91.82158438592158234, 44.40256751092336884, -12.16597498400043342 ) ) ;
#25823 = DIRECTION ( 'NONE',  ( 0.000000000000000000, 1.000000000000000000, 0.000000000000000000 ) ) ;
#25824 = CARTESIAN_POINT ( 'NONE',  ( 14.38125909742181108, -5.035366881890652543E-14, 15.17850393972633682 ) ) ;
#25825 = CARTESIAN_POINT ( 'NONE',  ( -1.828631717523949929, -13.94691770808705478, 47.79123445029436823 ) ) ;
#25826 = CARTESIAN_POINT ( 'NONE',  ( -87.13361725327072804, 8.813415818526478339E-15, 21.49321519333429009 ) ) ;
#25827 = EDGE_CURVE ( 'NONE', #10128, #25302, #12385, .T. ) ;
#25828 = CARTESIAN_POINT ( 'NONE',  ( 98.29820294267867098, 15.96737102139294606, 12.31690022607448221 ) ) ;
#25829 = CARTESIAN_POINT ( 'NONE',  ( -99.21568817060986589, -16.03295912088728770, 16.03295912088687913 ) ) ;
#25830 = CARTESIAN_POINT ( 'NONE',  ( 4.995406935893297984, -39.99999999999986500, -15.24977328854874870 ) ) ;
#25831 = CARTESIAN_POINT ( 'NONE',  ( -114.6097568999262393, -10.88341597697256269, 19.09891331899296318 ) ) ;
#25832 = CARTESIAN_POINT ( 'NONE',  ( 192.4448373802101173, -14.14213562370283128, -42.42640687122081999 ) ) ;
#25833 = CARTESIAN_POINT ( 'NONE',  ( 136.1360204305621551, 40.00000000000017053, -35.03383547441281820 ) ) ;
#25834 = EDGE_CURVE ( 'NONE', #13991, #19296, #24229, .T. ) ;
#25835 = CARTESIAN_POINT ( 'NONE',  ( -208.1127848780264742, -38.89260858015728672, -17.67593391476669851 ) ) ;
#25836 = CARTESIAN_POINT ( 'NONE',  ( 140.2235668266256425, 30.42137084504298628, 12.60094438999839994 ) ) ;
#25837 = EDGE_CURVE ( 'NONE', #15268, #17459, #11893, .T. ) ;
#25838 = CARTESIAN_POINT ( 'NONE',  ( -626.9846540392142060, 90.00000000000000000, 0.000000000000000000 ) ) ;
#25839 = FACE_OUTER_BOUND ( 'NONE', #26260, .T. ) ;
#25840 = CARTESIAN_POINT ( 'NONE',  ( -135.8532207217289738, 7.002209520526292428E-15, -9.153146818113572891 ) ) ;
#25841 = CARTESIAN_POINT ( 'NONE',  ( -259.2033419157646676, -6.730120644403667640, 49.83842185052029805 ) ) ;
#25842 = CARTESIAN_POINT ( 'NONE',  ( 57.59792236341148453, -54.84617931850879557, 1.722363176414566155 ) ) ;
#25843 = CARTESIAN_POINT ( 'NONE',  ( -183.6285492669668997, -17.34367427887346480, -41.87133366542966684 ) ) ;
#25844 = CARTESIAN_POINT ( 'NONE',  ( 91.82158438592158234, 12.16597498397773869, -12.16597498397759303 ) ) ;
#25845 = VERTEX_POINT ( 'NONE', #19976 ) ;
#25846 = CARTESIAN_POINT ( 'NONE',  ( 91.82158438592158234, 16.11829626346161604, -16.11829626346121103 ) ) ;
#25847 = LINE ( 'NONE', #13843, #9401 ) ;
#25848 = CARTESIAN_POINT ( 'NONE',  ( -53.37717264285771535, 10.11115224722917993, -29.42738956023907093 ) ) ;
#25849 = CARTESIAN_POINT ( 'NONE',  ( 199.9999999999999432, 14.14213562373110911, -14.14213562373072364 ) ) ;
#25850 = CARTESIAN_POINT ( 'NONE',  ( -77.90255099907052738, 8.064892378688682584, 20.29001641119209154 ) ) ;
#25851 = ORIENTED_EDGE ( 'NONE', *, *, #9629, .F. ) ;
#25852 = CARTESIAN_POINT ( 'NONE',  ( 199.9999999999999716, 14.31544119637113432, -12.55530011466301055 ) ) ;
#25853 = CARTESIAN_POINT ( 'NONE',  ( 199.0157566623909702, -13.86784264559070756, -14.41179826723872459 ) ) ;
#25854 = CARTESIAN_POINT ( 'NONE',  ( 8.517493242716003721, -44.90626920808415434, 24.85395068094661397 ) ) ;
#25855 = ORIENTED_EDGE ( 'NONE', *, *, #5343, .T. ) ;
#25856 = ORIENTED_EDGE ( 'NONE', *, *, #19065, .T. ) ;
#25857 = CARTESIAN_POINT ( 'NONE',  ( -56.48582580120559982, 30.84685318188643777, -40.00000000000002132 ) ) ;
#25858 = FACE_OUTER_BOUND ( 'NONE', #11095, .T. ) ;
#25859 = CARTESIAN_POINT ( 'NONE',  ( -162.0762913951021176, 39.99999999999998579, 1.694272876828463614 ) ) ;
#25860 = CARTESIAN_POINT ( 'NONE',  ( 190.0000000000001137, -30.00000000000000711, 3.673940397442064700E-15 ) ) ;
#25861 = CARTESIAN_POINT ( 'NONE',  ( -208.1127848780265026, 1.189126717069624012E-13, -15.00245453012669472 ) ) ;
#25862 = CARTESIAN_POINT ( 'NONE',  ( 130.8568914410475372, 8.154165912415230659E-16, 5.949712681206690945 ) ) ;
#25863 = CARTESIAN_POINT ( 'NONE',  ( 199.9999999999998863, -11.20618975336454071, -15.34975362513495689 ) ) ;
#25864 = CARTESIAN_POINT ( 'NONE',  ( -208.1127848780264742, 39.99999999999992895, 15.00245453012683683 ) ) ;
#25865 = CARTESIAN_POINT ( 'NONE',  ( -121.3893627896829770, 22.57752009493451339, 9.351915028061926094 ) ) ;
#25866 = CARTESIAN_POINT ( 'NONE',  ( -135.8532207217289738, -6.472252184284280396, 6.472252184284099208 ) ) ;
#25867 = CARTESIAN_POINT ( 'NONE',  ( 151.7948205124836250, 23.49921654116328540, 23.49921654116366554 ) ) ;
#25868 = DIRECTION ( 'NONE',  ( -1.000000000000000000, -1.836970198721030181E-16, -0.000000000000000000 ) ) ;
#25869 = CARTESIAN_POINT ( 'NONE',  ( 14.38125909742181818, -39.99999999999986500, -15.17850393972675604 ) ) ;
#25870 = CARTESIAN_POINT ( 'NONE',  ( -726.9846540392142060, -82.49999999999991473, 52.49999999999977263 ) ) ;
#25871 = CARTESIAN_POINT ( 'NONE',  ( 19.06497207195982924, -54.19242893257843008, 40.00000000000002132 ) ) ;
#25872 = CARTESIAN_POINT ( 'NONE',  ( -105.3755690713226585, -18.24025645688353947, -40.00000000000002132 ) ) ;
#25873 = CARTESIAN_POINT ( 'NONE',  ( 170.2234770963711128, 45.64576402573181468, 10.92277846919223627 ) ) ;
#25874 = CARTESIAN_POINT ( 'NONE',  ( -86.96347745069645896, 21.75974354311648895, -0.000000000000000000 ) ) ;
#25875 = CARTESIAN_POINT ( 'NONE',  ( -105.2054292635175443, 0.6800022380124111088, 21.49321519473986442 ) ) ;
#25876 = CARTESIAN_POINT ( 'NONE',  ( 14.38125909742181108, 1.616281842095393922E-13, -15.17850393972633682 ) ) ;
#25877 = CARTESIAN_POINT ( 'NONE',  ( -280.0000000000000568, 42.42640687119285303, -14.14213562373088351 ) ) ;
#25878 = CARTESIAN_POINT ( 'NONE',  ( -213.1075012329537230, 53.71589010951910836, 2.449293598294708485E-15 ) ) ;
#25880 = ORIENTED_EDGE ( 'NONE', *, *, #14642, .F. ) ;
#25879 = VECTOR ( 'NONE', #17992, 1000.000000000000000 ) ;
#25881 = EDGE_CURVE ( 'NONE', #151, #23459, #4237, .T. ) ;
#25882 = CARTESIAN_POINT ( 'NONE',  ( 44.46627453565378119, -36.79413088022850786, 15.24062802607578249 ) ) ;
#25883 = DIRECTION ( 'NONE',  ( 1.000000000000000000, 0.000000000000000000, 0.000000000000000000 ) ) ;
#25884 = CARTESIAN_POINT ( 'NONE',  ( 170.2234770963711128, 39.20704971665398375, -17.36149277826984871 ) ) ;
#25885 = CARTESIAN_POINT ( 'NONE',  ( 130.8568914410475372, 8.154165912415230659E-16, 5.949712681206690945 ) ) ;
#25886 = CARTESIAN_POINT ( 'NONE',  ( 4.995406935893289102, 10.78321810389013002, -10.78321810388986712 ) ) ;
#25887 = EDGE_CURVE ( 'NONE', #22617, #13720, #17220, .T. ) ;
#25888 = CARTESIAN_POINT ( 'NONE',  ( 0.2972598230769930572, 14.33493731733933352, 0.000000000000000000 ) ) ;
#25889 = CARTESIAN_POINT ( 'NONE',  ( 200.0000000000000000, -20.00000000000006750, -40.00000000000002132 ) ) ;
#25890 = PRODUCT_DEFINITION_SHAPE ( 'NONE', 'NONE',  #26366 ) ;
#25891 = CARTESIAN_POINT ( 'NONE',  ( -175.9234121947850440, -39.35887396291793294, -21.03678982257773455 ) ) ;
#25892 = CARTESIAN_POINT ( 'NONE',  ( 199.9999999999999432, 3.548988777896260771, 18.67457114543681485 ) ) ;
#25893 = CARTESIAN_POINT ( 'NONE',  ( 170.0000000000427178, -17.64300463311358769, 17.64300463311318268 ) ) ;
#25894 = CARTESIAN_POINT ( 'NONE',  ( -280.0000000000000000, -14.14213562373118549, 14.14213562373078936 ) ) ;
#25895 = CARTESIAN_POINT ( 'NONE',  ( -56.48582580120558561, -21.81201906317755146, -21.81201906317792449 ) ) ;
#25896 = CARTESIAN_POINT ( 'NONE',  ( -190.1760961840481627, -13.92889018258695799, 47.67020129369084458 ) ) ;
#25897 = CARTESIAN_POINT ( 'NONE',  ( -77.55632011646486035, 15.16702236932743375, -16.13210123263645812 ) ) ;
#25898 = CARTESIAN_POINT ( 'NONE',  ( 151.7948205124836534, 23.49921654116056047, -33.06932595376338213 ) ) ;
#25900 = CARTESIAN_POINT ( 'NONE',  ( 130.8568914410475088, -52.36146031193413108, -4.207082182990267150 ) ) ;
#25899 = CARTESIAN_POINT ( 'NONE',  ( -86.96347745069644475, -12.89780903124395195, -12.89780903124416511 ) ) ;
#25901 = CARTESIAN_POINT ( 'NONE',  ( -105.3755690713226585, -43.67073346367964604, -12.89780903124457545 ) ) ;
#25902 = FACE_OUTER_BOUND ( 'NONE', #3458, .T. ) ;
#25903 = DIRECTION ( 'NONE',  ( -1.000000000000000000, -1.836970198721030181E-16, 0.000000000000000000 ) ) ;
#25904 = AXIS2_PLACEMENT_3D ( 'NONE', #20248, #4023, #5385 ) ;
#25906 = CARTESIAN_POINT ( 'NONE',  ( 151.7948205124836250, 1.439163438361279259E-13, -33.23291073765553705 ) ) ;
#25905 = CARTESIAN_POINT ( 'NONE',  ( -213.1075012329537230, 66.26714140138673770, -9.698598906462034819 ) ) ;
#25907 = CARTESIAN_POINT ( 'NONE',  ( -192.9588430854690273, -10.23066800229550388, 66.79921049721887982 ) ) ;
#25908 = CARTESIAN_POINT ( 'NONE',  ( -162.0762913951020892, -1.198031840385767266, -1.198031840385758384 ) ) ;
#25909 = CARTESIAN_POINT ( 'NONE',  ( -162.0762913951021176, 41.69427287672986182, 40.00000000000002132 ) ) ;
#25910 = ORIENTED_EDGE ( 'NONE', *, *, #15882, .T. ) ;
#25911 = CARTESIAN_POINT ( 'NONE',  ( 192.4448373802101173, 14.14213562370320076, -42.42640687122072762 ) ) ;
#25912 = EDGE_CURVE ( 'NONE', #25369, #19288, #21875, .T. ) ;
#25913 = DIRECTION ( 'NONE',  ( 1.000000000000000000, 0.000000000000000000, 0.000000000000000000 ) ) ;
#25914 = CARTESIAN_POINT ( 'NONE',  ( 23.46661716382972429, 23.32081713244427590, 42.82867125331105740 ) ) ;
#25915 = CARTESIAN_POINT ( 'NONE',  ( -56.48582580120559982, -9.153146818113595984, 40.00000000000002132 ) ) ;
#25916 = VERTEX_POINT ( 'NONE', #18776 ) ;
#25917 = CARTESIAN_POINT ( 'NONE',  ( -188.3120147333417549, -46.99495896211615786, 13.82877842034796068 ) ) ;
#25918 = CARTESIAN_POINT ( 'NONE',  ( 200.0000000000000568, -14.79650836250383250, 11.93661649116771173 ) ) ;
#25919 = CARTESIAN_POINT ( 'NONE',  ( -3.921555385250262482, -13.83441994316381241, 47.03297225793202330 ) ) ;
#25920 = ADVANCED_FACE ( 'NONE', ( #23172 ), #12653, .T. ) ;
#25921 = EDGE_CURVE ( 'NONE', #15233, #6802, #2995, .T. ) ;
#25922 = AXIS2_PLACEMENT_3D ( 'NONE', #19385, #19260, #16999 ) ;
#25923 = CARTESIAN_POINT ( 'NONE',  ( 23.48902902575293794, 13.79248457098146119, -46.76665409567217324 ) ) ;
#25924 = CARTESIAN_POINT ( 'NONE',  ( 199.0060751070798233, 18.35498561216385482, -7.937441424495496278 ) ) ;
#25925 = CARTESIAN_POINT ( 'NONE',  ( 110.0479209278586410, -22.74092928740055086, 9.419601331808566513 ) ) ;
#25926 = CARTESIAN_POINT ( 'NONE',  ( 190.0000000000000000, -52.49999999999972289, -82.49999999999998579 ) ) ;
#25927 = CARTESIAN_POINT ( 'NONE',  ( -77.55640685876515761, -9.396736996787120630E-14, 22.13135000837099398 ) ) ;
#25928 =( BOUNDED_SURFACE ( )  B_SPLINE_SURFACE ( 3, 3, ( 
 ( #15986, #13994, #16390, #22125, #16120, #164, #14131, #14395, #18516, #21991, #22260, #297, #8401, #1769, #3760, #19985, #9875, #12003, #10808, #14648, #25183, #10942, #16655, #832, #20789, #18918, #22787, #12662, #8941, #8538 ),
 ( #700, #4828, #14915, #2703, #21049, #4566, #22655, #12933, #2560, #6932, #16918, #6538, #25052, #4429, #20653, #8806, #2427, #4695, #6803, #10675, #18788, #15050, #569, #22916, #8674, #16783, #2833, #19050, #6407, #12797 ),
 ( #17047, #24919, #14524, #20924, #12522, #10537, #18649, #23056, #434, #24786, #14786, #6671, #12471, #10221, #1848, #109, #20469, #20598, #6489, #18328, #8216, #18060, #239, #22472, #2374, #4251, #24463, #8083, #16202, #24733 ),
 ( #20335, #16334, #14471, #14601, #3982, #8351, #6228, #14076, #4380, #12079, #24597, #14341, #10486, #22604, #18600, #24335, #378, #8483, #11947, #12341, #16600, #2244, #9951, #10351, #18461, #3843, #20072, #16472, #6352, #26211 ),
 ( #7947, #20201, #16065, #24192, #1980, #22340, #5965, #22207, #10086, #6099, #14206, #18190, #26341, #4116, #12213, #2112, #14735, #9139, #23001, #10756, #2911, #9024, #2508, #19259, #10892, #17128, #8621, #4778, #19129, #21263 ),
 ( #19004, #12882, #648, #17255, #11019, #22867, #20998, #2780, #10619, #18867, #16732, #516, #25259, #4644, #8754, #7010, #14867, #15131, #4905, #22731, #781, #8887, #25002, #18733, #16998, #7143, #11144, #25133, #13016, #20866 ),
 ( #23261, #12610, #24863, #6618, #4509, #2650, #1039, #6884, #5037, #911, #23133, #13144, #3035, #21136, #25391, #16870, #20739, #12746, #6755, #14998, #3540, #5282, #11640, #13268, #11264, #13641, #19383, #1421, #21767, #17505 ) ),
 .UNSPECIFIED., .T., .F., .F. ) 
 B_SPLINE_SURFACE_WITH_KNOTS ( ( 4, 3, 4 ),
 ( 4, 2, 2, 2, 2, 2, 2, 2, 2, 2, 2, 2, 2, 2, 4 ),
 ( 0.000000000000000000, 0.5000000000000000000, 1.000000000000000000 ),
 ( 0.000000000000000000, 0.1357259735107005372, 0.1651108541090157700, 0.1944957347073310028, 0.3598804999793158710, 0.3867117631979620773, 0.4135430264166082281, 0.5789277916885930964, 0.6062785021374117456, 0.6336292125862302838, 0.8508620842112317728, 0.8814014469398914198, 0.9119408096685510667, 0.9559704048342755334, 1.000000000000000000 ),
 .UNSPECIFIED. ) 
 GEOMETRIC_REPRESENTATION_ITEM ( )  RATIONAL_B_SPLINE_SURFACE ( (
 ( 1.000000000000000000, 1.000000000000000000, 1.000000000000000000, 1.000000000000000000, 1.000000000000000000, 1.000000000000000000, 1.000000000000000000, 1.000000000000000000, 1.000000000000000000, 1.000000000000000000, 1.000000000000000000, 1.000000000000000000, 1.000000000000000000, 1.000000000000000000, 1.000000000000000000, 1.000000000000000000, 1.000000000000000000, 1.000000000000000000, 1.000000000000000000, 1.000000000000000000, 1.000000000000000000, 1.000000000000000000, 1.000000000000000000, 1.000000000000000000, 1.000000000000000000, 1.000000000000000000, 1.000000000000000000, 1.000000000000000000, 1.000000000000000000, 1.000000000000000000),
 ( 0.3333333333333333703, 0.3333333333333333703, 0.3333333333333333703, 0.3333333333333333703, 0.3333333333333333703, 0.3333333333333333703, 0.3333333333333333703, 0.3333333333333333703, 0.3333333333333333703, 0.3333333333333333703, 0.3333333333333333703, 0.3333333333333333703, 0.3333333333333333703, 0.3333333333333333703, 0.3333333333333333703, 0.3333333333333333703, 0.3333333333333333703, 0.3333333333333333703, 0.3333333333333333703, 0.3333333333333333703, 0.3333333333333333703, 0.3333333333333333703, 0.3333333333333333703, 0.3333333333333333703, 0.3333333333333333703, 0.3333333333333333703, 0.3333333333333333703, 0.3333333333333333703, 0.3333333333333333703, 0.3333333333333333703),
 ( 0.3333333333333333703, 0.3333333333333333703, 0.3333333333333333703, 0.3333333333333333703, 0.3333333333333333703, 0.3333333333333333703, 0.3333333333333333703, 0.3333333333333333703, 0.3333333333333333703, 0.3333333333333333703, 0.3333333333333333703, 0.3333333333333333703, 0.3333333333333333703, 0.3333333333333333703, 0.3333333333333333703, 0.3333333333333333703, 0.3333333333333333703, 0.3333333333333333703, 0.3333333333333333703, 0.3333333333333333703, 0.3333333333333333703, 0.3333333333333333703, 0.3333333333333333703, 0.3333333333333333703, 0.3333333333333333703, 0.3333333333333333703, 0.3333333333333333703, 0.3333333333333333703, 0.3333333333333333703, 0.3333333333333333703),
 ( 1.000000000000000000, 1.000000000000000000, 1.000000000000000000, 1.000000000000000000, 1.000000000000000000, 1.000000000000000000, 1.000000000000000000, 1.000000000000000000, 1.000000000000000000, 1.000000000000000000, 1.000000000000000000, 1.000000000000000000, 1.000000000000000000, 1.000000000000000000, 1.000000000000000000, 1.000000000000000000, 1.000000000000000000, 1.000000000000000000, 1.000000000000000000, 1.000000000000000000, 1.000000000000000000, 1.000000000000000000, 1.000000000000000000, 1.000000000000000000, 1.000000000000000000, 1.000000000000000000, 1.000000000000000000, 1.000000000000000000, 1.000000000000000000, 1.000000000000000000),
 ( 0.3333333333333333703, 0.3333333333333333703, 0.3333333333333333703, 0.3333333333333333703, 0.3333333333333333703, 0.3333333333333333703, 0.3333333333333333703, 0.3333333333333333703, 0.3333333333333333703, 0.3333333333333333703, 0.3333333333333333703, 0.3333333333333333703, 0.3333333333333333703, 0.3333333333333333703, 0.3333333333333333703, 0.3333333333333333703, 0.3333333333333333703, 0.3333333333333333703, 0.3333333333333333703, 0.3333333333333333703, 0.3333333333333333703, 0.3333333333333333703, 0.3333333333333333703, 0.3333333333333333703, 0.3333333333333333703, 0.3333333333333333703, 0.3333333333333333703, 0.3333333333333333703, 0.3333333333333333703, 0.3333333333333333703),
 ( 0.3333333333333333703, 0.3333333333333333703, 0.3333333333333333703, 0.3333333333333333703, 0.3333333333333333703, 0.3333333333333333703, 0.3333333333333333703, 0.3333333333333333703, 0.3333333333333333703, 0.3333333333333333703, 0.3333333333333333703, 0.3333333333333333703, 0.3333333333333333703, 0.3333333333333333703, 0.3333333333333333703, 0.3333333333333333703, 0.3333333333333333703, 0.3333333333333333703, 0.3333333333333333703, 0.3333333333333333703, 0.3333333333333333703, 0.3333333333333333703, 0.3333333333333333703, 0.3333333333333333703, 0.3333333333333333703, 0.3333333333333333703, 0.3333333333333333703, 0.3333333333333333703, 0.3333333333333333703, 0.3333333333333333703),
 ( 1.000000000000000000, 1.000000000000000000, 1.000000000000000000, 1.000000000000000000, 1.000000000000000000, 1.000000000000000000, 1.000000000000000000, 1.000000000000000000, 1.000000000000000000, 1.000000000000000000, 1.000000000000000000, 1.000000000000000000, 1.000000000000000000, 1.000000000000000000, 1.000000000000000000, 1.000000000000000000, 1.000000000000000000, 1.000000000000000000, 1.000000000000000000, 1.000000000000000000, 1.000000000000000000, 1.000000000000000000, 1.000000000000000000, 1.000000000000000000, 1.000000000000000000, 1.000000000000000000, 1.000000000000000000, 1.000000000000000000, 1.000000000000000000, 1.000000000000000000) ) ) 
 REPRESENTATION_ITEM ( '' )  SURFACE ( )  );
#25929 = CARTESIAN_POINT ( 'NONE',  ( 184.8905102610680444, 41.77492675555983936, 14.79361573936436081 ) ) ;
#25930 = CARTESIAN_POINT ( 'NONE',  ( 170.2234770963711128, -15.44714144992813409, 40.00000000000002132 ) ) ;
#25932 = CARTESIAN_POINT ( 'NONE',  ( -598.0754867585920920, 39.18842370550271426, -8.032326897551609335 ) ) ;
#25931 = CARTESIAN_POINT ( 'NONE',  ( 60.14720761606899657, -10.94158980359358324, -33.22245024492937659 ) ) ;
#25933 = CARTESIAN_POINT ( 'NONE',  ( 169.9999999999999716, -125.7889608577475116, 82.50000000000001421 ) ) ;
#25934 = CARTESIAN_POINT ( 'NONE',  ( -259.2033419157646676, 9.517827891722582478, -40.00000000000002132 ) ) ;
#25935 = CARTESIAN_POINT ( 'NONE',  ( 170.2234770963711128, -24.55285855007184281, 40.00000000000002132 ) ) ;
#25936 = CARTESIAN_POINT ( 'NONE',  ( -100.7734535825088500, -39.99999999999986500, -17.32597176626853397 ) ) ;
#25937 = CARTESIAN_POINT ( 'NONE',  ( 184.8905102610680444, -1.851754852062639767E-13, 20.92133201514444352 ) ) ;
#25938 = CARTESIAN_POINT ( 'NONE',  ( 4.995406935893287326, 17.50105314357225694, -39.06748935135176026 ) ) ;
#25939 = ORIENTED_EDGE ( 'NONE', *, *, #19163, .F. ) ;
#25940 = DIRECTION ( 'NONE',  ( 1.000000000000000000, 0.000000000000000000, -0.000000000000000000 ) ) ;
#25941 = CARTESIAN_POINT ( 'NONE',  ( -198.0356074513804572, -15.37879056873074290, 0.000000000000000000 ) ) ;
#25942 = CIRCLE ( 'NONE', #11073, 46.18033988749894547 ) ;
#25943 = CARTESIAN_POINT ( 'NONE',  ( 184.5754832356733459, -14.84877008830847345, 14.84877008830815015 ) ) ;
#25944 = CARTESIAN_POINT ( 'NONE',  ( -188.7701069479164460, 47.15820909662599547, -13.85300054332491371 ) ) ;
#25945 = PRODUCT_CONTEXT ( 'NONE', #20471, 'mechanical' ) ;
#25946 = ORIENTED_EDGE ( 'NONE', *, *, #5254, .F. ) ;
#25947 = EDGE_LOOP ( 'NONE', ( #5947, #10837, #24244, #6833 ) ) ;
#25948 = CARTESIAN_POINT ( 'NONE',  ( 19.06497207195982924, -66.60410523465823474, 10.03556273973400081 ) ) ;
#25949 = CARTESIAN_POINT ( 'NONE',  ( 23.10188454848715978, -42.94013537404167380, -23.40120037234288475 ) ) ;
#25950 = ORIENTED_EDGE ( 'NONE', *, *, #1426, .F. ) ;
#25951 = CARTESIAN_POINT ( 'NONE',  ( -162.0762913951020892, 41.69427287692678163, -40.00000000000002132 ) ) ;
#25952 = PLANE ( 'NONE',  #24932 ) ;
#25953 = VERTEX_POINT ( 'NONE', #823 ) ;
#25954 = CARTESIAN_POINT ( 'NONE',  ( 199.9999999999998295, 13.96930097052764097, 12.88701297307445159 ) ) ;
#25955 = CARTESIAN_POINT ( 'NONE',  ( -175.9234121941017293, 21.03678982652580487, -39.35887396262683069 ) ) ;
#25956 = CARTESIAN_POINT ( 'NONE',  ( 14.38125909742181108, 39.01709431150907648, 39.01709431150921858 ) ) ;
#25957 = DIRECTION ( 'NONE',  ( 0.000000000000000000, -1.000000000000000000, 0.000000000000000000 ) ) ;
#25958 = CARTESIAN_POINT ( 'NONE',  ( 163.1118516004056573, 1.251511021549353291E-13, -27.26290988616872824 ) ) ;
#25959 = CARTESIAN_POINT ( 'NONE',  ( 0.2972598230769930572, 14.33493731733933352, 0.000000000000000000 ) ) ;
#25960 = CARTESIAN_POINT ( 'NONE',  ( -213.1075012329537230, 9.698598906438871126, -66.26714140136179765 ) ) ;
#25961 = DIRECTION ( 'NONE',  ( -1.000000000000000000, 1.836970198721030181E-16, 0.000000000000000000 ) ) ;
#25962 = B_SPLINE_CURVE_WITH_KNOTS ( 'NONE', 3,
 ( #25218, #22825, #23347, #24961, #15217, #16954 ),
 .UNSPECIFIED., .F., .F.,
 ( 4, 2, 4 ),
 ( 1.440969542111313559E-17, 0.03937685683732346925, 0.07875371367464692463 ),
 .UNSPECIFIED. ) ;
#25963 = AXIS2_PLACEMENT_3D ( 'NONE', #10959, #25200, #16800 ) ;
#25964 = LINE ( 'NONE', #23437, #25503 ) ;
#25965 = CARTESIAN_POINT ( 'NONE',  ( 199.9999999999999432, -1.727494763561684666E-13, 20.00000000000010303 ) ) ;
#25966 = CARTESIAN_POINT ( 'NONE',  ( 0.2972598230770030492, -39.99999999999987210, -14.33493731733975451 ) ) ;
#25967 = CARTESIAN_POINT ( 'NONE',  ( -114.7538884075548964, -13.57382480623414445, 17.50182194317655160 ) ) ;
#25968 = CARTESIAN_POINT ( 'NONE',  ( 170.2234770963711128, -39.20704971665379190, -17.36149277827012938 ) ) ;
#25969 = CARTESIAN_POINT ( 'NONE',  ( -213.1075012329537230, -13.71589010951915810, 0.000000000000000000 ) ) ;
#25970 = CARTESIAN_POINT ( 'NONE',  ( 91.82158438592159655, -44.40256751092324095, -12.16597498400075139 ) ) ;
#25971 = DIRECTION ( 'NONE',  ( -1.000000000000000000, -1.836970198721030181E-16, -0.000000000000000000 ) ) ;
#25972 = DIRECTION ( 'NONE',  ( -0.01051738777839801575, 0.9307051272556606802, -0.3656191333263937304 ) ) ;
#25973 = CARTESIAN_POINT ( 'NONE',  ( 165.3321726438165626, 18.76308274333374371, 18.76308274333403503 ) ) ;
#25974 = CARTESIAN_POINT ( 'NONE',  ( 146.6084372240433993, 1.478241399363601114E-13, -34.62501878078305850 ) ) ;
#25975 = CARTESIAN_POINT ( 'NONE',  ( -259.2033419157646676, 21.55415060305830366, 21.55415060305842800 ) ) ;
#25976 = CARTESIAN_POINT ( 'NONE',  ( 19.06497207195981858, -38.31983398719641087, 18.24870850772724040 ) ) ;
#25977 = CARTESIAN_POINT ( 'NONE',  ( -188.3509229510629552, -17.87648076835369437, -43.15764231844840282 ) ) ;
#25978 = CARTESIAN_POINT ( 'NONE',  ( -30.26275506840324070, -29.48230279907780016, -27.08623969584605362 ) ) ;
#25979 = ORIENTED_EDGE ( 'NONE', *, *, #24117, .F. ) ;
#25980 = CARTESIAN_POINT ( 'NONE',  ( -105.3755690713226585, -15.38646221621738164, -41.18208027870615240 ) ) ;
#25981 = CARTESIAN_POINT ( 'NONE',  ( -135.8532207217289738, 6.472252184284186249, -6.472252184284142729 ) ) ;
#25982 = DIRECTION ( 'NONE',  ( 1.000000000000000000, 1.836970198721030427E-16, -0.000000000000000000 ) ) ;
#25983 = PRESENTATION_STYLE_ASSIGNMENT (( #7992 ) ) ;
#25984 = CARTESIAN_POINT ( 'NONE',  ( -91.56559293963834989, -44.31723036834885932, -12.25131212657538171 ) ) ;
#25985 =( LENGTH_UNIT ( ) NAMED_UNIT ( * ) SI_UNIT ( .MILLI., .METRE. ) );
#25986 = CARTESIAN_POINT ( 'NONE',  ( -82.24889283716245814, 3.157952835618418330, 19.94440861093309181 ) ) ;
#25987 = EDGE_LOOP ( 'NONE', ( #17639, #1599 ) ) ;
#25988 = CIRCLE ( 'NONE', #3433, 9.999999999999969802 ) ;
#25989 = CARTESIAN_POINT ( 'NONE',  ( -265.6482238768269326, 0.000000000000000000, 0.000000000000000000 ) ) ;
#25990 = CARTESIAN_POINT ( 'NONE',  ( -105.2054292635176296, -15.67883240738871287, 14.71716402001586665 ) ) ;
#25991 = CARTESIAN_POINT ( 'NONE',  ( -3.494657986429658969, 17.93150516116838844, 43.29048295385586442 ) ) ;
#25992 = AXIS2_PLACEMENT_3D ( 'NONE', #4576, #18800, #12813 ) ;
#25993 = VERTEX_POINT ( 'NONE', #14638 ) ;
#25994 = EDGE_LOOP ( 'NONE', ( #23576, #13460, #24384, #10334 ) ) ;
#25995 = CARTESIAN_POINT ( 'NONE',  ( 163.1118516004056573, 12.73709011382478806, -40.00000000000002132 ) ) ;
#25996 = CARTESIAN_POINT ( 'NONE',  ( 184.8905102610680444, 14.79361573936396113, -14.79361573936377461 ) ) ;
#25997 = CARTESIAN_POINT ( 'NONE',  ( 0.2972598230769956662, 39.99999999999983658, 54.33493731733950938 ) ) ;
#25998 = CARTESIAN_POINT ( 'NONE',  ( 23.37394308801977161, 13.80096434448334186, -46.80823611210181667 ) ) ;
#25999 = EDGE_CURVE ( 'NONE', #13223, #5232, #14677, .T. ) ;
#26000 = CARTESIAN_POINT ( 'NONE',  ( 130.8568914410475372, 4.207082182992923691, -4.207082182992794017 ) ) ;
#26001 = CARTESIAN_POINT ( 'NONE',  ( -162.0762913951020892, -1.202636532414034422E-14, -1.694272876828323948 ) ) ;
#26002 = CARTESIAN_POINT ( 'NONE',  ( 98.29820294267527458, 2.689882573189819553E-13, -20.00000000000500222 ) ) ;
#26003 = VECTOR ( 'NONE', #6805, 1000.000000000000000 ) ;
#26004 = CARTESIAN_POINT ( 'NONE',  ( 199.0249556294982938, -5.033924301686514724, 19.36137939705603017 ) ) ;
#26005 = CARTESIAN_POINT ( 'NONE',  ( -129.2303492455655771, 11.67678589714761017, 24.84170067272852833 ) ) ;
#26006 = CARTESIAN_POINT ( 'NONE',  ( -4.027137536849729749, -23.45200847982304992, -43.00884733904526058 ) ) ;
#26007 = CARTESIAN_POINT ( 'NONE',  ( -105.3755690713226585, -41.18208027870611687, 15.38646221621750954 ) ) ;
#26008 = CARTESIAN_POINT ( 'NONE',  ( 130.8568914410475372, -24.07718906447255947, 24.07718906447199458 ) ) ;
#26009 = CARTESIAN_POINT ( 'NONE',  ( -105.3755690713226585, -41.18208027870589660, -15.38646221621809040 ) ) ;
#26010 = CARTESIAN_POINT ( 'NONE',  ( 19.06497207195981858, -39.99999999999987210, -14.19242893257882621 ) ) ;
#26011 = CARTESIAN_POINT ( 'NONE',  ( -210.0000000000000284, 0.000000000000000000, -69.99999999999998579 ) ) ;
#26012 = FACE_BOUND ( 'NONE', #13517, .T. ) ;
#26013 = CARTESIAN_POINT ( 'NONE',  ( 199.9999999999999432, -19.99999999999988987, -2.449293598294708485E-15 ) ) ;
#26014 = CARTESIAN_POINT ( 'NONE',  ( 151.7948205124836534, 23.49921654116009506, 33.06932595376371609 ) ) ;
#26015 = CARTESIAN_POINT ( 'NONE',  ( 57.59792236341148453, -37.56421063658185489, 40.00000000000002132 ) ) ;
#26016 = CARTESIAN_POINT ( 'NONE',  ( -105.2334157265395618, 2.725992507770012452, 21.31091308246880089 ) ) ;
#26017 = CARTESIAN_POINT ( 'NONE',  ( -238.4067589809705794, 39.99999999999999289, -0.9644942799821634161 ) ) ;
#26018 = CARTESIAN_POINT ( 'NONE',  ( -238.4067589809705794, 28.96627169325315165, 28.96627169325329731 ) ) ;
#26019 = CARTESIAN_POINT ( 'NONE',  ( 57.59792236341147031, -2.435789363418150000, -40.00000000000002132 ) ) ;
#26020 = ORIENTED_EDGE ( 'NONE', *, *, #10770, .F. ) ;
#26021 = CARTESIAN_POINT ( 'NONE',  ( 67.67011021022788952, -29.29769665550713498, 12.13550330104319208 ) ) ;
#26022 = AXIS2_PLACEMENT_3D ( 'NONE', #21545, #17795, #9826 ) ;
#26023 = CARTESIAN_POINT ( 'NONE',  ( -28.75791583366072146, -12.03523584680483083, 38.33181286256369447 ) ) ;
#26024 = CARTESIAN_POINT ( 'NONE',  ( 192.4448373802101173, 14.14213562370320076, -42.42640687122072762 ) ) ;
#26025 = CARTESIAN_POINT ( 'NONE',  ( -162.0762913951021176, -40.00000000000019895, 41.69427287672974813 ) ) ;
#26026 = CARTESIAN_POINT ( 'NONE',  ( 199.9999999999999432, -14.14213562373115884, 14.14213562373085153 ) ) ;
#26027 = CARTESIAN_POINT ( 'NONE',  ( 14.38125909742180752, 15.17850393972634038, 0.000000000000000000 ) ) ;
#26028 = CARTESIAN_POINT ( 'NONE',  ( 163.1118516004056573, -27.26290988616869626, -40.00000000000002132 ) ) ;
#26029 = CARTESIAN_POINT ( 'NONE',  ( 160.9163046357249129, -135.7889608577475542, 55.61140153332248559 ) ) ;
#26030 = CARTESIAN_POINT ( 'NONE',  ( 199.9999999999998579, 18.35745069958362308, -4.904641354906189576 ) ) ;
#26031 = CARTESIAN_POINT ( 'NONE',  ( 200.0000000000000000, -17.61921750228558281, -7.131901422850258854 ) ) ;
#26032 = CARTESIAN_POINT ( 'NONE',  ( -135.8532207217289738, 21.81201906317798134, -21.81201906317747685 ) ) ;
#26033 = CARTESIAN_POINT ( 'NONE',  ( 14.38125909742181996, -10.73282306405815234, -67.30136555898266693 ) ) ;
#26034 = CARTESIAN_POINT ( 'NONE',  ( -196.0240701931629417, -14.12332411430281631, 48.96019555158520831 ) ) ;
#26035 = DIRECTION ( 'NONE',  ( 1.000000000000000000, 1.836970198721030427E-16, -0.000000000000000000 ) ) ;
#26036 = CARTESIAN_POINT ( 'NONE',  ( -105.3755690713226727, -12.89780903124395550, -12.89780903124416511 ) ) ;
#26038 = DIRECTION ( 'NONE',  ( -1.000000000000000000, 0.000000000000000000, 0.000000000000000000 ) ) ;
#26037 = CARTESIAN_POINT ( 'NONE',  ( 19.06497207195982568, -38.31983398719592770, -38.31983398719660272 ) ) ;
#26039 = CARTESIAN_POINT ( 'NONE',  ( 163.1118516004056573, -47.56205970284945295, -9.006482792074823607 ) ) ;
#26040 = CARTESIAN_POINT ( 'NONE',  ( -105.4288953903231629, -9.009229104196512239, 19.35825399501247546 ) ) ;
#26041 = CARTESIAN_POINT ( 'NONE',  ( -190.0000000000000000, 61.50000000000009948, -66.50000000000005684 ) ) ;
#26043 = CARTESIAN_POINT ( 'NONE',  ( 146.6084372240433709, -39.99999999999987921, -34.62501878078319351 ) ) ;
#26042 = CARTESIAN_POINT ( 'NONE',  ( 184.8905102610680444, 13.49065550809757497, 43.07788698682593065 ) ) ;
#26044 = CARTESIAN_POINT ( 'NONE',  ( 136.1360204305621551, 24.77266263493108411, 31.79587985999273769 ) ) ;
#26045 = CARTESIAN_POINT ( 'NONE',  ( -238.4067589809705794, 28.96627169325285678, 27.60227080167094726 ) ) ;
#26046 = CARTESIAN_POINT ( 'NONE',  ( -30.26275506840324425, 41.69427246844627177, 40.00000000000002132 ) ) ;
#26047 = EDGE_LOOP ( 'NONE', ( #19262, #296, #23425, #9466 ) ) ;
#26048 = CARTESIAN_POINT ( 'NONE',  ( -105.3755690713226585, 12.89780903124410472, -43.67073346367977393 ) ) ;
#26049 = CARTESIAN_POINT ( 'NONE',  ( 96.51883974015090928, 19.13300947096759685, 7.925152011866398283 ) ) ;
#26050 = CARTESIAN_POINT ( 'NONE',  ( -612.0709805440841365, -9.999999999999969802, 1.224646799147352073E-15 ) ) ;
#26051 = CARTESIAN_POINT ( 'NONE',  ( 98.29820294267403824, -19.87244099730552094, -2.605266741664709507 ) ) ;
#26052 = ORIENTED_EDGE ( 'NONE', *, *, #3424, .T. ) ;
#26053 = CARTESIAN_POINT ( 'NONE',  ( -197.4154352059224493, -49.11380478891992141, 14.14666496776951377 ) ) ;
#26054 = CARTESIAN_POINT ( 'NONE',  ( -716.9846540392142060, -66.50000000000001421, -61.50000000000006395 ) ) ;
#26055 = CARTESIAN_POINT ( 'NONE',  ( 17.49521241104683966, -18.35049639064382276, 44.30201726249271843 ) ) ;
#26056 = CARTESIAN_POINT ( 'NONE',  ( 23.39921416754926753, 23.33452606844902988, -42.84940400815654726 ) ) ;
#26057 = CARTESIAN_POINT ( 'NONE',  ( 199.0074854128475579, 2.768696461275208520, -19.80384161416936806 ) ) ;
#26058 = DIRECTION ( 'NONE',  ( -1.000000000000000000, -1.836970198721030181E-16, -0.000000000000000000 ) ) ;
#26059 = FACE_OUTER_BOUND ( 'NONE', #11463, .T. ) ;
#26060 = EDGE_CURVE ( 'NONE', #4428, #21267, #8647, .T. ) ;
#26061 = CARTESIAN_POINT ( 'NONE',  ( -105.3755690713226585, -15.38646221621738164, -41.18208027870615240 ) ) ;
#26062 = CARTESIAN_POINT ( 'NONE',  ( -280.0000000000000568, 19.99999999999996092, 40.00000000000002132 ) ) ;
#26064 = CARTESIAN_POINT ( 'NONE',  ( -259.2033419157646676, -9.517827891722680178, 0.000000000000000000 ) ) ;
#26063 = CARTESIAN_POINT ( 'NONE',  ( 44.46627453556679654, -15.24062802624899504, -36.79413088011303046 ) ) ;
#26065 = EDGE_CURVE ( 'NONE', #17669, #5443, #22967, .T. ) ;
#26066 = CARTESIAN_POINT ( 'NONE',  ( 91.82158438592158234, 17.20528682183301683, 0.000000000000000000 ) ) ;
#26067 = CARTESIAN_POINT ( 'NONE',  ( -100.7734535825088500, 22.67402823373189591, -0.000000000000000000 ) ) ;
#26068 = CARTESIAN_POINT ( 'NONE',  ( 192.4448373802101173, -20.00000000003938538, 40.00000000000002132 ) ) ;
#26069 = CARTESIAN_POINT ( 'NONE',  ( -56.48582580120558561, 3.151766524733697544E-13, -30.84685318188644132 ) ) ;
#26070 = DIRECTION ( 'NONE',  ( 1.836970198721030427E-16, -1.000000000000000000, 4.182618615277681568E-16 ) ) ;
#26071 = CARTESIAN_POINT ( 'NONE',  ( -56.48582580120559271, 6.472252184284121412, 6.472252184284244869 ) ) ;
#26072 = EDGE_CURVE ( 'NONE', #3167, #7987, #21676, .T. ) ;
#26073 = EDGE_CURVE ( 'NONE', #7090, #16387, #24196, .T. ) ;
#26074 = VERTEX_POINT ( 'NONE', #15666 ) ;
#26075 = CARTESIAN_POINT ( 'NONE',  ( -65.65550967526021964, -24.89650881518424796, 9.107276986624334825 ) ) ;
#26076 = CARTESIAN_POINT ( 'NONE',  ( 163.1118516004056573, 27.26290988616876021, 40.00000000000002132 ) ) ;
#26077 = CARTESIAN_POINT ( 'NONE',  ( -77.90255099906863734, -20.04994828524331396, -8.644468104250957907 ) ) ;
#26078 = PRODUCT_CONTEXT ( 'NONE', #19110, 'mechanical' ) ;
#26079 = ORIENTED_EDGE ( 'NONE', *, *, #25887, .T. ) ;
#26080 = MANIFOLD_SOLID_BREP ( 'Chamfer3', #4528 ) ;
#26081 = ORIENTED_EDGE ( 'NONE', *, *, #26327, .T. ) ;
#26082 = CARTESIAN_POINT ( 'NONE',  ( -56.48582580120558561, -50.09629031063963112, -6.472252184284449150 ) ) ;
#26083 = CARTESIAN_POINT ( 'NONE',  ( 23.72853009152626669, -42.74808902029896984, -23.26754081577798416 ) ) ;
#26084 = ORIENTED_EDGE ( 'NONE', *, *, #13844, .T. ) ;
#26085 = CARTESIAN_POINT ( 'NONE',  ( -238.4067589809705794, 0.9644942799825385604, -40.00000000000002132 ) ) ;
#26086 = CARTESIAN_POINT ( 'NONE',  ( -97.73806390046078718, -20.71810467719840076, 8.581719943915564031 ) ) ;
#26087 = ORIENTED_EDGE ( 'NONE', *, *, #6380, .F. ) ;
#26088 = CARTESIAN_POINT ( 'NONE',  ( 200.0000000000001421, 9.088304224312857116, 16.69380151103622012 ) ) ;
#26089 = CARTESIAN_POINT ( 'NONE',  ( -726.9846540392142060, -66.50000000000001421, -66.50000000000005684 ) ) ;
#26090 = CARTESIAN_POINT ( 'NONE',  ( -208.1127848780264742, 38.89260858015732936, -17.67593391476642140 ) ) ;
#26091 = CARTESIAN_POINT ( 'NONE',  ( -129.2303573022218472, -25.82247248374897453, -9.309001178860381032 ) ) ;
#26092 =( BOUNDED_SURFACE ( )  B_SPLINE_SURFACE ( 3, 2, ( 
 ( #13281, #3176, #1054 ),
 ( #23647, #9289, #21528 ),
 ( #15018, #15146, #23148 ),
 ( #25277, #19144, #928 ),
 ( #17272, #9038, #9414 ),
 ( #7027, #23276, #9159 ),
 ( #3303, #17521, #7157 ),
 ( #11281, #15910, #15648 ),
 ( #13923, #11658, #3970 ),
 ( #7935, #6086, #3692 ),
 ( #19918, #12067, #8069 ),
 ( #22193, #7664, #10074 ),
 ( #11798, #19782, #25923 ),
 ( #26198, #18179, #23904 ),
 ( #26056, #1568, #13659 ),
 ( #18045, #1836, #7794 ),
 ( #1702, #9937, #5820 ),
 ( #14062, #16053, #14193 ),
 ( #1969, #4100, #24178 ),
 ( #25786, #21782, #3555 ),
 ( #26328, #15775, #24042 ),
 ( #22325, #20185, #16188 ),
 ( #17913, #9673, #22058 ),
 ( #5680, #12201, #24321 ),
 ( #17777, #20322, #5550 ),
 ( #13785, #3831, #5953 ),
 ( #21920, #9536, #9809 ),
 ( #11932, #20059, #17645 ),
 ( #7536, #23773, #24718 ),
 ( #2359, #8467, #16321 ),
 ( #14459, #16856, #4627 ),
 ( #4492, #8203, #6214 ),
 ( #12594, #24987, #22715 ),
 ( #4367, #4762, #16586 ),
 ( #10338, #14326, #18852 ),
 ( #10472, #24448, #12730 ),
 ( #95, #22458, #6738 ),
 ( #20724, #8607, #223 ),
 ( #364, #16459, #24848 ),
 ( #14850, #24581, #16716 ),
 ( #12328, #2632, #18447 ),
 ( #8337, #22590, #22986 ),
 ( #12866, #18313, #6473 ),
 ( #6337, #4238, #8738 ),
 ( #6600, #20456, #2099 ),
 ( #2230, #14587, #12457 ),
 ( #632, #20584, #18587 ),
 ( #20852, #10208, #2492 ),
 ( #10603, #18715, #500 ),
 ( #14720, #22852, #10741 ),
 ( #766, #11371, #25378 ),
 ( #7253, #8872, #17490 ),
 ( #15372, #6870, #23373 ),
 ( #19492, #9383, #25632 ),
 ( #19114, #21502, #23495 ),
 ( #23118, #11004, #14984 ),
 ( #3273, #9007, #18988 ),
 ( #13000, #25118, #9260 ),
 ( #13254, #19243, #21377 ),
 ( #3147, #17240, #17114 ) ),
 .UNSPECIFIED., .F., .F., .F. ) 
 B_SPLINE_SURFACE_WITH_KNOTS ( ( 4, 2, 2, 2, 2, 2, 2, 2, 2, 2, 2, 2, 2, 2, 2, 2, 2, 2, 2, 2, 2, 2, 2, 2, 2, 2, 2, 2, 2, 4 ),
 ( 3, 3 ),
 ( -6.934549977324636831E-05, 0.02465257023823466329, 0.04937448597624257557, 0.07409640171425048438, 0.08027688064875246332, 0.08066316058215883267, 0.08085630054886201734, 0.08090458554053781004, 0.08095287053221361662, 0.08104944051556520201, 0.08182200038237795459, 0.08336712011600344585, 0.08645735958325444226, 0.09263783851775642120, 0.09881831745225840014, 0.1019085569195093965, 0.1049987963867603791, 0.1111792753212623441, 0.1173597542557643231, 0.1177460341891707063, 0.1179391741558738910, 0.1179874591475496837, 0.1180357441392254902, 0.1181323141225770756, 0.1189048739893898143, 0.1204499937230153195, 0.1235402331902663020, 0.1482621489282742178, 0.1729840646662821335, 0.1977059804042900493 ),
 ( 0.000000000000000000, 1.000000000000000000 ),
 .UNSPECIFIED. ) 
 GEOMETRIC_REPRESENTATION_ITEM ( )  RATIONAL_B_SPLINE_SURFACE ( (
 ( 1.000000000000000000, 1.000000000000000000, 1.000000000000000000),
 ( 1.000000000000000000, 0.9999975583951711267, 1.000000000000000000),
 ( 1.000000000000000000, 0.9982436956960244467, 1.000000000000000000),
 ( 1.000000000000000000, 0.9910288481552836926, 1.000000000000000000),
 ( 1.000000000000000000, 0.9855714588515669394, 1.000000000000000000),
 ( 1.000000000000000000, 0.9705958323316277170, 1.000000000000000000),
 ( 1.000000000000000000, 0.9610788543728805422, 1.000000000000000000),
 ( 1.000000000000000000, 0.9462867046313790942, 1.000000000000000000),
 ( 1.000000000000000000, 0.9431828180754202595, 1.000000000000000000),
 ( 1.000000000000000000, 0.9397240291170393389, 1.000000000000000000),
 ( 1.000000000000000000, 0.9395199791395948408, 1.000000000000000000),
 ( 1.000000000000000000, 0.9392130141387217135, 1.000000000000000000),
 ( 1.000000000000000000, 0.9391105441325077186, 1.000000000000000000),
 ( 1.000000000000000000, 0.9389822709566318926, 1.000000000000000000),
 ( 1.000000000000000000, 0.9389566070380594986, 1.000000000000000000),
 ( 1.000000000000000000, 0.9389052606279759683, 1.000000000000000000),
 ( 1.000000000000000000, 0.9388799835492042112, 1.000000000000000000),
 ( 1.000000000000000000, 0.9388039637710107188, 1.000000000000000000),
 ( 1.000000000000000000, 0.9387533729070498545, 1.000000000000000000),
 ( 1.000000000000000000, 0.9382988607466662412, 1.000000000000000000),
 ( 1.000000000000000000, 0.9379005790853373048, 1.000000000000000000),
 ( 1.000000000000000000, 0.9367237203701870296, 1.000000000000000000),
 ( 1.000000000000000000, 0.9359625442025352182, 1.000000000000000000),
 ( 1.000000000000000000, 0.9337619511410462092, 1.000000000000000000),
 ( 1.000000000000000000, 0.9324064515426850885, 1.000000000000000000),
 ( 1.000000000000000000, 0.9287106072119778455, 1.000000000000000000),
 ( 1.000000000000000000, 0.9267422912949104807, 1.000000000000000000),
 ( 1.000000000000000000, 0.9239539123017169731, 1.000000000000000000),
 ( 1.000000000000000000, 0.9231338493907679243, 1.000000000000000000),
 ( 1.000000000000000000, 0.9228496048507219829, 1.000000000000000000),
 ( 1.000000000000000000, 0.9229135694614544194, 1.000000000000000000),
 ( 1.000000000000000000, 0.9233494155302709450, 1.000000000000000000),
 ( 1.000000000000000000, 0.9237209353787055877, 1.000000000000000000),
 ( 1.000000000000000000, 0.9252744993866384160, 1.000000000000000000),
 ( 1.000000000000000000, 0.9268968421606754715, 1.000000000000000000),
 ( 1.000000000000000000, 0.9311673748451266830, 1.000000000000000000),
 ( 1.000000000000000000, 0.9338157035271601458, 1.000000000000000000),
 ( 1.000000000000000000, 0.9370733336298897598, 1.000000000000000000),
 ( 1.000000000000000000, 0.9372665829346482624, 1.000000000000000000),
 ( 1.000000000000000000, 0.9375588533504889410, 1.000000000000000000),
 ( 1.000000000000000000, 0.9376566762263730537, 1.000000000000000000),
 ( 1.000000000000000000, 0.9377794499114625593, 1.000000000000000000),
 ( 1.000000000000000000, 0.9378038842964711019, 1.000000000000000000),
 ( 1.000000000000000000, 0.9378536652368905102, 1.000000000000000000),
 ( 1.000000000000000000, 0.9378785472098797316, 1.000000000000000000),
 ( 1.000000000000000000, 0.9379531676447510069, 1.000000000000000000),
 ( 1.000000000000000000, 0.9380028806225376714, 1.000000000000000000),
 ( 1.000000000000000000, 0.9384499917948705416, 1.000000000000000000),
 ( 1.000000000000000000, 0.9388452506063379444, 1.000000000000000000),
 ( 1.000000000000000000, 0.9400245377241723821, 1.000000000000000000),
 ( 1.000000000000000000, 0.9408020798629984638, 1.000000000000000000),
 ( 1.000000000000000000, 0.9431089717073131151, 1.000000000000000000),
 ( 1.000000000000000000, 0.9446123105951671484, 1.000000000000000000),
 ( 1.000000000000000000, 0.9578370004747042143, 1.000000000000000000),
 ( 1.000000000000000000, 0.9674308273343070752, 1.000000000000000000),
 ( 1.000000000000000000, 0.9828254127557658482, 1.000000000000000000),
 ( 1.000000000000000000, 0.9886239107116221447, 1.000000000000000000),
 ( 1.000000000000000000, 0.9967564037645806341, 1.000000000000000000),
 ( 1.000000000000000000, 0.9990872413561198151, 1.000000000000000000),
 ( 1.000000000000000000, 0.9997813423572990965, 1.000000000000000000) ) ) 
 REPRESENTATION_ITEM ( '' )  SURFACE ( )  );
#26093 = CARTESIAN_POINT ( 'NONE',  ( 91.82158438592159655, -39.99999999999994316, -17.20528682183314118 ) ) ;
#26094 = CARTESIAN_POINT ( 'NONE',  ( -135.8532207217289738, 30.84685318188643421, 40.00000000000002132 ) ) ;
#26095 = CARTESIAN_POINT ( 'NONE',  ( -213.1075012329537230, 37.98287015391280619, -37.98287015391192512 ) ) ;
#26096 = DIRECTION ( 'NONE',  ( 0.000000000000000000, 1.000000000000000000, 0.000000000000000000 ) ) ;
#26097 = CARTESIAN_POINT ( 'NONE',  ( -86.96347745069643054, -39.99999999999995737, -21.75974354311664527 ) ) ;
#26098 = CARTESIAN_POINT ( 'NONE',  ( -56.48582580120557850, -39.99999999999970868, -30.84685318188687120 ) ) ;
#26099 = CARTESIAN_POINT ( 'NONE',  ( 170.0000000000000000, 1.183443619805854272E-13, -24.95097643317000546 ) ) ;
#26100 = CARTESIAN_POINT ( 'NONE',  ( -162.0762913951020607, -1.198031840455708430, 57.76657433537920383 ) ) ;
#26101 = CARTESIAN_POINT ( 'NONE',  ( -135.8532207217289738, 9.153146818113546246, -0.000000000000000000 ) ) ;
#26102 = CARTESIAN_POINT ( 'NONE',  ( -238.4067589809705794, -28.96627169325343942, 28.96627169325309126 ) ) ;
#26103 = PLANE ( 'NONE',  #18555 ) ;
#26104 = CARTESIAN_POINT ( 'NONE',  ( 12.01676479903286676, -49.30523874212533286, 14.17570730777206833 ) ) ;
#26105 = CARTESIAN_POINT ( 'NONE',  ( 98.29820294273055481, 14.14213562373424971, 14.14213562373465294 ) ) ;
#26106 = CARTESIAN_POINT ( 'NONE',  ( 163.1118516004056573, 1.251511021549353291E-13, -27.26290988616872824 ) ) ;
#26107 = CARTESIAN_POINT ( 'NONE',  ( -100.7734535825088500, 12.25131212657490209, -44.31723036834897300 ) ) ;
#26108 = CARTESIAN_POINT ( 'NONE',  ( 199.9999999999999432, 14.14213562373093680, 14.14213562373114641 ) ) ;
#26109 = CARTESIAN_POINT ( 'NONE',  ( -188.4265466358192214, -13.83489705870103137, -47.03621809928373665 ) ) ;
#26110 = CARTESIAN_POINT ( 'NONE',  ( -190.0000000000000000, -71.50000000000002842, -66.50000000000005684 ) ) ;
#26111 = EDGE_LOOP ( 'NONE', ( #17305, #21850, #8532, #9901 ) ) ;
#26112 = CARTESIAN_POINT ( 'NONE',  ( 57.59792236341147031, -30.00663442387662627, -26.56190807104723461 ) ) ;
#26113 = CARTESIAN_POINT ( 'NONE',  ( 136.1360204305621266, 53.05693388239316022, 3.511608612530967566 ) ) ;
#26114 = CARTESIAN_POINT ( 'NONE',  ( -198.0356074513804572, -15.37879056873074290, 0.000000000000000000 ) ) ;
#26115 = FACE_OUTER_BOUND ( 'NONE', #4459, .T. ) ;
#26116 = CARTESIAN_POINT ( 'NONE',  ( -86.96347745069644475, -43.67073346367964604, -12.89780903124457545 ) ) ;
#26117 = CARTESIAN_POINT ( 'NONE',  ( -197.4153392274985492, -24.72549520219616781, -44.73189834453274472 ) ) ;
#26118 = ORIENTED_EDGE ( 'NONE', *, *, #21119, .T. ) ;
#26119 = CARTESIAN_POINT ( 'NONE',  ( 199.9999999999999432, 18.94174490274730616, -1.534455786497347596 ) ) ;
#26120 = CARTESIAN_POINT ( 'NONE',  ( -370.0000000000001137, -4.734761052820324085E-14, -10.00000000000004796 ) ) ;
#26121 = CARTESIAN_POINT ( 'NONE',  ( -4.082462733456094561, 13.82507958736525921, 46.97557262069152273 ) ) ;
#26122 = VERTEX_POINT ( 'NONE', #23298 ) ;
#26123 = ORIENTED_EDGE ( 'NONE', *, *, #22018, .F. ) ;
#26124 = CARTESIAN_POINT ( 'NONE',  ( -105.3755690713226727, -21.75974354311652093, 0.000000000000000000 ) ) ;
#26125 = CARTESIAN_POINT ( 'NONE',  ( 199.0125641721520822, -8.847877585088737007, -17.93749959268865979 ) ) ;
#26126 = CARTESIAN_POINT ( 'NONE',  ( -114.4364955367317549, 8.064892380853404319, 20.29001642038314657 ) ) ;
#26127 = CARTESIAN_POINT ( 'NONE',  ( 73.43468571101038833, 9.843145813772503416, -28.18272067128102520 ) ) ;
#26128 = MANIFOLD_SOLID_BREP ( 'Cut-Extrude5', #24044 ) ;
#26129 = CARTESIAN_POINT ( 'NONE',  ( -265.0000000000000000, -4.857225732735059864E-14, 0.000000000000000000 ) ) ;
#26130 = CARTESIAN_POINT ( 'NONE',  ( -198.0356074513804572, 1.247057299367198800E-13, -15.37879056873070560 ) ) ;
#26131 = CARTESIAN_POINT ( 'NONE',  ( -280.0000000000000000, -2.609240458947769655E-13, 20.00000000000001421 ) ) ;
#26132 = CARTESIAN_POINT ( 'NONE',  ( -626.9846540392142060, 95.00000000000000000, -30.00000000000005684 ) ) ;
#26133 = DIRECTION ( 'NONE',  ( 1.000000000000000000, 0.000000000000000000, 0.000000000000000000 ) ) ;
#26134 = CARTESIAN_POINT ( 'NONE',  ( 199.0132385929227610, 17.30986399168244461, 10.02103235953326710 ) ) ;
#26135 = CARTESIAN_POINT ( 'NONE',  ( -151.4802849341772628, 16.17241510384845782, 31.86309571750582137 ) ) ;
#26136 = CARTESIAN_POINT ( 'NONE',  ( 8.209392600897984948, -14.17653494425323224, -49.31072049265799961 ) ) ;
#26137 = CARTESIAN_POINT ( 'NONE',  ( 163.1118516004056573, -9.006482792069506971, -9.006482792069697041 ) ) ;
#26138 = CARTESIAN_POINT ( 'NONE',  ( -110.1017833366333463, 1.261429655903683500, -20.19517362625915524 ) ) ;
#26139 = CARTESIAN_POINT ( 'NONE',  ( 91.82158438592159655, -44.40256751092324095, -12.16597498400075139 ) ) ;
#26140 = CARTESIAN_POINT ( 'NONE',  ( 136.1360204305621266, -3.419521671106983309E-13, 35.03383547441296741 ) ) ;
#26141 = CARTESIAN_POINT ( 'NONE',  ( -162.0762913951020892, -1.198031840385767266, -1.198031840385758384 ) ) ;
#26142 = CARTESIAN_POINT ( 'NONE',  ( 19.06497207195982924, -54.19242893257843008, 40.00000000000002132 ) ) ;
#26143 = CARTESIAN_POINT ( 'NONE',  ( 107.5473083967384298, 16.96446921415044784, -16.96446921415024889 ) ) ;
#26144 = B_SPLINE_CURVE_WITH_KNOTS ( 'NONE', 3,
 ( #20121, #24381, #2035, #21986, #1899, #10004, #25990, #19981 ),
 .UNSPECIFIED., .F., .F.,
 ( 4, 2, 2, 4 ),
 ( 0.0002282271114689535154, 0.004312393619941001614, 0.006354476874177026301, 0.008396560128413051854 ),
 .UNSPECIFIED. ) ;
#26145 = CARTESIAN_POINT ( 'NONE',  ( 4.995406935893307754, -55.24977328854835434, -2.449293598294708485E-15 ) ) ;
#26146 = CARTESIAN_POINT ( 'NONE',  ( -114.7469097549961674, 17.41872337029852602, 13.60512637059788155 ) ) ;
#26147 = EDGE_CURVE ( 'NONE', #10974, #16948, #2631, .T. ) ;
#26148 = CARTESIAN_POINT ( 'NONE',  ( 14.38125909742180930, 40.00000000000060396, -55.17850393974224232 ) ) ;
#26149 = CARTESIAN_POINT ( 'NONE',  ( -192.9588430854689989, 10.23066800230742679, 10.23066800230749607 ) ) ;
#26150 = CARTESIAN_POINT ( 'NONE',  ( 163.1118516004056573, 12.73709011382478806, -40.00000000000002132 ) ) ;
#26151 = VERTEX_POINT ( 'NONE', #17166 ) ;
#26152 = CARTESIAN_POINT ( 'NONE',  ( 23.40652632868000538, -46.79646383233843920, 13.79856377312506055 ) ) ;
#26153 = AXIS2_PLACEMENT_3D ( 'NONE', #15296, #23669, #17542 ) ;
#26154 = CARTESIAN_POINT ( 'NONE',  ( 141.7948666911896112, 12.58737617328871572, 30.38861427224642853 ) ) ;
#26155 = CARTESIAN_POINT ( 'NONE',  ( 0.2972598230769886718, 38.42060263243669027, -18.14793986248710667 ) ) ;
#26156 = CIRCLE ( 'NONE', #14668, 10.00000000000000000 ) ;
#26157 = CARTESIAN_POINT ( 'NONE',  ( 19.06497207195982924, -40.00000000000021316, 54.19242893257830218 ) ) ;
#26158 = AXIS2_PLACEMENT_3D ( 'NONE', #15252, #13261, #17498 ) ;
#26159 = CARTESIAN_POINT ( 'NONE',  ( -280.0000000000000568, 14.14213562373038968, 42.42640687119305198 ) ) ;
#26160 = CARTESIAN_POINT ( 'NONE',  ( -86.96347745069644475, -21.75974354311651737, 0.000000000000000000 ) ) ;
#26161 = EDGE_CURVE ( 'NONE', #21338, #13305, #1349, .T. ) ;
#26162 = CARTESIAN_POINT ( 'NONE',  ( -56.48582580120559271, -9.153146818113595984, 0.000000000000000000 ) ) ;
#26163 = DIRECTION ( 'NONE',  ( 0.000000000000000000, 1.000000000000000000, 0.000000000000000000 ) ) ;
#26164 = CARTESIAN_POINT ( 'NONE',  ( 199.9999999999999432, 14.48708306876533136, 12.30466461812483914 ) ) ;
#26165 = ADVANCED_FACE ( 'NONE', ( #1589 ), #15069, .T. ) ;
#26166 = CARTESIAN_POINT ( 'NONE',  ( 199.9999999999999716, -18.97839083694794837, 1.248491631922335143 ) ) ;
#26167 = CARTESIAN_POINT ( 'NONE',  ( 146.6084372240433709, 32.08495691632030145, 24.48358557860365181 ) ) ;
#26168 = CARTESIAN_POINT ( 'NONE',  ( -135.8532207217289738, -50.09629031063973770, 6.472252184283735943 ) ) ;
#26169 = CARTESIAN_POINT ( 'NONE',  ( 146.6084372240433993, 24.48358557860341733, -24.48358557860313311 ) ) ;
#26170 = CARTESIAN_POINT ( 'NONE',  ( -82.27051431265631720, 17.53273480389332306, -9.999544339261095871 ) ) ;
#26171 = CARTESIAN_POINT ( 'NONE',  ( 136.1360204305621266, -3.511608612531119000, 53.05693388239312469 ) ) ;
#26173 = LINE ( 'NONE', #20435, #4089 ) ;
#26172 = CARTESIAN_POINT ( 'NONE',  ( 170.2234770963711128, -10.92277846919187034, -10.92277846919209594 ) ) ;
#26174 = CARTESIAN_POINT ( 'NONE',  ( -56.48582580120559271, -6.472252184284276844, 6.472252184284108978 ) ) ;
#26175 = CARTESIAN_POINT ( 'NONE',  ( -105.4741150117390021, -8.366608964578313490, 19.60045294983322961 ) ) ;
#26176 = CARTESIAN_POINT ( 'NONE',  ( 199.0229061757917464, 1.171229046118675177, 19.97135794441219048 ) ) ;
#26177 = EDGE_CURVE ( 'NONE', #1760, #567, #12555, .T. ) ;
#26179 = CARTESIAN_POINT ( 'NONE',  ( -280.0000000000000568, -40.00000000000000000, -20.00000000000015277 ) ) ;
#26178 = CARTESIAN_POINT ( 'NONE',  ( -86.96347745069644475, -15.38646221621738164, -41.18208027870615240 ) ) ;
#26180 = CARTESIAN_POINT ( 'NONE',  ( 170.2234770963711128, 45.64576402573181468, 10.92277846919223627 ) ) ;
#26181 = CIRCLE ( 'NONE', #15519, 14.99999999999999645 ) ;
#26182 = CARTESIAN_POINT ( 'NONE',  ( -56.48582580120559271, -6.472252184284276844, 6.472252184284108978 ) ) ;
#26183 = AXIS2_PLACEMENT_3D ( 'NONE', #21411, #13290, #19659 ) ;
#26184 = CARTESIAN_POINT ( 'NONE',  ( -4.201409602818355182, 42.95750343186458764, -23.41774994521173170 ) ) ;
#26185 = CARTESIAN_POINT ( 'NONE',  ( -100.7734535825088500, -22.67402823373193499, 40.00000000000002132 ) ) ;
#26186 = ORIENTED_EDGE ( 'NONE', *, *, #12200, .T. ) ;
#26187 = CARTESIAN_POINT ( 'NONE',  ( -1.821043593238323544, -23.89737153267490655, -43.61003463695192295 ) ) ;
#26188 = CARTESIAN_POINT ( 'NONE',  ( 47.87955150251453063, 35.38323854600922402, 14.65621728643953148 ) ) ;
#26189 = DIRECTION ( 'NONE',  ( -1.000000000000000000, -0.000000000000000000, -0.000000000000000000 ) ) ;
#26190 =( REPRESENTATION_RELATIONSHIP ('NONE','NONE', #23888, #9131 ) REPRESENTATION_RELATIONSHIP_WITH_TRANSFORMATION ( #12890 )SHAPE_REPRESENTATION_RELATIONSHIP( ) );
#26191 = CARTESIAN_POINT ( 'NONE',  ( -280.0000000000000000, -20.00000000000006750, 0.000000000000000000 ) ) ;
#26192 = VECTOR ( 'NONE', #23062, 1000.000000000000000 ) ;
#26193 = ORIENTED_EDGE ( 'NONE', *, *, #24685, .F. ) ;
#26194 = CARTESIAN_POINT ( 'NONE',  ( -188.6013476421507278, -47.09841799633881010, 13.84412643132970189 ) ) ;
#26195 = CARTESIAN_POINT ( 'NONE',  ( 199.9999999999998295, -17.79330310134281135, 6.698924172861754123 ) ) ;
#26196 = VECTOR ( 'NONE', #10994, 1000.000000000000000 ) ;
#26197 = CARTESIAN_POINT ( 'NONE',  ( 13.08024833506956064, -18.54957993049078979, 44.78264744452992829 ) ) ;
#26198 = CARTESIAN_POINT ( 'NONE',  ( 23.41418334855310945, 23.33148157649319288, -42.84479974151748394 ) ) ;
#26199 = CARTESIAN_POINT ( 'NONE',  ( 199.0142478014330720, -11.65985798941387941, -16.24932773989132073 ) ) ;
#26200 = CIRCLE ( 'NONE', #20242, 14.99999999999999645 ) ;
#26201 = CARTESIAN_POINT ( 'NONE',  ( 130.8888609958233928, -29.49786752803548495, 12.21841679119701851 ) ) ;
#26202 = CARTESIAN_POINT ( 'NONE',  ( 57.59792236341147031, 1.908507979671054758E-14, -2.435789363418160658 ) ) ;
#26203 = CARTESIAN_POINT ( 'NONE',  ( -86.96347745069644475, 41.18208027870576871, 15.38646221621837107 ) ) ;
#26204 = DIRECTION ( 'NONE',  ( 0.000000000000000000, -1.000000000000000000, 0.000000000000000000 ) ) ;
#26206 = CARTESIAN_POINT ( 'NONE',  ( 184.8905102610680444, 13.49065550809757497, 43.07788698682593065 ) ) ;
#26205 = CARTESIAN_POINT ( 'NONE',  ( -189.1288815661392562, 23.62384257861526038, -43.24061771115778186 ) ) ;
#26207 = DIRECTION ( 'NONE',  ( 0.000000000000000000, 0.000000000000000000, -1.000000000000000000 ) ) ;
#26208 = CARTESIAN_POINT ( 'NONE',  ( 170.2234770963711128, 24.55285855007190676, -40.00000000000002132 ) ) ;
#26209 = CARTESIAN_POINT ( 'NONE',  ( 4.995406935893288214, 15.24977328854832770, 0.000000000000000000 ) ) ;
#26210 = CARTESIAN_POINT ( 'NONE',  ( -192.9588430854690273, -39.99999999999948841, -54.46834944098263520 ) ) ;
#26211 = CARTESIAN_POINT ( 'NONE',  ( 199.9999999999999432, 14.14213562373090838, 14.14213562373092437 ) ) ;
#26212 = CARTESIAN_POINT ( 'NONE',  ( -105.3755690713226727, -2.472783935621397949E-13, 21.75974354311649961 ) ) ;
#26213 = CARTESIAN_POINT ( 'NONE',  ( 130.8568914410475372, 24.07718906447210472, 24.07718906447249907 ) ) ;
#26214 = ORIENTED_EDGE ( 'NONE', *, *, #3626, .F. ) ;
#26215 = CARTESIAN_POINT ( 'NONE',  ( 0.2972598230769990524, -18.14793986248724522, 38.42060263243662632 ) ) ;
#26216 = CARTESIAN_POINT ( 'NONE',  ( -192.9588430854689989, -14.46834944099973086, 0.000000000000000000 ) ) ;
#26217 = CARTESIAN_POINT ( 'NONE',  ( -190.0000000000000000, -61.50000000000001421, 66.50000000000005684 ) ) ;
#26218 = APPLICATION_PROTOCOL_DEFINITION ( 'draft international standard', 'automotive_design', 1998, #17997 ) ;
#26219 = ORIENTED_EDGE ( 'NONE', *, *, #4923, .F. ) ;
#26220 = ORIENTED_EDGE ( 'NONE', *, *, #16965, .F. ) ;
#26221 = CARTESIAN_POINT ( 'NONE',  ( 199.9999999999999432, 14.14213562373113398, -14.14213562373094923 ) ) ;
#26222 = CARTESIAN_POINT ( 'NONE',  ( 22.76838195347375304, -43.17632592580142870, -17.88421977190818168 ) ) ;
#26223 = EDGE_LOOP ( 'NONE', ( #2544, #17909, #16942, #10306, #13807, #9564 ) ) ;
#26224 = CARTESIAN_POINT ( 'NONE',  ( 146.6084372240433709, 5.374981219217002781, -40.00000000000002132 ) ) ;
#26225 = LINE ( 'NONE', #9968, #3669 ) ;
#26226 = EDGE_CURVE ( 'NONE', #11892, #17137, #19070, .T. ) ;
#26227 = ORIENTED_EDGE ( 'NONE', *, *, #20292, .F. ) ;
#26228 = CARTESIAN_POINT ( 'NONE',  ( 199.9999999999998579, 13.31531350134012648, 13.56203446005050317 ) ) ;
#26229 = DIRECTION ( 'NONE',  ( -1.000000000000000000, -0.000000000000000000, -0.000000000000000000 ) ) ;
#26230 = CARTESIAN_POINT ( 'NONE',  ( 192.4448373802101173, 14.14213562370320076, -42.42640687122072762 ) ) ;
#26231 = EDGE_CURVE ( 'NONE', #122, #5454, #8298, .T. ) ;
#26232 = CARTESIAN_POINT ( 'NONE',  ( -174.2682069750611902, -39.26787081113005939, -16.26528465560755876 ) ) ;
#26233 = CARTESIAN_POINT ( 'NONE',  ( -213.1075012329537230, -40.00000000000025580, 53.71589010953650956 ) ) ;
#26234 = CARTESIAN_POINT ( 'NONE',  ( 163.1118516004056573, -27.26290988616869626, 40.00000000000002132 ) ) ;
#26235 = CARTESIAN_POINT ( 'NONE',  ( -105.3755690713226727, 12.89780903124418998, -12.89780903124389155 ) ) ;
#26236 = CARTESIAN_POINT ( 'NONE',  ( 199.0261090282319856, -10.57113834583376644, 16.98461103275367634 ) ) ;
#26237 = EDGE_CURVE ( 'NONE', #11587, #961, #18153, .T. ) ;
#26238 = CARTESIAN_POINT ( 'NONE',  ( -213.1075012329537230, -40.00000000000011369, 13.71589010951897691 ) ) ;
#26239 = CARTESIAN_POINT ( 'NONE',  ( 14.38125909742181818, -39.99999999999986500, -15.17850393972675604 ) ) ;
#26240 = CARTESIAN_POINT ( 'NONE',  ( -105.3394646353678041, -10.54672847193054075, 18.62482576794085887 ) ) ;
#26241 = CARTESIAN_POINT ( 'NONE',  ( -198.0356074513804288, -39.15871834505936278, 39.15871834505892224 ) ) ;
#26242 = CARTESIAN_POINT ( 'NONE',  ( -208.1127848780264742, -15.00245453012673202, -40.00000000000002132 ) ) ;
#26243 = CARTESIAN_POINT ( 'NONE',  ( 136.1360204305621551, -31.79587985999244282, -24.77266263493140386 ) ) ;
#26244 = CARTESIAN_POINT ( 'NONE',  ( -105.4741150117390021, -8.366608964578313490, 19.60045294983322961 ) ) ;
#26245 = CYLINDRICAL_SURFACE ( 'NONE', #6411, 4.999999999999997335 ) ;
#26246 = CARTESIAN_POINT ( 'NONE',  ( 107.5473083967699068, 16.96446921415981635, 16.96446921416008990 ) ) ;
#26247 = CARTESIAN_POINT ( 'NONE',  ( -238.4067589809705794, -4.716212492215116094E-14, 0.9644942799825824142 ) ) ;
#26248 = CARTESIAN_POINT ( 'NONE',  ( 14.38125909742180220, 39.01709431150916885, -17.55144818341463164 ) ) ;
#26249 = CARTESIAN_POINT ( 'NONE',  ( 163.1118516004056573, 19.27778845538753316, 19.27778845538783870 ) ) ;
#26250 = CARTESIAN_POINT ( 'NONE',  ( -188.6890294954627620, -13.84869711777154855, -47.12920239600004635 ) ) ;
#26251 = CARTESIAN_POINT ( 'NONE',  ( 165.3321726438082351, -2.475684083387132530E-13, 26.53500608755492252 ) ) ;
#26252 = ORIENTED_EDGE ( 'NONE', *, *, #20692, .T. ) ;
#26253 = CARTESIAN_POINT ( 'NONE',  ( 170.2234770963711128, -17.36149277826940462, -39.20704971665412586 ) ) ;
#26254 = CARTESIAN_POINT ( 'NONE',  ( 98.29820294267493352, -20.00000000000511235, 5.223721743777709619E-12 ) ) ;
#26255 = CARTESIAN_POINT ( 'NONE',  ( 130.8568914410475372, 34.05028731879791337, 0.000000000000000000 ) ) ;
#26256 = CARTESIAN_POINT ( 'NONE',  ( -87.13361725327074225, -15.19799821270821560, -15.19799821270861884 ) ) ;
#26257 = CARTESIAN_POINT ( 'NONE',  ( -259.2033419157646676, -35.01439189186523748, -21.55415060305881170 ) ) ;
#26258 = DIRECTION ( 'NONE',  ( 0.000000000000000000, -1.000000000000000000, 0.000000000000000000 ) ) ;
#26259 = CARTESIAN_POINT ( 'NONE',  ( -105.2054292635175585, 21.49321519473984665, 5.610018989487960791E-28 ) ) ;
#26260 = EDGE_LOOP ( 'NONE', ( #8924, #6210, #5847, #20684 ) ) ;
#26261 = CARTESIAN_POINT ( 'NONE',  ( 199.9999999999999432, 17.67867420253430311, -6.969775622007540861 ) ) ;
#26262 = CARTESIAN_POINT ( 'NONE',  ( 189.9999999999999716, 82.50000000000008527, 52.49999999999977973 ) ) ;
#26263 = CARTESIAN_POINT ( 'NONE',  ( -5.866564133101632272, 23.09290806363617676, 42.46617576964622742 ) ) ;
#26264 = EDGE_LOOP ( 'NONE', ( #15394, #7067, #9186, #9956 ) ) ;
#26265 = VERTEX_POINT ( 'NONE', #12681 ) ;
#26266 =( BOUNDED_SURFACE ( )  B_SPLINE_SURFACE ( 3, 3, ( 
 ( #5828, #11941, #18456, #8211, #2238, #373, #13930, #5960, #234, #24330, #6094, #2369, #3977, #14070, #16197, #14201, #16060, #22335, #8077, #12074, #104, #20195, #1843, #1975, #24458, #20593, #26336, #8346, #16467, #7942 ),
 ( #10216, #12336, #2107, #20330, #18322, #24591, #6347, #10081, #20464, #4110, #12209, #4375, #22066, #20067, #9945, #16329, #14335, #18055, #15919, #14466, #18595, #22467, #10346, #22599, #24051, #12465, #10481, #26206, #17125, #2908 ),
 ( #8883, #25256, #19126, #8750, #6879, #4902, #14596, #20861, #2776, #14863, #908, #11016, #23258, #16727, #16866, #18727, #22725, #9021, #21260, #6484, #12605, #5034, #11141, #777, #2645, #22997, #24728, #4504, #7007, #16994 ),
 ( #24998, #10888, #6612, #20734, #13141, #4774, #12878, #18863, #20994, #8477, #644, #19000, #25129, #6751, #14995, #23130, #511, #13012, #15128, #2503, #14730, #21133, #19256, #3032, #8616, #16595, #10614, #24858, #22862, #4639 ),
 ( #12741, #10752, #23884, #13638, #1287, #17759, #3537, #7140, #21764, #9136, #21511, #1167, #9395, #19635, #5661, #11779, #3283, #11381, #5532, #5279, #23505, #25769, #7388, #21632, #17625, #15383, #9654, #7264, #19502, #5159 ),
 ( #23750, #15255, #13384, #3408, #15499, #19760, #11637, #15756, #9270, #17502, #11261, #23385, #1550, #13767, #25388, #13265, #21894, #3671, #1418, #25642, #23629, #25900, #21387, #9519, #3159, #1036, #7519, #15627, #5408, #19380 ),
 ( #17378, #17252, #13509, #25517, #7641, #11509, #24301, #18161, #6069, #3948, #6193, #8315, #15890, #19897, #14171, #26307, #7775, #8186, #10187, #1947, #4081, #20303, #12182, #18429, #22174, #206, #6319, #9787, #1815, #4217 ) ),
 .UNSPECIFIED., .T., .F., .F. ) 
 B_SPLINE_SURFACE_WITH_KNOTS ( ( 4, 3, 4 ),
 ( 4, 2, 2, 2, 2, 2, 2, 2, 2, 2, 2, 2, 2, 2, 4 ),
 ( 0.000000000000000000, 0.5000000000000000000, 1.000000000000000000 ),
 ( 0.000000000000000000, 0.1357259735107005372, 0.1651108541090157700, 0.1944957347073310028, 0.3598804999793158710, 0.3867117631979620773, 0.4135430264166082281, 0.5789277916885930964, 0.6062785021374117456, 0.6336292125862302838, 0.8508620842112317728, 0.8814014469398914198, 0.9119408096685510667, 0.9559704048342755334, 1.000000000000000000 ),
 .UNSPECIFIED. ) 
 GEOMETRIC_REPRESENTATION_ITEM ( )  RATIONAL_B_SPLINE_SURFACE ( (
 ( 1.000000000000000000, 1.000000000000000000, 1.000000000000000000, 1.000000000000000000, 1.000000000000000000, 1.000000000000000000, 1.000000000000000000, 1.000000000000000000, 1.000000000000000000, 1.000000000000000000, 1.000000000000000000, 1.000000000000000000, 1.000000000000000000, 1.000000000000000000, 1.000000000000000000, 1.000000000000000000, 1.000000000000000000, 1.000000000000000000, 1.000000000000000000, 1.000000000000000000, 1.000000000000000000, 1.000000000000000000, 1.000000000000000000, 1.000000000000000000, 1.000000000000000000, 1.000000000000000000, 1.000000000000000000, 1.000000000000000000, 1.000000000000000000, 1.000000000000000000),
 ( 0.3333333333333333703, 0.3333333333333333703, 0.3333333333333333703, 0.3333333333333333703, 0.3333333333333333703, 0.3333333333333333703, 0.3333333333333333703, 0.3333333333333333703, 0.3333333333333333703, 0.3333333333333333703, 0.3333333333333333703, 0.3333333333333333703, 0.3333333333333333703, 0.3333333333333333703, 0.3333333333333333703, 0.3333333333333333703, 0.3333333333333333703, 0.3333333333333333703, 0.3333333333333333703, 0.3333333333333333703, 0.3333333333333333703, 0.3333333333333333703, 0.3333333333333333703, 0.3333333333333333703, 0.3333333333333333703, 0.3333333333333333703, 0.3333333333333333703, 0.3333333333333333703, 0.3333333333333333703, 0.3333333333333333703),
 ( 0.3333333333333333703, 0.3333333333333333703, 0.3333333333333333703, 0.3333333333333333703, 0.3333333333333333703, 0.3333333333333333703, 0.3333333333333333703, 0.3333333333333333703, 0.3333333333333333703, 0.3333333333333333703, 0.3333333333333333703, 0.3333333333333333703, 0.3333333333333333703, 0.3333333333333333703, 0.3333333333333333703, 0.3333333333333333703, 0.3333333333333333703, 0.3333333333333333703, 0.3333333333333333703, 0.3333333333333333703, 0.3333333333333333703, 0.3333333333333333703, 0.3333333333333333703, 0.3333333333333333703, 0.3333333333333333703, 0.3333333333333333703, 0.3333333333333333703, 0.3333333333333333703, 0.3333333333333333703, 0.3333333333333333703),
 ( 1.000000000000000000, 1.000000000000000000, 1.000000000000000000, 1.000000000000000000, 1.000000000000000000, 1.000000000000000000, 1.000000000000000000, 1.000000000000000000, 1.000000000000000000, 1.000000000000000000, 1.000000000000000000, 1.000000000000000000, 1.000000000000000000, 1.000000000000000000, 1.000000000000000000, 1.000000000000000000, 1.000000000000000000, 1.000000000000000000, 1.000000000000000000, 1.000000000000000000, 1.000000000000000000, 1.000000000000000000, 1.000000000000000000, 1.000000000000000000, 1.000000000000000000, 1.000000000000000000, 1.000000000000000000, 1.000000000000000000, 1.000000000000000000, 1.000000000000000000),
 ( 0.3333333333333333703, 0.3333333333333333703, 0.3333333333333333703, 0.3333333333333333703, 0.3333333333333333703, 0.3333333333333333703, 0.3333333333333333703, 0.3333333333333333703, 0.3333333333333333703, 0.3333333333333333703, 0.3333333333333333703, 0.3333333333333333703, 0.3333333333333333703, 0.3333333333333333703, 0.3333333333333333703, 0.3333333333333333703, 0.3333333333333333703, 0.3333333333333333703, 0.3333333333333333703, 0.3333333333333333703, 0.3333333333333333703, 0.3333333333333333703, 0.3333333333333333703, 0.3333333333333333703, 0.3333333333333333703, 0.3333333333333333703, 0.3333333333333333703, 0.3333333333333333703, 0.3333333333333333703, 0.3333333333333333703),
 ( 0.3333333333333333703, 0.3333333333333333703, 0.3333333333333333703, 0.3333333333333333703, 0.3333333333333333703, 0.3333333333333333703, 0.3333333333333333703, 0.3333333333333333703, 0.3333333333333333703, 0.3333333333333333703, 0.3333333333333333703, 0.3333333333333333703, 0.3333333333333333703, 0.3333333333333333703, 0.3333333333333333703, 0.3333333333333333703, 0.3333333333333333703, 0.3333333333333333703, 0.3333333333333333703, 0.3333333333333333703, 0.3333333333333333703, 0.3333333333333333703, 0.3333333333333333703, 0.3333333333333333703, 0.3333333333333333703, 0.3333333333333333703, 0.3333333333333333703, 0.3333333333333333703, 0.3333333333333333703, 0.3333333333333333703),
 ( 1.000000000000000000, 1.000000000000000000, 1.000000000000000000, 1.000000000000000000, 1.000000000000000000, 1.000000000000000000, 1.000000000000000000, 1.000000000000000000, 1.000000000000000000, 1.000000000000000000, 1.000000000000000000, 1.000000000000000000, 1.000000000000000000, 1.000000000000000000, 1.000000000000000000, 1.000000000000000000, 1.000000000000000000, 1.000000000000000000, 1.000000000000000000, 1.000000000000000000, 1.000000000000000000, 1.000000000000000000, 1.000000000000000000, 1.000000000000000000, 1.000000000000000000, 1.000000000000000000, 1.000000000000000000, 1.000000000000000000, 1.000000000000000000, 1.000000000000000000) ) ) 
 REPRESENTATION_ITEM ( '' )  SURFACE ( )  );
#26267 = CARTESIAN_POINT ( 'NONE',  ( 200.0000000000000000, -20.00000000000006750, -40.00000000000002132 ) ) ;
#26268 = CARTESIAN_POINT ( 'NONE',  ( 199.0083412756643497, 0.3136196654984919618, -19.99640146592421175 ) ) ;
#26269 = CARTESIAN_POINT ( 'NONE',  ( -110.0737093975992309, 5.042781230404372650, 19.58505513376282536 ) ) ;
#26270 = SURFACE_STYLE_USAGE ( .BOTH. , #24388 ) ;
#26271 = EDGE_CURVE ( 'NONE', #18983, #12649, #7362, .T. ) ;
#26272 = CARTESIAN_POINT ( 'NONE',  ( -93.01741312765912539, -8.169811846367046826, -20.82169463874099335 ) ) ;
#26273 = CARTESIAN_POINT ( 'NONE',  ( -259.2033419157646676, -1.473088368616265084E-13, 9.517827891722632216 ) ) ;
#26274 = CARTESIAN_POINT ( 'NONE',  ( -259.2033419157646676, -1.473088368616265084E-13, 9.517827891722632216 ) ) ;
#26275 = CARTESIAN_POINT ( 'NONE',  ( -631.0906524188512776, 26.75521908153718798, -29.73521811825018801 ) ) ;
#26276 = CARTESIAN_POINT ( 'NONE',  ( 160.9163046357249129, -135.7889608577475542, 55.61140153332248559 ) ) ;
#26277 = CARTESIAN_POINT ( 'NONE',  ( 199.0247325273615502, -4.232801689760709252, 19.55205092890061280 ) ) ;
#26278 = CARTESIAN_POINT ( 'NONE',  ( -4.027137536850113442, -13.82877337592765699, -46.99492183298336556 ) ) ;
#26279 = CARTESIAN_POINT ( 'NONE',  ( 184.8905102610680444, -13.49065550809791603, -13.49065550809818781 ) ) ;
#26280 = DIRECTION ( 'NONE',  ( -1.000000000000000000, 0.000000000000000000, 0.000000000000000000 ) ) ;
#26281 = CARTESIAN_POINT ( 'NONE',  ( 14.38125909742183062, -67.30136555898262429, 10.73282306405838682 ) ) ;
#26282 = CARTESIAN_POINT ( 'NONE',  ( 170.2234770963711128, -40.00000000000024158, 24.55285855007145202 ) ) ;
#26283 = CARTESIAN_POINT ( 'NONE',  ( 14.38125909742181285, -10.73282306404712472, -10.73282306404731301 ) ) ;
#26284 = CARTESIAN_POINT ( 'NONE',  ( -208.1127848780264742, -55.00245453010926866, 40.00000000000002132 ) ) ;
#26285 = CARTESIAN_POINT ( 'NONE',  ( -215.0000000000000284, 75.52305771588336825, -68.47933392563552957 ) ) ;
#26286 = CARTESIAN_POINT ( 'NONE',  ( 19.06497207195982924, -54.19242893257843008, -2.449293598294708485E-15 ) ) ;
#26287 = CARTESIAN_POINT ( 'NONE',  ( -110.0730399734196254, 10.33436089318840523, 17.33982166920115375 ) ) ;
#26288 = CARTESIAN_POINT ( 'NONE',  ( -259.2033419157646676, 40.00000000000029843, -30.48217210827696988 ) ) ;
#26289 = CARTESIAN_POINT ( 'NONE',  ( -280.0000000000000568, 14.14213562373097943, -42.42640687119285303 ) ) ;
#26290 = CARTESIAN_POINT ( 'NONE',  ( 184.8905102610680444, 19.07866798485562398, -40.00000000000002132 ) ) ;
#26291 = EDGE_LOOP ( 'NONE', ( #12660, #17964, #2127, #14908 ) ) ;
#26292 = ORIENTED_EDGE ( 'NONE', *, *, #25415, .T. ) ;
#26293 = CARTESIAN_POINT ( 'NONE',  ( -91.56559293963834989, -22.67402823373193499, 40.00000000000002132 ) ) ;
#26294 = CARTESIAN_POINT ( 'NONE',  ( 170.0000000000001421, 9.369682556672135121, 22.62041470344889760 ) ) ;
#26295 = CARTESIAN_POINT ( 'NONE',  ( -192.9588430854690273, -40.00000000000024158, 54.46834944101708231 ) ) ;
#26296 = CARTESIAN_POINT ( 'NONE',  ( -105.3755690713226727, -15.38646221621807619, 15.38646221621768362 ) ) ;
#26297 = CARTESIAN_POINT ( 'NONE',  ( 163.1118516004056573, -2.556006622855449647E-13, 27.26290988616872824 ) ) ;
#26298 = CARTESIAN_POINT ( 'NONE',  ( -190.6721700386037526, -43.63442057298705379, -23.91541588165668131 ) ) ;
#26299 = CARTESIAN_POINT ( 'NONE',  ( 199.0053211804427633, 14.13331159297750617, -14.14343255912447361 ) ) ;
#26300 = CARTESIAN_POINT ( 'NONE',  ( 199.9999999999998863, 18.97179924413623908, -1.226483293096950700 ) ) ;
#26301 = CARTESIAN_POINT ( 'NONE',  ( 199.9999999999999147, -17.95406390809352004, -6.253787172257868399 ) ) ;
#26302 = CARTESIAN_POINT ( 'NONE',  ( -198.0356074513804572, 39.15871834505956173, -39.15871834505865223 ) ) ;
#26303 = CARTESIAN_POINT ( 'NONE',  ( -100.7734535825088500, -40.53558337403692491, 16.03295912088671571 ) ) ;
#26304 = CARTESIAN_POINT ( 'NONE',  ( -110.1011157335593396, 20.18087853521583241, 1.497753828917178565 ) ) ;
#26305 = CARTESIAN_POINT ( 'NONE',  ( -135.8532207217289738, -1.208299557080134822E-13, 9.153146818113572891 ) ) ;
#26306 = CARTESIAN_POINT ( 'NONE',  ( 136.1360204305621551, -31.79587985999279454, 24.77266263493094911 ) ) ;
#26307 = CARTESIAN_POINT ( 'NONE',  ( 0.2972598230769938343, 10.13633138497486286, -10.13633138497461594 ) ) ;
#26308 = CARTESIAN_POINT ( 'NONE',  ( -198.0356074513804572, 10.87444709759730088, -10.87444709759707173 ) ) ;
#26309 = CARTESIAN_POINT ( 'NONE',  ( -213.1075012329537230, -66.26714140138676612, 9.698598906462487790 ) ) ;
#26310 = CARTESIAN_POINT ( 'NONE',  ( 200.0000000000000000, -66.50000000000001421, -66.50000000000005684 ) ) ;
#26311 = AXIS2_PLACEMENT_3D ( 'NONE', #4572, #19187, #9074 ) ;
#26313 = CARTESIAN_POINT ( 'NONE',  ( 91.82158438592156813, 39.99999999999995737, 22.79471317813484887 ) ) ;
#26312 = CARTESIAN_POINT ( 'NONE',  ( -213.1075012329537230, 37.98287015391280619, -37.98287015391192512 ) ) ;
#26314 = CARTESIAN_POINT ( 'NONE',  ( 57.59792236341147031, 1.722363176415040886, 1.722363176415060426 ) ) ;
#26315 = CARTESIAN_POINT ( 'NONE',  ( 17.24092899315852279, 44.34059580269009615, -18.36647614519047522 ) ) ;
#26316 = CARTESIAN_POINT ( 'NONE',  ( -56.48582580120559982, 30.84685318188643777, -40.00000000000002132 ) ) ;
#26318 = EDGE_CURVE ( 'NONE', #21399, #87, #10433, .T. ) ;
#26317 = EDGE_LOOP ( 'NONE', ( #21181, #14605, #11148, #8536 ) ) ;
#26319 = CARTESIAN_POINT ( 'NONE',  ( -213.1075012329537230, 13.71589010951907994, 0.000000000000000000 ) ) ;
#26320 = CARTESIAN_POINT ( 'NONE',  ( -3.524834090818314891, -43.28235980537091621, 17.92814044289653097 ) ) ;
#26321 = CARTESIAN_POINT ( 'NONE',  ( -135.8532207217289738, -9.153146818113595984, 40.00000000000002132 ) ) ;
#26322 = ORIENTED_EDGE ( 'NONE', *, *, #7759, .T. ) ;
#26323 = CARTESIAN_POINT ( 'NONE',  ( -194.4222775679849917, -44.35790405182654439, 24.44979664542841391 ) ) ;
#26324 = CARTESIAN_POINT ( 'NONE',  ( 200.0000000000001990, -15.46007656673369368, 11.06691610098113543 ) ) ;
#26325 = CARTESIAN_POINT ( 'NONE',  ( 21.45050411887960706, -18.02367319545413693, 43.51299627226052280 ) ) ;
#26326 = ADVANCED_FACE ( 'NONE', ( #13330 ), #25626, .T. ) ;
#26327 = EDGE_CURVE ( 'NONE', #23049, #17205, #16368, .T. ) ;
#26328 = CARTESIAN_POINT ( 'NONE',  ( 22.92196489052082953, 23.44087486047551394, -42.99364193793545041 ) ) ;
#26329 = CARTESIAN_POINT ( 'NONE',  ( 199.0122387307937686, -8.258478517853962586, -18.21619819090958714 ) ) ;
#26330 = CIRCLE ( 'NONE', #3792, 5.000000000000004441 ) ;
#26331 = DIRECTION ( 'NONE',  ( 1.836970198721030181E-16, -1.000000000000000000, 0.000000000000000000 ) ) ;
#26332 = CARTESIAN_POINT ( 'NONE',  ( -144.0562696876083066, -14.68019673967120120, 29.54283206236174664 ) ) ;
#26333 = CARTESIAN_POINT ( 'NONE',  ( 136.1360204305621266, 3.511608612530757068, -3.511608612530642937 ) ) ;
#26334 = CARTESIAN_POINT ( 'NONE',  ( 14.38125909742181285, -15.17850393972633505, 0.000000000000000000 ) ) ;
#26336 = CARTESIAN_POINT ( 'NONE',  ( 170.2234770963711128, -17.36149277827010096, 17.36149277826970660 ) ) ;
#26335 = CARTESIAN_POINT ( 'NONE',  ( -192.9370379451880240, 14.03127537977120909, -48.35015161801996442 ) ) ;
#26337 = DIRECTION ( 'NONE',  ( 0.000000000000000000, -0.9767746502210203907, 0.2142691827715860198 ) ) ;
#26338 = CARTESIAN_POINT ( 'NONE',  ( 14.38125909742182884, -55.17850393971007605, 40.00000000000002132 ) ) ;
#26339 = CARTESIAN_POINT ( 'NONE',  ( 4.995406935893288214, 55.24977328854835434, 2.449293598294708485E-15 ) ) ;
#26340 = CARTESIAN_POINT ( 'NONE',  ( -105.3755690713226727, 1.741486606973311632E-13, -18.24025645688352881 ) ) ;
#26341 = CARTESIAN_POINT ( 'NONE',  ( -86.96347745069644475, 41.18208027870598187, -15.38646221621779731 ) ) ;
#26342 = FACE_OUTER_BOUND ( 'NONE', #10399, .T. ) ;
#26343 = PRODUCT_DEFINITION_SHAPE ( 'NONE', 'NONE',  #26357 ) ;
#26344 = FACE_OUTER_BOUND ( 'NONE', #19324, .T. ) ;
#26345 = EDGE_LOOP ( 'NONE', ( #25600, #12163 ) ) ;
#26346 = CARTESIAN_POINT ( 'NONE',  ( -280.0000000000000568, -14.14213562373108601, 42.42640687119285303 ) ) ;
#26347 = CARTESIAN_POINT ( 'NONE',  ( -103.9663809733797990, -8.026122152273305943, 20.15238534308313589 ) ) ;
#26348 = PRODUCT_CONTEXT ( 'NONE', #17728, 'mechanical' ) ;
#26349 = ORIENTED_EDGE ( 'NONE', *, *, #7991, .T. ) ;
#26350 = EDGE_LOOP ( 'NONE', ( #22647, #18912, #4092, #21310 ) ) ;
#26351 = CARTESIAN_POINT ( 'NONE',  ( 163.1118516004056573, -9.006482792073960297, -47.56205970284963769 ) ) ;
#26352 = CARTESIAN_POINT ( 'NONE',  ( 83.11963132834678447, -24.42551322420066384, -9.001241435739066432 ) ) ;
#26353 = CARTESIAN_POINT ( 'NONE',  ( 163.1118516004056573, -40.00000000000003553, 12.73709011382460687 ) ) ;
#26354 = NEXT_ASSEMBLY_USAGE_OCCURRENCE ( 'NAUO1', ' ', ' ', #10140, #1112, $ ) ;
#26355 = NEXT_ASSEMBLY_USAGE_OCCURRENCE ( 'NAUO2', ' ', ' ', #10140, #17991, $ ) ;
#26356 = NEXT_ASSEMBLY_USAGE_OCCURRENCE ( 'NAUO3', ' ', ' ', #10140, #14914, $ ) ;
#26357 = NEXT_ASSEMBLY_USAGE_OCCURRENCE ( 'NAUO4', ' ', ' ', #10140, #25182, $ ) ;
#26358 = NEXT_ASSEMBLY_USAGE_OCCURRENCE ( 'NAUO5', ' ', ' ', #10140, #11592, $ ) ;
#26359 = NEXT_ASSEMBLY_USAGE_OCCURRENCE ( 'NAUO6', ' ', ' ', #10140, #6229, $ ) ;
#26360 = NEXT_ASSEMBLY_USAGE_OCCURRENCE ( 'NAUO7', ' ', ' ', #10140, #8176, $ ) ;
#26361 = NEXT_ASSEMBLY_USAGE_OCCURRENCE ( 'NAUO8', ' ', ' ', #10140, #17594, $ ) ;
#26362 = NEXT_ASSEMBLY_USAGE_OCCURRENCE ( 'NAUO9', ' ', ' ', #10140, #8176, $ ) ;
#26363 = NEXT_ASSEMBLY_USAGE_OCCURRENCE ( 'NAUO10', ' ', ' ', #10140, #8176, $ ) ;
#26364 = NEXT_ASSEMBLY_USAGE_OCCURRENCE ( 'NAUO11', ' ', ' ', #10140, #8176, $ ) ;
#26365 = NEXT_ASSEMBLY_USAGE_OCCURRENCE ( 'NAUO12', ' ', ' ', #10140, #11592, $ ) ;
#26366 = NEXT_ASSEMBLY_USAGE_OCCURRENCE ( 'NAUO13', ' ', ' ', #10140, #11592, $ ) ;
#26367 = NEXT_ASSEMBLY_USAGE_OCCURRENCE ( 'NAUO14', ' ', ' ', #10140, #17594, $ ) ;
#26368=COLOUR_RGB('Dark Blue',0.08,0.2,0.34);
#26369=FILL_AREA_STYLE_COLOUR('',#26368);
#26370=FILL_AREA_STYLE('',(#26369));
#26371=SURFACE_STYLE_FILL_AREA(#26370);
#26372=SURFACE_SIDE_STYLE('',(#26371));
#26373=SURFACE_STYLE_USAGE(.BOTH.,#26372);
#26374=PRESENTATION_STYLE_ASSIGNMENT((#26373));
#26375=COLOUR_RGB('Light Blue',0.38,0.62,0.78);
#26376=FILL_AREA_STYLE_COLOUR('',#26375);
#26377=FILL_AREA_STYLE('',(#26376));
#26378=SURFACE_STYLE_FILL_AREA(#26377);
#26379=SURFACE_SIDE_STYLE('',(#26378));
#26380=SURFACE_STYLE_USAGE(.BOTH.,#26379);
#26381=PRESENTATION_STYLE_ASSIGNMENT((#26380));
#26382=COLOUR_RGB('Sky Blue',0.24,0.69,0.87);
#26383=FILL_AREA_STYLE_COLOUR('',#26382);
#26384=FILL_AREA_STYLE('',(#26383));
#26385=SURFACE_STYLE_FILL_AREA(#26384);
#26386=SURFACE_SIDE_STYLE('',(#26385));
#26387=SURFACE_STYLE_USAGE(.BOTH.,#26386);
#26388=PRESENTATION_STYLE_ASSIGNMENT((#26387));
#26389=COLOUR_RGB('Grey',0.48,0.52,0.57);
#26390=FILL_AREA_STYLE_COLOUR('',#26389);
#26391=FILL_AREA_STYLE('',(#26390));
#26392=SURFACE_STYLE_FILL_AREA(#26391);
#26393=SURFACE_SIDE_STYLE('',(#26392));
#26394=SURFACE_STYLE_USAGE(.BOTH.,#26393);
#26395=PRESENTATION_STYLE_ASSIGNMENT((#26394));
#26396=COLOUR_RGB('Black',0.12,0.14,0.17);
#26397=FILL_AREA_STYLE_COLOUR('',#26396);
#26398=FILL_AREA_STYLE('',(#26397));
#26399=SURFACE_STYLE_FILL_AREA(#26398);
#26400=SURFACE_SIDE_STYLE('',(#26399));
#26401=SURFACE_STYLE_USAGE(.BOTH.,#26400);
#26402=PRESENTATION_STYLE_ASSIGNMENT((#26401));
#26403=COLOUR_RGB('Off White',0.89,0.88,0.83);
#26404=FILL_AREA_STYLE_COLOUR('',#26403);
#26405=FILL_AREA_STYLE('',(#26404));
#26406=SURFACE_STYLE_FILL_AREA(#26405);
#26407=SURFACE_SIDE_STYLE('',(#26406));
#26408=SURFACE_STYLE_USAGE(.BOTH.,#26407);
#26409=PRESENTATION_STYLE_ASSIGNMENT((#26408));
ENDSEC;
END-ISO-10303-21;
